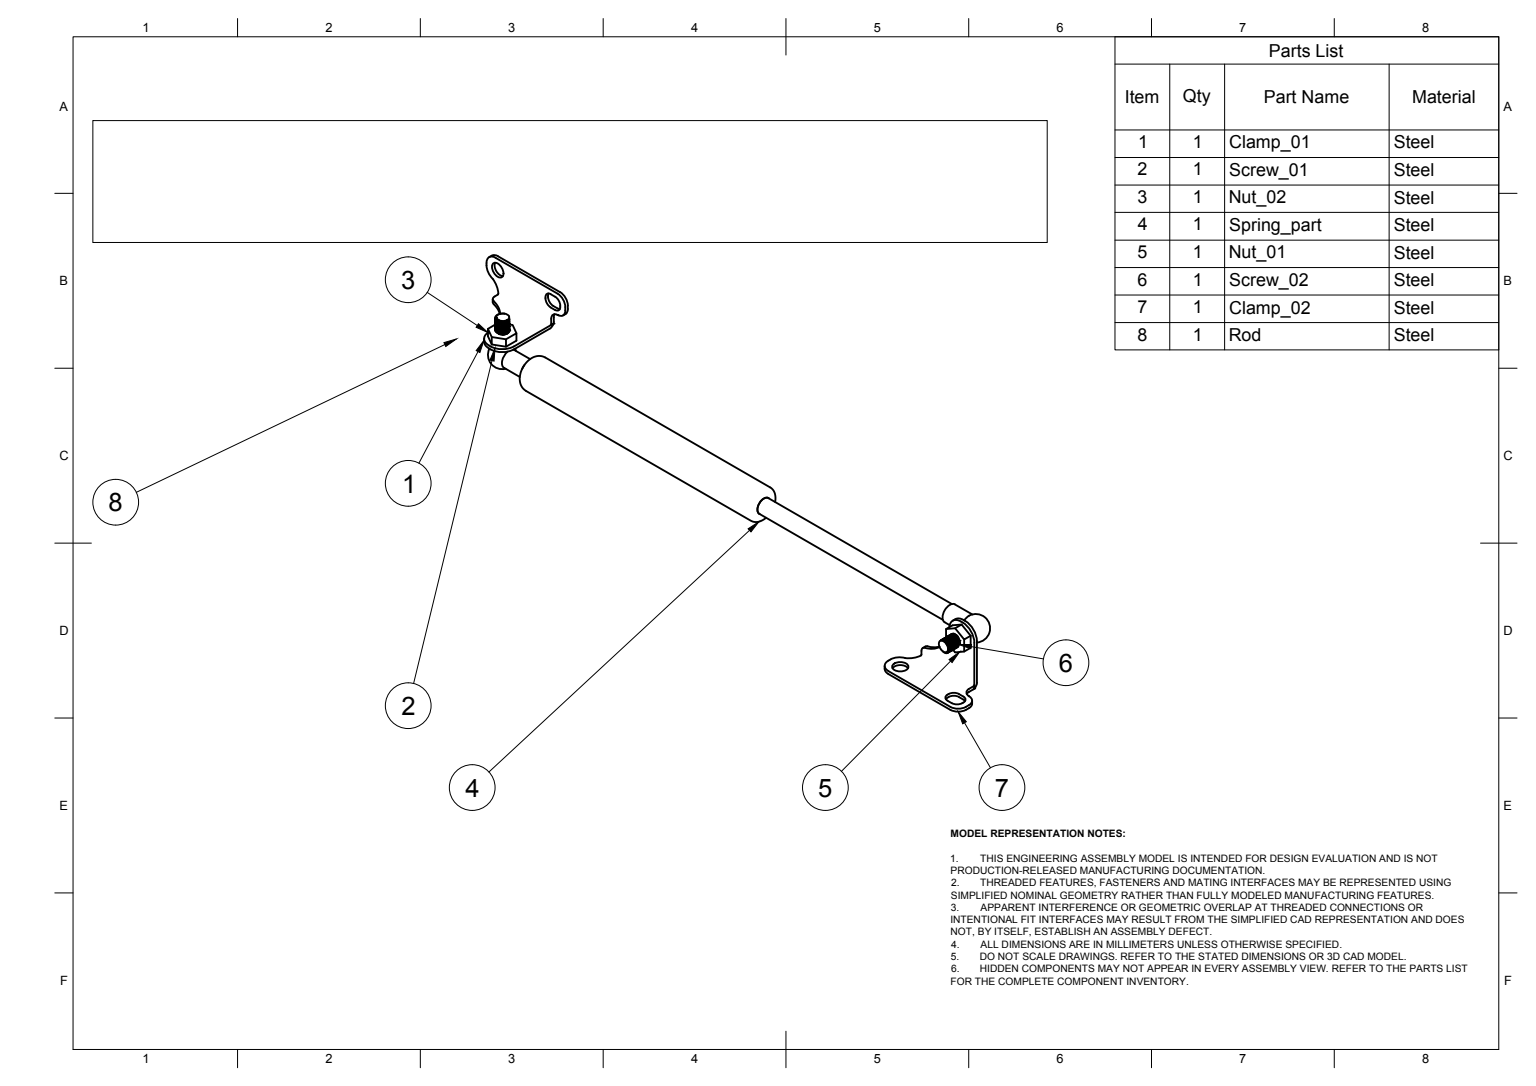
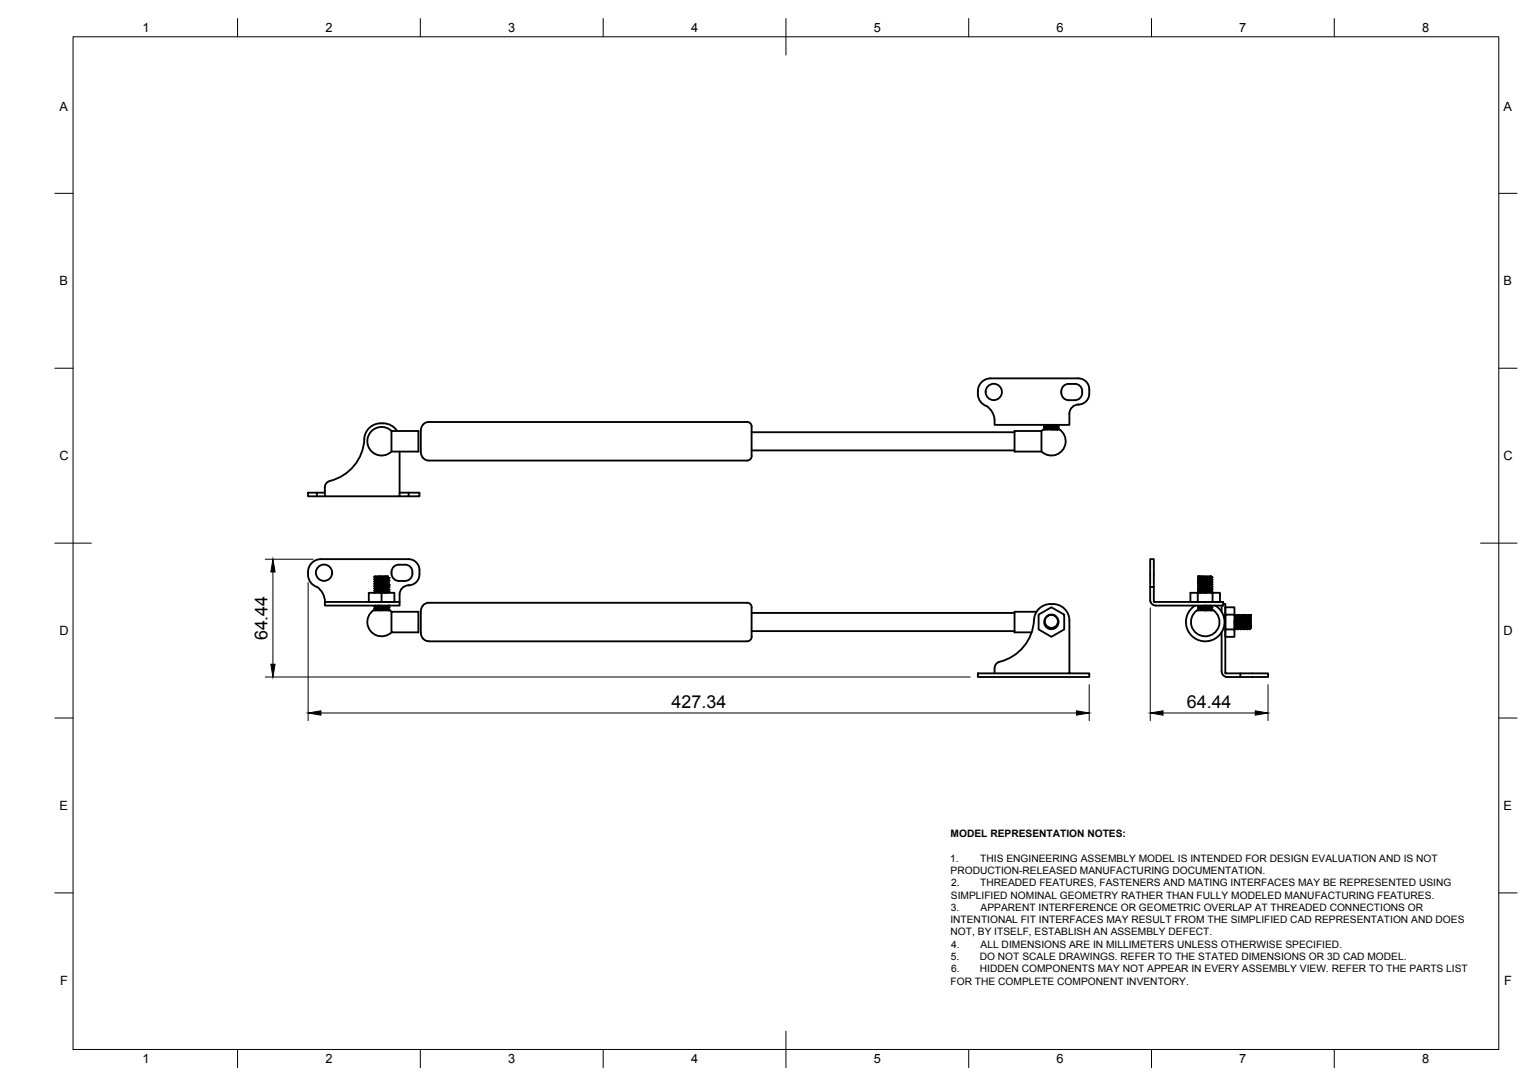
ISO-10303-21;
HEADER;
/* Generated by software containing ST-Developer
 * from STEP Tools, Inc. (www.steptools.com) 
 */

FILE_DESCRIPTION(
/* description */ (''),
/* implementation_level */ '2;1');

FILE_NAME(
/* name */ 'BR-107',
/* time_stamp */ '2026-10-04T16:49:01-07:00',
/* author */ (''),
/* organization */ (''),
/* preprocessor_version */ 'ST-DEVELOPER v20.2',
/* originating_system */ 'Autodesk Translation Framework v15.15.0.0',
/* authorisation */ '');

FILE_SCHEMA (('AUTOMOTIVE_DESIGN { 1 0 10303 214 3 1 1 }'));
ENDSEC;

DATA;
#10=MECHANICAL_DESIGN_GEOMETRIC_PRESENTATION_REPRESENTATION('',(#80,#81,
#82,#83,#84,#85,#86,#87,#88),#51553);
#11=ITEM_DEFINED_TRANSFORMATION($,$,#4358,#4663);
#12=ITEM_DEFINED_TRANSFORMATION($,$,#4430,#4664);
#13=ITEM_DEFINED_TRANSFORMATION($,$,#4466,#4665);
#14=ITEM_DEFINED_TRANSFORMATION($,$,#4489,#4666);
#15=ITEM_DEFINED_TRANSFORMATION($,$,#4507,#4667);
#16=ITEM_DEFINED_TRANSFORMATION($,$,#4530,#4668);
#17=ITEM_DEFINED_TRANSFORMATION($,$,#4559,#4669);
#18=ITEM_DEFINED_TRANSFORMATION($,$,#4631,#4670);
#19=(
REPRESENTATION_RELATIONSHIP($,$,#51585,#51584)
REPRESENTATION_RELATIONSHIP_WITH_TRANSFORMATION(#11)
SHAPE_REPRESENTATION_RELATIONSHIP()
);
#20=(
REPRESENTATION_RELATIONSHIP($,$,#51586,#51584)
REPRESENTATION_RELATIONSHIP_WITH_TRANSFORMATION(#12)
SHAPE_REPRESENTATION_RELATIONSHIP()
);
#21=(
REPRESENTATION_RELATIONSHIP($,$,#51587,#51584)
REPRESENTATION_RELATIONSHIP_WITH_TRANSFORMATION(#13)
SHAPE_REPRESENTATION_RELATIONSHIP()
);
#22=(
REPRESENTATION_RELATIONSHIP($,$,#51588,#51584)
REPRESENTATION_RELATIONSHIP_WITH_TRANSFORMATION(#14)
SHAPE_REPRESENTATION_RELATIONSHIP()
);
#23=(
REPRESENTATION_RELATIONSHIP($,$,#51589,#51584)
REPRESENTATION_RELATIONSHIP_WITH_TRANSFORMATION(#15)
SHAPE_REPRESENTATION_RELATIONSHIP()
);
#24=(
REPRESENTATION_RELATIONSHIP($,$,#51590,#51584)
REPRESENTATION_RELATIONSHIP_WITH_TRANSFORMATION(#16)
SHAPE_REPRESENTATION_RELATIONSHIP()
);
#25=(
REPRESENTATION_RELATIONSHIP($,$,#51591,#51584)
REPRESENTATION_RELATIONSHIP_WITH_TRANSFORMATION(#17)
SHAPE_REPRESENTATION_RELATIONSHIP()
);
#26=(
REPRESENTATION_RELATIONSHIP($,$,#51592,#51584)
REPRESENTATION_RELATIONSHIP_WITH_TRANSFORMATION(#18)
SHAPE_REPRESENTATION_RELATIONSHIP()
);
#27=CONTEXT_DEPENDENT_SHAPE_REPRESENTATION(#19,#51576);
#28=CONTEXT_DEPENDENT_SHAPE_REPRESENTATION(#20,#51577);
#29=CONTEXT_DEPENDENT_SHAPE_REPRESENTATION(#21,#51578);
#30=CONTEXT_DEPENDENT_SHAPE_REPRESENTATION(#22,#51579);
#31=CONTEXT_DEPENDENT_SHAPE_REPRESENTATION(#23,#51580);
#32=CONTEXT_DEPENDENT_SHAPE_REPRESENTATION(#24,#51581);
#33=CONTEXT_DEPENDENT_SHAPE_REPRESENTATION(#25,#51582);
#34=CONTEXT_DEPENDENT_SHAPE_REPRESENTATION(#26,#51583);
#35=NEXT_ASSEMBLY_USAGE_OCCURRENCE('Clamp_01:1','Clamp_01:1',
'Clamp_01:1',#51594,#51595,'Clamp_01:1');
#36=NEXT_ASSEMBLY_USAGE_OCCURRENCE('Screw_01:1','Screw_01:1',
'Screw_01:1',#51594,#51596,'Screw_01:1');
#37=NEXT_ASSEMBLY_USAGE_OCCURRENCE('Nut_02:1','Nut_02:1','Nut_02:1',#51594,
#51597,'Nut_02:1');
#38=NEXT_ASSEMBLY_USAGE_OCCURRENCE('Spring_part:1','Spring_part:1',
'Spring_part:1',#51594,#51598,'Spring_part:1');
#39=NEXT_ASSEMBLY_USAGE_OCCURRENCE('Nut_01:1','Nut_01:1','Nut_01:1',#51594,
#51599,'Nut_01:1');
#40=NEXT_ASSEMBLY_USAGE_OCCURRENCE('Screw_02:1','Screw_02:1',
'Screw_02:1',#51594,#51600,'Screw_02:1');
#41=NEXT_ASSEMBLY_USAGE_OCCURRENCE('Clamp_02:1','Clamp_02:1',
'Clamp_02:1',#51594,#51601,'Clamp_02:1');
#42=NEXT_ASSEMBLY_USAGE_OCCURRENCE('Rod:1','Rod:1','Rod:1',#51594,#51602,
'Rod:1');
#43=SPHERICAL_SURFACE('',#4646,7.81234603703673);
#44=SPHERICAL_SURFACE('',#4651,7.81234603703673);
#45=TOROIDAL_SURFACE('',#4496,8.03882147643231,2.49999999999996);
#46=TOROIDAL_SURFACE('',#4502,5.78096926885271,5.05765846207533);
#47=TOROIDAL_SURFACE('',#4505,6.2888214764323,4.24999999999998);
#48=B_SPLINE_SURFACE_WITH_KNOTS('',3,3,((#17982,#17983,#17984,#17985,#17986,
#17987,#17988,#17989,#17990,#17991,#17992,#17993,#17994,#17995,#17996,#17997,
#17998,#17999,#18000,#18001,#18002,#18003,#18004,#18005,#18006,#18007,#18008,
#18009,#18010,#18011,#18012,#18013,#18014,#18015,#18016,#18017,#18018,#18019,
#18020,#18021,#18022,#18023,#18024,#18025,#18026,#18027,#18028,#18029,#18030,
#18031,#18032,#18033,#18034,#18035,#18036,#18037,#18038,#18039,#18040,#18041,
#18042,#18043,#18044,#18045,#18046,#18047,#18048,#18049,#18050,#18051,#18052,
#18053,#18054,#18055,#18056,#18057,#18058,#18059,#18060,#18061,#18062,#18063,
#18064,#18065,#18066,#18067,#18068,#18069,#18070,#18071,#18072,#18073,#18074,
#18075,#18076,#18077,#18078,#18079,#18080,#18081,#18082,#18083,#18084,#18085,
#18086,#18087,#18088,#18089,#18090,#18091,#18092,#18093,#18094,#18095,#18096,
#18097,#18098,#18099,#18100,#18101,#18102,#18103,#18104,#18105,#18106,#18107,
#18108,#18109,#18110,#18111,#18112),(#18113,#18114,#18115,#18116,#18117,
#18118,#18119,#18120,#18121,#18122,#18123,#18124,#18125,#18126,#18127,#18128,
#18129,#18130,#18131,#18132,#18133,#18134,#18135,#18136,#18137,#18138,#18139,
#18140,#18141,#18142,#18143,#18144,#18145,#18146,#18147,#18148,#18149,#18150,
#18151,#18152,#18153,#18154,#18155,#18156,#18157,#18158,#18159,#18160,#18161,
#18162,#18163,#18164,#18165,#18166,#18167,#18168,#18169,#18170,#18171,#18172,
#18173,#18174,#18175,#18176,#18177,#18178,#18179,#18180,#18181,#18182,#18183,
#18184,#18185,#18186,#18187,#18188,#18189,#18190,#18191,#18192,#18193,#18194,
#18195,#18196,#18197,#18198,#18199,#18200,#18201,#18202,#18203,#18204,#18205,
#18206,#18207,#18208,#18209,#18210,#18211,#18212,#18213,#18214,#18215,#18216,
#18217,#18218,#18219,#18220,#18221,#18222,#18223,#18224,#18225,#18226,#18227,
#18228,#18229,#18230,#18231,#18232,#18233,#18234,#18235,#18236,#18237,#18238,
#18239,#18240,#18241,#18242,#18243),(#18244,#18245,#18246,#18247,#18248,
#18249,#18250,#18251,#18252,#18253,#18254,#18255,#18256,#18257,#18258,#18259,
#18260,#18261,#18262,#18263,#18264,#18265,#18266,#18267,#18268,#18269,#18270,
#18271,#18272,#18273,#18274,#18275,#18276,#18277,#18278,#18279,#18280,#18281,
#18282,#18283,#18284,#18285,#18286,#18287,#18288,#18289,#18290,#18291,#18292,
#18293,#18294,#18295,#18296,#18297,#18298,#18299,#18300,#18301,#18302,#18303,
#18304,#18305,#18306,#18307,#18308,#18309,#18310,#18311,#18312,#18313,#18314,
#18315,#18316,#18317,#18318,#18319,#18320,#18321,#18322,#18323,#18324,#18325,
#18326,#18327,#18328,#18329,#18330,#18331,#18332,#18333,#18334,#18335,#18336,
#18337,#18338,#18339,#18340,#18341,#18342,#18343,#18344,#18345,#18346,#18347,
#18348,#18349,#18350,#18351,#18352,#18353,#18354,#18355,#18356,#18357,#18358,
#18359,#18360,#18361,#18362,#18363,#18364,#18365,#18366,#18367,#18368,#18369,
#18370,#18371,#18372,#18373,#18374),(#18375,#18376,#18377,#18378,#18379,
#18380,#18381,#18382,#18383,#18384,#18385,#18386,#18387,#18388,#18389,#18390,
#18391,#18392,#18393,#18394,#18395,#18396,#18397,#18398,#18399,#18400,#18401,
#18402,#18403,#18404,#18405,#18406,#18407,#18408,#18409,#18410,#18411,#18412,
#18413,#18414,#18415,#18416,#18417,#18418,#18419,#18420,#18421,#18422,#18423,
#18424,#18425,#18426,#18427,#18428,#18429,#18430,#18431,#18432,#18433,#18434,
#18435,#18436,#18437,#18438,#18439,#18440,#18441,#18442,#18443,#18444,#18445,
#18446,#18447,#18448,#18449,#18450,#18451,#18452,#18453,#18454,#18455,#18456,
#18457,#18458,#18459,#18460,#18461,#18462,#18463,#18464,#18465,#18466,#18467,
#18468,#18469,#18470,#18471,#18472,#18473,#18474,#18475,#18476,#18477,#18478,
#18479,#18480,#18481,#18482,#18483,#18484,#18485,#18486,#18487,#18488,#18489,
#18490,#18491,#18492,#18493,#18494,#18495,#18496,#18497,#18498,#18499,#18500,
#18501,#18502,#18503,#18504,#18505)),.UNSPECIFIED.,.F.,.F.,.F.,(4,4),(4,
1,1,1,1,1,1,1,1,1,1,1,1,1,1,1,1,1,1,1,1,1,1,1,1,1,1,1,1,1,1,1,1,1,1,1,1,
1,1,1,1,1,1,1,1,1,1,1,1,1,1,1,1,1,1,1,1,1,1,1,1,1,1,1,1,1,1,1,1,1,1,1,1,
1,1,1,1,1,1,1,1,1,1,1,1,1,1,1,1,1,1,1,1,1,1,1,1,1,1,1,1,1,1,1,1,1,1,1,1,
1,1,1,1,1,1,1,1,1,1,1,1,1,1,1,1,1,1,1,4),(-0.000314077148181808,0.0826777824702824),
(11.6145490510227,12.613065069482,13.6109159112094,14.6087667529368,15.6066175946642,
16.6044684363917,17.6023192781191,18.6001701198465,19.5980209615739,20.5958718033013,
21.5937226450287,22.5915734867561,23.5894243284835,24.5872751702109,25.5851260119383,
26.5829768536657,27.5808276953931,28.5786785371205,29.5765293788479,30.5743802205753,
31.5722310623027,32.5700819040301,33.5679327457575,34.5657835874849,35.5636344292123,
36.5614852709397,37.5593361126671,38.5571869543945,39.5550377961219,40.5528886378493,
41.5507394795767,42.5485903213041,43.5464411630315,44.5442920047589,45.5421428464863,
46.5399936882137,47.5378445299411,48.5356953716685,49.5335462133959,50.5313970551233,
51.5292478968507,52.5270987385781,53.5249495803055,54.522800422033,55.5206512637604,
56.5185021054878,57.5163529472152,58.5142037889426,59.51205463067,60.5099054723974,
61.5077563141248,62.5056071558522,63.5034579975796,64.501308839307,65.4991596810344,
66.4970105227618,67.4948613644892,68.4927122062166,69.490563047944,70.4884138896714,
71.4862647313988,72.4841155731262,73.4819664148536,74.479817256581,75.4776680983084,
76.4755189400358,77.4733697817632,78.4712206234906,79.469071465218,80.4669223069454,
81.4647731486728,82.4626239904002,83.4604748321276,84.458325673855,85.4561765155824,
86.4540273573098,87.4518781990372,88.4497290407646,89.4475798824921,90.4454307242194,
91.4432815659468,92.4411324076742,93.4389832494017,94.4368340911291,95.4346849328565,
96.4325357745839,97.4303866163113,98.4282374580387,99.4260882997661,100.423939141493,
101.421789983221,102.419640824948,103.417491666676,104.415342508403,105.41319335013,
106.411044191858,107.408895033585,108.406745875313,109.40459671704,110.402447558768,
111.400298400495,112.398149242222,113.39600008395,114.393850925677,115.391701767405,
116.389552609132,117.387403450859,118.385254292587,119.383105134314,120.380955976042,
121.378806817769,122.376657659496,123.374508501224,124.372359342951,125.370210184679,
126.368061026406,127.365911868133,128.363762709861,129.361613551588,130.359464393316,
131.357315235043,132.35516607677,133.353016918498,134.350867760225,135.348718601953,
136.34656944368,137.344420285407,138.342271127135,139.340121968862),
 .UNSPECIFIED.);
#49=B_SPLINE_SURFACE_WITH_KNOTS('',3,3,((#18820,#18821,#18822,#18823,#18824,
#18825,#18826,#18827,#18828,#18829,#18830,#18831,#18832,#18833,#18834,#18835,
#18836,#18837,#18838,#18839,#18840,#18841,#18842,#18843,#18844,#18845,#18846,
#18847,#18848,#18849,#18850,#18851,#18852,#18853,#18854,#18855,#18856,#18857,
#18858,#18859,#18860,#18861,#18862,#18863,#18864,#18865,#18866,#18867,#18868,
#18869,#18870,#18871,#18872,#18873,#18874,#18875,#18876,#18877,#18878,#18879,
#18880,#18881,#18882,#18883,#18884,#18885,#18886,#18887,#18888,#18889,#18890,
#18891,#18892,#18893,#18894,#18895,#18896,#18897,#18898,#18899,#18900,#18901,
#18902,#18903,#18904,#18905,#18906,#18907,#18908,#18909,#18910,#18911,#18912,
#18913,#18914,#18915,#18916,#18917,#18918,#18919,#18920,#18921,#18922,#18923,
#18924,#18925,#18926,#18927,#18928,#18929,#18930,#18931,#18932,#18933,#18934,
#18935,#18936,#18937,#18938,#18939,#18940,#18941,#18942,#18943,#18944,#18945,
#18946,#18947,#18948,#18949,#18950),(#18951,#18952,#18953,#18954,#18955,
#18956,#18957,#18958,#18959,#18960,#18961,#18962,#18963,#18964,#18965,#18966,
#18967,#18968,#18969,#18970,#18971,#18972,#18973,#18974,#18975,#18976,#18977,
#18978,#18979,#18980,#18981,#18982,#18983,#18984,#18985,#18986,#18987,#18988,
#18989,#18990,#18991,#18992,#18993,#18994,#18995,#18996,#18997,#18998,#18999,
#19000,#19001,#19002,#19003,#19004,#19005,#19006,#19007,#19008,#19009,#19010,
#19011,#19012,#19013,#19014,#19015,#19016,#19017,#19018,#19019,#19020,#19021,
#19022,#19023,#19024,#19025,#19026,#19027,#19028,#19029,#19030,#19031,#19032,
#19033,#19034,#19035,#19036,#19037,#19038,#19039,#19040,#19041,#19042,#19043,
#19044,#19045,#19046,#19047,#19048,#19049,#19050,#19051,#19052,#19053,#19054,
#19055,#19056,#19057,#19058,#19059,#19060,#19061,#19062,#19063,#19064,#19065,
#19066,#19067,#19068,#19069,#19070,#19071,#19072,#19073,#19074,#19075,#19076,
#19077,#19078,#19079,#19080,#19081),(#19082,#19083,#19084,#19085,#19086,
#19087,#19088,#19089,#19090,#19091,#19092,#19093,#19094,#19095,#19096,#19097,
#19098,#19099,#19100,#19101,#19102,#19103,#19104,#19105,#19106,#19107,#19108,
#19109,#19110,#19111,#19112,#19113,#19114,#19115,#19116,#19117,#19118,#19119,
#19120,#19121,#19122,#19123,#19124,#19125,#19126,#19127,#19128,#19129,#19130,
#19131,#19132,#19133,#19134,#19135,#19136,#19137,#19138,#19139,#19140,#19141,
#19142,#19143,#19144,#19145,#19146,#19147,#19148,#19149,#19150,#19151,#19152,
#19153,#19154,#19155,#19156,#19157,#19158,#19159,#19160,#19161,#19162,#19163,
#19164,#19165,#19166,#19167,#19168,#19169,#19170,#19171,#19172,#19173,#19174,
#19175,#19176,#19177,#19178,#19179,#19180,#19181,#19182,#19183,#19184,#19185,
#19186,#19187,#19188,#19189,#19190,#19191,#19192,#19193,#19194,#19195,#19196,
#19197,#19198,#19199,#19200,#19201,#19202,#19203,#19204,#19205,#19206,#19207,
#19208,#19209,#19210,#19211,#19212),(#19213,#19214,#19215,#19216,#19217,
#19218,#19219,#19220,#19221,#19222,#19223,#19224,#19225,#19226,#19227,#19228,
#19229,#19230,#19231,#19232,#19233,#19234,#19235,#19236,#19237,#19238,#19239,
#19240,#19241,#19242,#19243,#19244,#19245,#19246,#19247,#19248,#19249,#19250,
#19251,#19252,#19253,#19254,#19255,#19256,#19257,#19258,#19259,#19260,#19261,
#19262,#19263,#19264,#19265,#19266,#19267,#19268,#19269,#19270,#19271,#19272,
#19273,#19274,#19275,#19276,#19277,#19278,#19279,#19280,#19281,#19282,#19283,
#19284,#19285,#19286,#19287,#19288,#19289,#19290,#19291,#19292,#19293,#19294,
#19295,#19296,#19297,#19298,#19299,#19300,#19301,#19302,#19303,#19304,#19305,
#19306,#19307,#19308,#19309,#19310,#19311,#19312,#19313,#19314,#19315,#19316,
#19317,#19318,#19319,#19320,#19321,#19322,#19323,#19324,#19325,#19326,#19327,
#19328,#19329,#19330,#19331,#19332,#19333,#19334,#19335,#19336,#19337,#19338,
#19339,#19340,#19341,#19342,#19343)),.UNSPECIFIED.,.F.,.F.,.F.,(4,4),(4,
1,1,1,1,1,1,1,1,1,1,1,1,1,1,1,1,1,1,1,1,1,1,1,1,1,1,1,1,1,1,1,1,1,1,1,1,
1,1,1,1,1,1,1,1,1,1,1,1,1,1,1,1,1,1,1,1,1,1,1,1,1,1,1,1,1,1,1,1,1,1,1,1,
1,1,1,1,1,1,1,1,1,1,1,1,1,1,1,1,1,1,1,1,1,1,1,1,1,1,1,1,1,1,1,1,1,1,1,1,
1,1,1,1,1,1,1,1,1,1,1,1,1,1,1,1,1,1,1,4),(-0.000314077148181808,0.0826777824702824),
(11.6145490510227,12.613065069482,13.6109159112094,14.6087667529368,15.6066175946642,
16.6044684363917,17.6023192781191,18.6001701198465,19.5980209615739,20.5958718033013,
21.5937226450287,22.5915734867561,23.5894243284835,24.5872751702109,25.5851260119383,
26.5829768536657,27.5808276953931,28.5786785371205,29.5765293788479,30.5743802205753,
31.5722310623027,32.5700819040301,33.5679327457575,34.5657835874849,35.5636344292123,
36.5614852709397,37.5593361126671,38.5571869543945,39.5550377961219,40.5528886378493,
41.5507394795767,42.5485903213041,43.5464411630315,44.5442920047589,45.5421428464863,
46.5399936882137,47.5378445299411,48.5356953716685,49.5335462133959,50.5313970551233,
51.5292478968507,52.5270987385781,53.5249495803055,54.522800422033,55.5206512637604,
56.5185021054878,57.5163529472152,58.5142037889426,59.51205463067,60.5099054723974,
61.5077563141248,62.5056071558522,63.5034579975796,64.501308839307,65.4991596810344,
66.4970105227618,67.4948613644892,68.4927122062166,69.490563047944,70.4884138896714,
71.4862647313988,72.4841155731262,73.4819664148536,74.479817256581,75.4776680983084,
76.4755189400358,77.4733697817632,78.4712206234906,79.469071465218,80.4669223069454,
81.4647731486728,82.4626239904002,83.4604748321276,84.458325673855,85.4561765155824,
86.4540273573098,87.4518781990372,88.4497290407646,89.4475798824921,90.4454307242194,
91.4432815659468,92.4411324076742,93.4389832494017,94.4368340911291,95.4346849328565,
96.4325357745839,97.4303866163113,98.4282374580387,99.4260882997661,100.423939141493,
101.421789983221,102.419640824948,103.417491666676,104.415342508403,105.41319335013,
106.411044191858,107.408895033585,108.406745875313,109.40459671704,110.402447558768,
111.400298400495,112.398149242222,113.39600008395,114.393850925677,115.391701767405,
116.389552609132,117.387403450859,118.385254292587,119.383105134314,120.380955976042,
121.378806817769,122.376657659496,123.374508501224,124.372359342951,125.370210184679,
126.368061026406,127.365911868133,128.363762709861,129.361613551588,130.359464393316,
131.357315235043,132.35516607677,133.353016918498,134.350867760225,135.348718601953,
136.34656944368,137.344420285407,138.342271127135,139.340121968862),
 .UNSPECIFIED.);
#50=B_SPLINE_SURFACE_WITH_KNOTS('',3,3,((#19498,#19499,#19500,#19501,#19502,
#19503,#19504,#19505,#19506,#19507,#19508,#19509,#19510,#19511,#19512,#19513,
#19514,#19515,#19516,#19517,#19518,#19519,#19520,#19521,#19522,#19523,#19524,
#19525,#19526,#19527,#19528,#19529,#19530,#19531,#19532,#19533,#19534,#19535,
#19536,#19537,#19538,#19539,#19540,#19541,#19542,#19543,#19544,#19545,#19546,
#19547,#19548,#19549,#19550,#19551,#19552,#19553,#19554,#19555,#19556,#19557,
#19558,#19559,#19560,#19561,#19562,#19563,#19564,#19565,#19566,#19567,#19568,
#19569,#19570,#19571,#19572,#19573,#19574,#19575,#19576,#19577,#19578,#19579,
#19580,#19581,#19582,#19583,#19584,#19585,#19586,#19587,#19588,#19589,#19590,
#19591,#19592,#19593,#19594,#19595,#19596,#19597,#19598,#19599,#19600,#19601,
#19602,#19603,#19604,#19605,#19606,#19607,#19608,#19609,#19610,#19611,#19612,
#19613,#19614,#19615,#19616,#19617,#19618,#19619,#19620,#19621,#19622,#19623,
#19624,#19625,#19626,#19627,#19628),(#19629,#19630,#19631,#19632,#19633,
#19634,#19635,#19636,#19637,#19638,#19639,#19640,#19641,#19642,#19643,#19644,
#19645,#19646,#19647,#19648,#19649,#19650,#19651,#19652,#19653,#19654,#19655,
#19656,#19657,#19658,#19659,#19660,#19661,#19662,#19663,#19664,#19665,#19666,
#19667,#19668,#19669,#19670,#19671,#19672,#19673,#19674,#19675,#19676,#19677,
#19678,#19679,#19680,#19681,#19682,#19683,#19684,#19685,#19686,#19687,#19688,
#19689,#19690,#19691,#19692,#19693,#19694,#19695,#19696,#19697,#19698,#19699,
#19700,#19701,#19702,#19703,#19704,#19705,#19706,#19707,#19708,#19709,#19710,
#19711,#19712,#19713,#19714,#19715,#19716,#19717,#19718,#19719,#19720,#19721,
#19722,#19723,#19724,#19725,#19726,#19727,#19728,#19729,#19730,#19731,#19732,
#19733,#19734,#19735,#19736,#19737,#19738,#19739,#19740,#19741,#19742,#19743,
#19744,#19745,#19746,#19747,#19748,#19749,#19750,#19751,#19752,#19753,#19754,
#19755,#19756,#19757,#19758,#19759),(#19760,#19761,#19762,#19763,#19764,
#19765,#19766,#19767,#19768,#19769,#19770,#19771,#19772,#19773,#19774,#19775,
#19776,#19777,#19778,#19779,#19780,#19781,#19782,#19783,#19784,#19785,#19786,
#19787,#19788,#19789,#19790,#19791,#19792,#19793,#19794,#19795,#19796,#19797,
#19798,#19799,#19800,#19801,#19802,#19803,#19804,#19805,#19806,#19807,#19808,
#19809,#19810,#19811,#19812,#19813,#19814,#19815,#19816,#19817,#19818,#19819,
#19820,#19821,#19822,#19823,#19824,#19825,#19826,#19827,#19828,#19829,#19830,
#19831,#19832,#19833,#19834,#19835,#19836,#19837,#19838,#19839,#19840,#19841,
#19842,#19843,#19844,#19845,#19846,#19847,#19848,#19849,#19850,#19851,#19852,
#19853,#19854,#19855,#19856,#19857,#19858,#19859,#19860,#19861,#19862,#19863,
#19864,#19865,#19866,#19867,#19868,#19869,#19870,#19871,#19872,#19873,#19874,
#19875,#19876,#19877,#19878,#19879,#19880,#19881,#19882,#19883,#19884,#19885,
#19886,#19887,#19888,#19889,#19890),(#19891,#19892,#19893,#19894,#19895,
#19896,#19897,#19898,#19899,#19900,#19901,#19902,#19903,#19904,#19905,#19906,
#19907,#19908,#19909,#19910,#19911,#19912,#19913,#19914,#19915,#19916,#19917,
#19918,#19919,#19920,#19921,#19922,#19923,#19924,#19925,#19926,#19927,#19928,
#19929,#19930,#19931,#19932,#19933,#19934,#19935,#19936,#19937,#19938,#19939,
#19940,#19941,#19942,#19943,#19944,#19945,#19946,#19947,#19948,#19949,#19950,
#19951,#19952,#19953,#19954,#19955,#19956,#19957,#19958,#19959,#19960,#19961,
#19962,#19963,#19964,#19965,#19966,#19967,#19968,#19969,#19970,#19971,#19972,
#19973,#19974,#19975,#19976,#19977,#19978,#19979,#19980,#19981,#19982,#19983,
#19984,#19985,#19986,#19987,#19988,#19989,#19990,#19991,#19992,#19993,#19994,
#19995,#19996,#19997,#19998,#19999,#20000,#20001,#20002,#20003,#20004,#20005,
#20006,#20007,#20008,#20009,#20010,#20011,#20012,#20013,#20014,#20015,#20016,
#20017,#20018,#20019,#20020,#20021)),.UNSPECIFIED.,.F.,.F.,.F.,(4,4),(4,
1,1,1,1,1,1,1,1,1,1,1,1,1,1,1,1,1,1,1,1,1,1,1,1,1,1,1,1,1,1,1,1,1,1,1,1,
1,1,1,1,1,1,1,1,1,1,1,1,1,1,1,1,1,1,1,1,1,1,1,1,1,1,1,1,1,1,1,1,1,1,1,1,
1,1,1,1,1,1,1,1,1,1,1,1,1,1,1,1,1,1,1,1,1,1,1,1,1,1,1,1,1,1,1,1,1,1,1,1,
1,1,1,1,1,1,1,1,1,1,1,1,1,1,1,1,1,1,1,4),(-0.000314077148181808,0.0826777824702824),
(11.6145490510227,12.613065069482,13.6109159112094,14.6087667529368,15.6066175946642,
16.6044684363917,17.6023192781191,18.6001701198465,19.5980209615739,20.5958718033013,
21.5937226450287,22.5915734867561,23.5894243284835,24.5872751702109,25.5851260119383,
26.5829768536657,27.5808276953931,28.5786785371205,29.5765293788479,30.5743802205753,
31.5722310623027,32.5700819040301,33.5679327457575,34.5657835874849,35.5636344292123,
36.5614852709397,37.5593361126671,38.5571869543945,39.5550377961219,40.5528886378493,
41.5507394795767,42.5485903213041,43.5464411630315,44.5442920047589,45.5421428464863,
46.5399936882137,47.5378445299411,48.5356953716685,49.5335462133959,50.5313970551233,
51.5292478968507,52.5270987385781,53.5249495803055,54.522800422033,55.5206512637604,
56.5185021054878,57.5163529472152,58.5142037889426,59.51205463067,60.5099054723974,
61.5077563141248,62.5056071558522,63.5034579975796,64.501308839307,65.4991596810344,
66.4970105227618,67.4948613644892,68.4927122062166,69.490563047944,70.4884138896714,
71.4862647313988,72.4841155731262,73.4819664148536,74.479817256581,75.4776680983084,
76.4755189400358,77.4733697817632,78.4712206234906,79.469071465218,80.4669223069454,
81.4647731486728,82.4626239904002,83.4604748321276,84.458325673855,85.4561765155824,
86.4540273573098,87.4518781990372,88.4497290407646,89.4475798824921,90.4454307242194,
91.4432815659468,92.4411324076742,93.4389832494017,94.4368340911291,95.4346849328565,
96.4325357745839,97.4303866163113,98.4282374580387,99.4260882997661,100.423939141493,
101.421789983221,102.419640824948,103.417491666676,104.415342508403,105.41319335013,
106.411044191858,107.408895033585,108.406745875313,109.40459671704,110.402447558768,
111.400298400495,112.398149242222,113.39600008395,114.393850925677,115.391701767405,
116.389552609132,117.387403450859,118.385254292587,119.383105134314,120.380955976042,
121.378806817769,122.376657659496,123.374508501224,124.372359342951,125.370210184679,
126.368061026406,127.365911868133,128.363762709861,129.361613551588,130.359464393316,
131.357315235043,132.35516607677,133.353016918498,134.350867760225,135.348718601953,
136.34656944368,137.344420285407,138.342271127135,139.340121968862),
 .UNSPECIFIED.);
#51=B_SPLINE_SURFACE_WITH_KNOTS('',3,3,((#20214,#20215,#20216,#20217,#20218,
#20219,#20220,#20221,#20222,#20223,#20224,#20225,#20226,#20227,#20228,#20229,
#20230,#20231,#20232,#20233,#20234,#20235,#20236,#20237,#20238,#20239,#20240,
#20241,#20242,#20243,#20244,#20245,#20246,#20247,#20248,#20249,#20250,#20251,
#20252,#20253,#20254,#20255,#20256,#20257,#20258,#20259,#20260,#20261,#20262,
#20263,#20264,#20265,#20266,#20267,#20268,#20269,#20270,#20271,#20272,#20273,
#20274,#20275,#20276,#20277,#20278,#20279,#20280,#20281,#20282,#20283,#20284,
#20285,#20286,#20287,#20288,#20289,#20290,#20291,#20292,#20293,#20294,#20295,
#20296,#20297,#20298,#20299,#20300,#20301,#20302,#20303,#20304,#20305,#20306,
#20307,#20308,#20309,#20310,#20311,#20312,#20313,#20314,#20315,#20316,#20317,
#20318,#20319,#20320,#20321,#20322,#20323,#20324,#20325,#20326,#20327,#20328,
#20329,#20330,#20331,#20332,#20333,#20334,#20335,#20336,#20337,#20338,#20339,
#20340,#20341,#20342,#20343,#20344),(#20345,#20346,#20347,#20348,#20349,
#20350,#20351,#20352,#20353,#20354,#20355,#20356,#20357,#20358,#20359,#20360,
#20361,#20362,#20363,#20364,#20365,#20366,#20367,#20368,#20369,#20370,#20371,
#20372,#20373,#20374,#20375,#20376,#20377,#20378,#20379,#20380,#20381,#20382,
#20383,#20384,#20385,#20386,#20387,#20388,#20389,#20390,#20391,#20392,#20393,
#20394,#20395,#20396,#20397,#20398,#20399,#20400,#20401,#20402,#20403,#20404,
#20405,#20406,#20407,#20408,#20409,#20410,#20411,#20412,#20413,#20414,#20415,
#20416,#20417,#20418,#20419,#20420,#20421,#20422,#20423,#20424,#20425,#20426,
#20427,#20428,#20429,#20430,#20431,#20432,#20433,#20434,#20435,#20436,#20437,
#20438,#20439,#20440,#20441,#20442,#20443,#20444,#20445,#20446,#20447,#20448,
#20449,#20450,#20451,#20452,#20453,#20454,#20455,#20456,#20457,#20458,#20459,
#20460,#20461,#20462,#20463,#20464,#20465,#20466,#20467,#20468,#20469,#20470,
#20471,#20472,#20473,#20474,#20475),(#20476,#20477,#20478,#20479,#20480,
#20481,#20482,#20483,#20484,#20485,#20486,#20487,#20488,#20489,#20490,#20491,
#20492,#20493,#20494,#20495,#20496,#20497,#20498,#20499,#20500,#20501,#20502,
#20503,#20504,#20505,#20506,#20507,#20508,#20509,#20510,#20511,#20512,#20513,
#20514,#20515,#20516,#20517,#20518,#20519,#20520,#20521,#20522,#20523,#20524,
#20525,#20526,#20527,#20528,#20529,#20530,#20531,#20532,#20533,#20534,#20535,
#20536,#20537,#20538,#20539,#20540,#20541,#20542,#20543,#20544,#20545,#20546,
#20547,#20548,#20549,#20550,#20551,#20552,#20553,#20554,#20555,#20556,#20557,
#20558,#20559,#20560,#20561,#20562,#20563,#20564,#20565,#20566,#20567,#20568,
#20569,#20570,#20571,#20572,#20573,#20574,#20575,#20576,#20577,#20578,#20579,
#20580,#20581,#20582,#20583,#20584,#20585,#20586,#20587,#20588,#20589,#20590,
#20591,#20592,#20593,#20594,#20595,#20596,#20597,#20598,#20599,#20600,#20601,
#20602,#20603,#20604,#20605,#20606),(#20607,#20608,#20609,#20610,#20611,
#20612,#20613,#20614,#20615,#20616,#20617,#20618,#20619,#20620,#20621,#20622,
#20623,#20624,#20625,#20626,#20627,#20628,#20629,#20630,#20631,#20632,#20633,
#20634,#20635,#20636,#20637,#20638,#20639,#20640,#20641,#20642,#20643,#20644,
#20645,#20646,#20647,#20648,#20649,#20650,#20651,#20652,#20653,#20654,#20655,
#20656,#20657,#20658,#20659,#20660,#20661,#20662,#20663,#20664,#20665,#20666,
#20667,#20668,#20669,#20670,#20671,#20672,#20673,#20674,#20675,#20676,#20677,
#20678,#20679,#20680,#20681,#20682,#20683,#20684,#20685,#20686,#20687,#20688,
#20689,#20690,#20691,#20692,#20693,#20694,#20695,#20696,#20697,#20698,#20699,
#20700,#20701,#20702,#20703,#20704,#20705,#20706,#20707,#20708,#20709,#20710,
#20711,#20712,#20713,#20714,#20715,#20716,#20717,#20718,#20719,#20720,#20721,
#20722,#20723,#20724,#20725,#20726,#20727,#20728,#20729,#20730,#20731,#20732,
#20733,#20734,#20735,#20736,#20737)),.UNSPECIFIED.,.F.,.F.,.F.,(4,4),(4,
1,1,1,1,1,1,1,1,1,1,1,1,1,1,1,1,1,1,1,1,1,1,1,1,1,1,1,1,1,1,1,1,1,1,1,1,
1,1,1,1,1,1,1,1,1,1,1,1,1,1,1,1,1,1,1,1,1,1,1,1,1,1,1,1,1,1,1,1,1,1,1,1,
1,1,1,1,1,1,1,1,1,1,1,1,1,1,1,1,1,1,1,1,1,1,1,1,1,1,1,1,1,1,1,1,1,1,1,1,
1,1,1,1,1,1,1,1,1,1,1,1,1,1,1,1,1,1,1,4),(-0.000314077148181808,0.0826777824702824),
(11.6145490510227,12.613065069482,13.6109159112094,14.6087667529368,15.6066175946642,
16.6044684363917,17.6023192781191,18.6001701198465,19.5980209615739,20.5958718033013,
21.5937226450287,22.5915734867561,23.5894243284835,24.5872751702109,25.5851260119383,
26.5829768536657,27.5808276953931,28.5786785371205,29.5765293788479,30.5743802205753,
31.5722310623027,32.5700819040301,33.5679327457575,34.5657835874849,35.5636344292123,
36.5614852709397,37.5593361126671,38.5571869543945,39.5550377961219,40.5528886378493,
41.5507394795767,42.5485903213041,43.5464411630315,44.5442920047589,45.5421428464863,
46.5399936882137,47.5378445299411,48.5356953716685,49.5335462133959,50.5313970551233,
51.5292478968507,52.5270987385781,53.5249495803055,54.522800422033,55.5206512637604,
56.5185021054878,57.5163529472152,58.5142037889426,59.51205463067,60.5099054723974,
61.5077563141248,62.5056071558522,63.5034579975796,64.501308839307,65.4991596810344,
66.4970105227618,67.4948613644892,68.4927122062166,69.490563047944,70.4884138896714,
71.4862647313988,72.4841155731262,73.4819664148536,74.479817256581,75.4776680983084,
76.4755189400358,77.4733697817632,78.4712206234906,79.469071465218,80.4669223069454,
81.4647731486728,82.4626239904002,83.4604748321276,84.458325673855,85.4561765155824,
86.4540273573098,87.4518781990372,88.4497290407646,89.4475798824921,90.4454307242194,
91.4432815659468,92.4411324076742,93.4389832494017,94.4368340911291,95.4346849328565,
96.4325357745839,97.4303866163113,98.4282374580387,99.4260882997661,100.423939141493,
101.421789983221,102.419640824948,103.417491666676,104.415342508403,105.41319335013,
106.411044191858,107.408895033585,108.406745875313,109.40459671704,110.402447558768,
111.400298400495,112.398149242222,113.39600008395,114.393850925677,115.391701767405,
116.389552609132,117.387403450859,118.385254292587,119.383105134314,120.380955976042,
121.378806817769,122.376657659496,123.374508501224,124.372359342951,125.370210184679,
126.368061026406,127.365911868133,128.363762709861,129.361613551588,130.359464393316,
131.357315235043,132.35516607677,133.353016918498,134.350867760225,135.348718601953,
136.34656944368,137.344420285407,138.342271127135,139.340121968862),
 .UNSPECIFIED.);
#52=B_SPLINE_SURFACE_WITH_KNOTS('',3,3,((#21566,#21567,#21568,#21569,#21570,
#21571,#21572,#21573,#21574,#21575,#21576,#21577,#21578,#21579,#21580,#21581,
#21582,#21583,#21584,#21585,#21586,#21587,#21588,#21589,#21590,#21591,#21592,
#21593,#21594,#21595,#21596,#21597,#21598,#21599,#21600,#21601,#21602,#21603,
#21604,#21605,#21606,#21607,#21608,#21609,#21610,#21611,#21612,#21613,#21614,
#21615,#21616,#21617,#21618,#21619,#21620,#21621,#21622,#21623,#21624,#21625,
#21626,#21627,#21628,#21629,#21630,#21631,#21632,#21633,#21634,#21635,#21636,
#21637,#21638,#21639,#21640,#21641,#21642,#21643,#21644,#21645,#21646,#21647,
#21648,#21649,#21650,#21651,#21652,#21653,#21654,#21655,#21656,#21657,#21658,
#21659,#21660,#21661,#21662,#21663,#21664,#21665,#21666,#21667,#21668,#21669,
#21670,#21671,#21672,#21673,#21674,#21675,#21676,#21677,#21678,#21679,#21680,
#21681,#21682,#21683,#21684,#21685,#21686,#21687,#21688,#21689,#21690,#21691,
#21692,#21693,#21694,#21695,#21696),(#21697,#21698,#21699,#21700,#21701,
#21702,#21703,#21704,#21705,#21706,#21707,#21708,#21709,#21710,#21711,#21712,
#21713,#21714,#21715,#21716,#21717,#21718,#21719,#21720,#21721,#21722,#21723,
#21724,#21725,#21726,#21727,#21728,#21729,#21730,#21731,#21732,#21733,#21734,
#21735,#21736,#21737,#21738,#21739,#21740,#21741,#21742,#21743,#21744,#21745,
#21746,#21747,#21748,#21749,#21750,#21751,#21752,#21753,#21754,#21755,#21756,
#21757,#21758,#21759,#21760,#21761,#21762,#21763,#21764,#21765,#21766,#21767,
#21768,#21769,#21770,#21771,#21772,#21773,#21774,#21775,#21776,#21777,#21778,
#21779,#21780,#21781,#21782,#21783,#21784,#21785,#21786,#21787,#21788,#21789,
#21790,#21791,#21792,#21793,#21794,#21795,#21796,#21797,#21798,#21799,#21800,
#21801,#21802,#21803,#21804,#21805,#21806,#21807,#21808,#21809,#21810,#21811,
#21812,#21813,#21814,#21815,#21816,#21817,#21818,#21819,#21820,#21821,#21822,
#21823,#21824,#21825,#21826,#21827),(#21828,#21829,#21830,#21831,#21832,
#21833,#21834,#21835,#21836,#21837,#21838,#21839,#21840,#21841,#21842,#21843,
#21844,#21845,#21846,#21847,#21848,#21849,#21850,#21851,#21852,#21853,#21854,
#21855,#21856,#21857,#21858,#21859,#21860,#21861,#21862,#21863,#21864,#21865,
#21866,#21867,#21868,#21869,#21870,#21871,#21872,#21873,#21874,#21875,#21876,
#21877,#21878,#21879,#21880,#21881,#21882,#21883,#21884,#21885,#21886,#21887,
#21888,#21889,#21890,#21891,#21892,#21893,#21894,#21895,#21896,#21897,#21898,
#21899,#21900,#21901,#21902,#21903,#21904,#21905,#21906,#21907,#21908,#21909,
#21910,#21911,#21912,#21913,#21914,#21915,#21916,#21917,#21918,#21919,#21920,
#21921,#21922,#21923,#21924,#21925,#21926,#21927,#21928,#21929,#21930,#21931,
#21932,#21933,#21934,#21935,#21936,#21937,#21938,#21939,#21940,#21941,#21942,
#21943,#21944,#21945,#21946,#21947,#21948,#21949,#21950,#21951,#21952,#21953,
#21954,#21955,#21956,#21957,#21958),(#21959,#21960,#21961,#21962,#21963,
#21964,#21965,#21966,#21967,#21968,#21969,#21970,#21971,#21972,#21973,#21974,
#21975,#21976,#21977,#21978,#21979,#21980,#21981,#21982,#21983,#21984,#21985,
#21986,#21987,#21988,#21989,#21990,#21991,#21992,#21993,#21994,#21995,#21996,
#21997,#21998,#21999,#22000,#22001,#22002,#22003,#22004,#22005,#22006,#22007,
#22008,#22009,#22010,#22011,#22012,#22013,#22014,#22015,#22016,#22017,#22018,
#22019,#22020,#22021,#22022,#22023,#22024,#22025,#22026,#22027,#22028,#22029,
#22030,#22031,#22032,#22033,#22034,#22035,#22036,#22037,#22038,#22039,#22040,
#22041,#22042,#22043,#22044,#22045,#22046,#22047,#22048,#22049,#22050,#22051,
#22052,#22053,#22054,#22055,#22056,#22057,#22058,#22059,#22060,#22061,#22062,
#22063,#22064,#22065,#22066,#22067,#22068,#22069,#22070,#22071,#22072,#22073,
#22074,#22075,#22076,#22077,#22078,#22079,#22080,#22081,#22082,#22083,#22084,
#22085,#22086,#22087,#22088,#22089)),.UNSPECIFIED.,.F.,.F.,.F.,(4,4),(4,
1,1,1,1,1,1,1,1,1,1,1,1,1,1,1,1,1,1,1,1,1,1,1,1,1,1,1,1,1,1,1,1,1,1,1,1,
1,1,1,1,1,1,1,1,1,1,1,1,1,1,1,1,1,1,1,1,1,1,1,1,1,1,1,1,1,1,1,1,1,1,1,1,
1,1,1,1,1,1,1,1,1,1,1,1,1,1,1,1,1,1,1,1,1,1,1,1,1,1,1,1,1,1,1,1,1,1,1,1,
1,1,1,1,1,1,1,1,1,1,1,1,1,1,1,1,1,1,1,4),(-0.000646252380093648,0.082354798859151),
(8.31473274985794,9.31258359158534,10.3104344333127,11.3082852750401,12.3061361167675,
13.3039869584949,14.3018378002224,15.2996886419498,16.2975394836772,17.2953903254046,
18.293241167132,19.2910920088594,20.2889428505868,21.2867936923142,22.2846445340416,
23.282495375769,24.2803462174964,25.2781970592238,26.2760479009512,27.2738987426786,
28.271749584406,29.2696004261334,30.2674512678608,31.2653021095882,32.2631529513156,
33.261003793043,34.2588546347704,35.2567054764978,36.2545563182252,37.2524071599526,
38.25025800168,39.2481088434074,40.2459596851348,41.2438105268622,42.2416613685896,
43.239512210317,44.2373630520444,45.2352138937718,46.2330647354992,47.2309155772266,
48.228766418954,49.2266172606814,50.2244681024088,51.2223189441362,52.2201697858636,
53.218020627591,54.2158714693185,55.2137223110459,56.2115731527733,57.2094239945007,
58.2072748362281,59.2051256779555,60.2029765196829,61.2008273614103,62.1986782031377,
63.1965290448651,64.1943798865925,65.1922307283199,66.1900815700473,67.1879324117747,
68.1857832535021,69.1836340952295,70.1814849369569,71.1793357786843,72.1771866204117,
73.1750374621391,74.1728883038665,75.1707391455939,76.1685899873213,77.1664408290487,
78.1642916707761,79.1621425125035,80.1599933542309,81.1578441959583,82.1556950376857,
83.1535458794131,84.1513967211405,85.1492475628679,86.1470984045953,87.1449492463227,
88.1428000880501,89.1406509297776,90.1385017715049,91.1363526132323,92.1342034549598,
93.1320542966872,94.1299051384146,95.127755980142,96.1256068218694,97.1234576635968,
98.1213085053242,99.1191593470516,100.117010188779,101.114861030506,102.112711872234,
103.110562713961,104.108413555689,105.106264397416,106.104115239143,107.101966080871,
108.099816922598,109.097667764326,110.095518606053,111.09336944778,112.091220289508,
113.089071131235,114.086921972963,115.08477281469,116.082623656417,117.080474498145,
118.078325339872,119.0761761816,120.074027023327,121.071877865054,122.069728706782,
123.067579548509,124.065430390237,125.063281231964,126.061132073691,127.058982915419,
128.056833757146,129.054684598874,130.052535440601,131.050386282328,132.048237124056,
133.046087965783,134.043938807511,135.041789649238,136.040286743345),
 .UNSPECIFIED.);
#53=B_SPLINE_SURFACE_WITH_KNOTS('',3,3,((#22184,#22185,#22186,#22187,#22188,
#22189,#22190,#22191,#22192,#22193,#22194,#22195,#22196,#22197,#22198,#22199,
#22200,#22201,#22202,#22203,#22204,#22205,#22206,#22207,#22208,#22209,#22210,
#22211,#22212,#22213,#22214,#22215,#22216,#22217,#22218,#22219,#22220,#22221,
#22222,#22223,#22224,#22225,#22226,#22227,#22228,#22229,#22230,#22231,#22232,
#22233,#22234,#22235,#22236,#22237,#22238,#22239,#22240,#22241,#22242,#22243,
#22244,#22245,#22246,#22247,#22248,#22249,#22250,#22251,#22252,#22253,#22254,
#22255,#22256,#22257,#22258,#22259,#22260,#22261,#22262,#22263,#22264,#22265,
#22266,#22267,#22268,#22269,#22270,#22271,#22272,#22273,#22274,#22275,#22276,
#22277,#22278,#22279,#22280,#22281,#22282,#22283,#22284,#22285,#22286,#22287,
#22288,#22289,#22290,#22291,#22292,#22293,#22294,#22295,#22296,#22297,#22298,
#22299,#22300,#22301,#22302,#22303,#22304,#22305,#22306,#22307,#22308,#22309,
#22310,#22311,#22312,#22313,#22314),(#22315,#22316,#22317,#22318,#22319,
#22320,#22321,#22322,#22323,#22324,#22325,#22326,#22327,#22328,#22329,#22330,
#22331,#22332,#22333,#22334,#22335,#22336,#22337,#22338,#22339,#22340,#22341,
#22342,#22343,#22344,#22345,#22346,#22347,#22348,#22349,#22350,#22351,#22352,
#22353,#22354,#22355,#22356,#22357,#22358,#22359,#22360,#22361,#22362,#22363,
#22364,#22365,#22366,#22367,#22368,#22369,#22370,#22371,#22372,#22373,#22374,
#22375,#22376,#22377,#22378,#22379,#22380,#22381,#22382,#22383,#22384,#22385,
#22386,#22387,#22388,#22389,#22390,#22391,#22392,#22393,#22394,#22395,#22396,
#22397,#22398,#22399,#22400,#22401,#22402,#22403,#22404,#22405,#22406,#22407,
#22408,#22409,#22410,#22411,#22412,#22413,#22414,#22415,#22416,#22417,#22418,
#22419,#22420,#22421,#22422,#22423,#22424,#22425,#22426,#22427,#22428,#22429,
#22430,#22431,#22432,#22433,#22434,#22435,#22436,#22437,#22438,#22439,#22440,
#22441,#22442,#22443,#22444,#22445),(#22446,#22447,#22448,#22449,#22450,
#22451,#22452,#22453,#22454,#22455,#22456,#22457,#22458,#22459,#22460,#22461,
#22462,#22463,#22464,#22465,#22466,#22467,#22468,#22469,#22470,#22471,#22472,
#22473,#22474,#22475,#22476,#22477,#22478,#22479,#22480,#22481,#22482,#22483,
#22484,#22485,#22486,#22487,#22488,#22489,#22490,#22491,#22492,#22493,#22494,
#22495,#22496,#22497,#22498,#22499,#22500,#22501,#22502,#22503,#22504,#22505,
#22506,#22507,#22508,#22509,#22510,#22511,#22512,#22513,#22514,#22515,#22516,
#22517,#22518,#22519,#22520,#22521,#22522,#22523,#22524,#22525,#22526,#22527,
#22528,#22529,#22530,#22531,#22532,#22533,#22534,#22535,#22536,#22537,#22538,
#22539,#22540,#22541,#22542,#22543,#22544,#22545,#22546,#22547,#22548,#22549,
#22550,#22551,#22552,#22553,#22554,#22555,#22556,#22557,#22558,#22559,#22560,
#22561,#22562,#22563,#22564,#22565,#22566,#22567,#22568,#22569,#22570,#22571,
#22572,#22573,#22574,#22575,#22576),(#22577,#22578,#22579,#22580,#22581,
#22582,#22583,#22584,#22585,#22586,#22587,#22588,#22589,#22590,#22591,#22592,
#22593,#22594,#22595,#22596,#22597,#22598,#22599,#22600,#22601,#22602,#22603,
#22604,#22605,#22606,#22607,#22608,#22609,#22610,#22611,#22612,#22613,#22614,
#22615,#22616,#22617,#22618,#22619,#22620,#22621,#22622,#22623,#22624,#22625,
#22626,#22627,#22628,#22629,#22630,#22631,#22632,#22633,#22634,#22635,#22636,
#22637,#22638,#22639,#22640,#22641,#22642,#22643,#22644,#22645,#22646,#22647,
#22648,#22649,#22650,#22651,#22652,#22653,#22654,#22655,#22656,#22657,#22658,
#22659,#22660,#22661,#22662,#22663,#22664,#22665,#22666,#22667,#22668,#22669,
#22670,#22671,#22672,#22673,#22674,#22675,#22676,#22677,#22678,#22679,#22680,
#22681,#22682,#22683,#22684,#22685,#22686,#22687,#22688,#22689,#22690,#22691,
#22692,#22693,#22694,#22695,#22696,#22697,#22698,#22699,#22700,#22701,#22702,
#22703,#22704,#22705,#22706,#22707)),.UNSPECIFIED.,.F.,.F.,.F.,(4,4),(4,
1,1,1,1,1,1,1,1,1,1,1,1,1,1,1,1,1,1,1,1,1,1,1,1,1,1,1,1,1,1,1,1,1,1,1,1,
1,1,1,1,1,1,1,1,1,1,1,1,1,1,1,1,1,1,1,1,1,1,1,1,1,1,1,1,1,1,1,1,1,1,1,1,
1,1,1,1,1,1,1,1,1,1,1,1,1,1,1,1,1,1,1,1,1,1,1,1,1,1,1,1,1,1,1,1,1,1,1,1,
1,1,1,1,1,1,1,1,1,1,1,1,1,1,1,1,1,1,1,4),(-0.000646252380093648,0.082354798859151),
(8.31473274985794,9.31258359158534,10.3104344333127,11.3082852750401,12.3061361167675,
13.3039869584949,14.3018378002224,15.2996886419498,16.2975394836772,17.2953903254046,
18.293241167132,19.2910920088594,20.2889428505868,21.2867936923142,22.2846445340416,
23.282495375769,24.2803462174964,25.2781970592238,26.2760479009512,27.2738987426786,
28.271749584406,29.2696004261334,30.2674512678608,31.2653021095882,32.2631529513156,
33.261003793043,34.2588546347704,35.2567054764978,36.2545563182252,37.2524071599526,
38.25025800168,39.2481088434074,40.2459596851348,41.2438105268622,42.2416613685896,
43.239512210317,44.2373630520444,45.2352138937718,46.2330647354992,47.2309155772266,
48.228766418954,49.2266172606814,50.2244681024088,51.2223189441362,52.2201697858636,
53.218020627591,54.2158714693185,55.2137223110459,56.2115731527733,57.2094239945007,
58.2072748362281,59.2051256779555,60.2029765196829,61.2008273614103,62.1986782031377,
63.1965290448651,64.1943798865925,65.1922307283199,66.1900815700473,67.1879324117747,
68.1857832535021,69.1836340952295,70.1814849369569,71.1793357786843,72.1771866204117,
73.1750374621391,74.1728883038665,75.1707391455939,76.1685899873213,77.1664408290487,
78.1642916707761,79.1621425125035,80.1599933542309,81.1578441959583,82.1556950376857,
83.1535458794131,84.1513967211405,85.1492475628679,86.1470984045953,87.1449492463227,
88.1428000880501,89.1406509297776,90.1385017715049,91.1363526132323,92.1342034549598,
93.1320542966872,94.1299051384146,95.127755980142,96.1256068218694,97.1234576635968,
98.1213085053242,99.1191593470516,100.117010188779,101.114861030506,102.112711872234,
103.110562713961,104.108413555689,105.106264397416,106.104115239143,107.101966080871,
108.099816922598,109.097667764326,110.095518606053,111.09336944778,112.091220289508,
113.089071131235,114.086921972963,115.08477281469,116.082623656417,117.080474498145,
118.078325339872,119.0761761816,120.074027023327,121.071877865054,122.069728706782,
123.067579548509,124.065430390237,125.063281231964,126.061132073691,127.058982915419,
128.056833757146,129.054684598874,130.052535440601,131.050386282328,132.048237124056,
133.046087965783,134.043938807511,135.041789649238,136.040286743345),
 .UNSPECIFIED.);
#54=B_SPLINE_SURFACE_WITH_KNOTS('',3,3,((#22708,#22709,#22710,#22711,#22712,
#22713,#22714,#22715,#22716,#22717,#22718,#22719,#22720,#22721,#22722,#22723,
#22724,#22725,#22726,#22727,#22728,#22729,#22730,#22731,#22732,#22733,#22734,
#22735,#22736,#22737,#22738,#22739,#22740,#22741,#22742,#22743,#22744,#22745,
#22746,#22747,#22748,#22749,#22750,#22751,#22752,#22753,#22754,#22755,#22756,
#22757,#22758,#22759,#22760,#22761,#22762,#22763,#22764,#22765,#22766,#22767,
#22768,#22769,#22770,#22771,#22772,#22773,#22774,#22775,#22776,#22777,#22778,
#22779,#22780,#22781,#22782,#22783,#22784,#22785,#22786,#22787,#22788,#22789,
#22790,#22791,#22792,#22793,#22794,#22795,#22796,#22797,#22798,#22799,#22800,
#22801,#22802,#22803,#22804,#22805,#22806,#22807,#22808,#22809,#22810,#22811,
#22812,#22813,#22814,#22815,#22816,#22817,#22818,#22819,#22820,#22821,#22822,
#22823,#22824,#22825,#22826,#22827,#22828,#22829,#22830,#22831,#22832,#22833,
#22834,#22835,#22836,#22837,#22838),(#22839,#22840,#22841,#22842,#22843,
#22844,#22845,#22846,#22847,#22848,#22849,#22850,#22851,#22852,#22853,#22854,
#22855,#22856,#22857,#22858,#22859,#22860,#22861,#22862,#22863,#22864,#22865,
#22866,#22867,#22868,#22869,#22870,#22871,#22872,#22873,#22874,#22875,#22876,
#22877,#22878,#22879,#22880,#22881,#22882,#22883,#22884,#22885,#22886,#22887,
#22888,#22889,#22890,#22891,#22892,#22893,#22894,#22895,#22896,#22897,#22898,
#22899,#22900,#22901,#22902,#22903,#22904,#22905,#22906,#22907,#22908,#22909,
#22910,#22911,#22912,#22913,#22914,#22915,#22916,#22917,#22918,#22919,#22920,
#22921,#22922,#22923,#22924,#22925,#22926,#22927,#22928,#22929,#22930,#22931,
#22932,#22933,#22934,#22935,#22936,#22937,#22938,#22939,#22940,#22941,#22942,
#22943,#22944,#22945,#22946,#22947,#22948,#22949,#22950,#22951,#22952,#22953,
#22954,#22955,#22956,#22957,#22958,#22959,#22960,#22961,#22962,#22963,#22964,
#22965,#22966,#22967,#22968,#22969),(#22970,#22971,#22972,#22973,#22974,
#22975,#22976,#22977,#22978,#22979,#22980,#22981,#22982,#22983,#22984,#22985,
#22986,#22987,#22988,#22989,#22990,#22991,#22992,#22993,#22994,#22995,#22996,
#22997,#22998,#22999,#23000,#23001,#23002,#23003,#23004,#23005,#23006,#23007,
#23008,#23009,#23010,#23011,#23012,#23013,#23014,#23015,#23016,#23017,#23018,
#23019,#23020,#23021,#23022,#23023,#23024,#23025,#23026,#23027,#23028,#23029,
#23030,#23031,#23032,#23033,#23034,#23035,#23036,#23037,#23038,#23039,#23040,
#23041,#23042,#23043,#23044,#23045,#23046,#23047,#23048,#23049,#23050,#23051,
#23052,#23053,#23054,#23055,#23056,#23057,#23058,#23059,#23060,#23061,#23062,
#23063,#23064,#23065,#23066,#23067,#23068,#23069,#23070,#23071,#23072,#23073,
#23074,#23075,#23076,#23077,#23078,#23079,#23080,#23081,#23082,#23083,#23084,
#23085,#23086,#23087,#23088,#23089,#23090,#23091,#23092,#23093,#23094,#23095,
#23096,#23097,#23098,#23099,#23100),(#23101,#23102,#23103,#23104,#23105,
#23106,#23107,#23108,#23109,#23110,#23111,#23112,#23113,#23114,#23115,#23116,
#23117,#23118,#23119,#23120,#23121,#23122,#23123,#23124,#23125,#23126,#23127,
#23128,#23129,#23130,#23131,#23132,#23133,#23134,#23135,#23136,#23137,#23138,
#23139,#23140,#23141,#23142,#23143,#23144,#23145,#23146,#23147,#23148,#23149,
#23150,#23151,#23152,#23153,#23154,#23155,#23156,#23157,#23158,#23159,#23160,
#23161,#23162,#23163,#23164,#23165,#23166,#23167,#23168,#23169,#23170,#23171,
#23172,#23173,#23174,#23175,#23176,#23177,#23178,#23179,#23180,#23181,#23182,
#23183,#23184,#23185,#23186,#23187,#23188,#23189,#23190,#23191,#23192,#23193,
#23194,#23195,#23196,#23197,#23198,#23199,#23200,#23201,#23202,#23203,#23204,
#23205,#23206,#23207,#23208,#23209,#23210,#23211,#23212,#23213,#23214,#23215,
#23216,#23217,#23218,#23219,#23220,#23221,#23222,#23223,#23224,#23225,#23226,
#23227,#23228,#23229,#23230,#23231)),.UNSPECIFIED.,.F.,.F.,.F.,(4,4),(4,
1,1,1,1,1,1,1,1,1,1,1,1,1,1,1,1,1,1,1,1,1,1,1,1,1,1,1,1,1,1,1,1,1,1,1,1,
1,1,1,1,1,1,1,1,1,1,1,1,1,1,1,1,1,1,1,1,1,1,1,1,1,1,1,1,1,1,1,1,1,1,1,1,
1,1,1,1,1,1,1,1,1,1,1,1,1,1,1,1,1,1,1,1,1,1,1,1,1,1,1,1,1,1,1,1,1,1,1,1,
1,1,1,1,1,1,1,1,1,1,1,1,1,1,1,1,1,1,1,4),(-0.000646252380093648,0.082354798859151),
(8.31473274985794,9.31258359158534,10.3104344333127,11.3082852750401,12.3061361167675,
13.3039869584949,14.3018378002224,15.2996886419498,16.2975394836772,17.2953903254046,
18.293241167132,19.2910920088594,20.2889428505868,21.2867936923142,22.2846445340416,
23.282495375769,24.2803462174964,25.2781970592238,26.2760479009512,27.2738987426786,
28.271749584406,29.2696004261334,30.2674512678608,31.2653021095882,32.2631529513156,
33.261003793043,34.2588546347704,35.2567054764978,36.2545563182252,37.2524071599526,
38.25025800168,39.2481088434074,40.2459596851348,41.2438105268622,42.2416613685896,
43.239512210317,44.2373630520444,45.2352138937718,46.2330647354992,47.2309155772266,
48.228766418954,49.2266172606814,50.2244681024088,51.2223189441362,52.2201697858636,
53.218020627591,54.2158714693185,55.2137223110459,56.2115731527733,57.2094239945007,
58.2072748362281,59.2051256779555,60.2029765196829,61.2008273614103,62.1986782031377,
63.1965290448651,64.1943798865925,65.1922307283199,66.1900815700473,67.1879324117747,
68.1857832535021,69.1836340952295,70.1814849369569,71.1793357786843,72.1771866204117,
73.1750374621391,74.1728883038665,75.1707391455939,76.1685899873213,77.1664408290487,
78.1642916707761,79.1621425125035,80.1599933542309,81.1578441959583,82.1556950376857,
83.1535458794131,84.1513967211405,85.1492475628679,86.1470984045953,87.1449492463227,
88.1428000880501,89.1406509297776,90.1385017715049,91.1363526132323,92.1342034549598,
93.1320542966872,94.1299051384146,95.127755980142,96.1256068218694,97.1234576635968,
98.1213085053242,99.1191593470516,100.117010188779,101.114861030506,102.112711872234,
103.110562713961,104.108413555689,105.106264397416,106.104115239143,107.101966080871,
108.099816922598,109.097667764326,110.095518606053,111.09336944778,112.091220289508,
113.089071131235,114.086921972963,115.08477281469,116.082623656417,117.080474498145,
118.078325339872,119.0761761816,120.074027023327,121.071877865054,122.069728706782,
123.067579548509,124.065430390237,125.063281231964,126.061132073691,127.058982915419,
128.056833757146,129.054684598874,130.052535440601,131.050386282328,132.048237124056,
133.046087965783,134.043938807511,135.041789649238,136.040286743345),
 .UNSPECIFIED.);
#55=B_SPLINE_SURFACE_WITH_KNOTS('',3,3,((#23232,#23233,#23234,#23235,#23236,
#23237,#23238,#23239,#23240,#23241,#23242,#23243,#23244,#23245,#23246,#23247,
#23248,#23249,#23250,#23251,#23252,#23253,#23254,#23255,#23256,#23257,#23258,
#23259,#23260,#23261,#23262,#23263,#23264,#23265,#23266,#23267,#23268,#23269,
#23270,#23271,#23272,#23273,#23274,#23275,#23276,#23277,#23278,#23279,#23280,
#23281,#23282,#23283,#23284,#23285,#23286,#23287,#23288,#23289,#23290,#23291,
#23292,#23293,#23294,#23295,#23296,#23297,#23298,#23299,#23300,#23301,#23302,
#23303,#23304,#23305,#23306,#23307,#23308,#23309,#23310,#23311,#23312,#23313,
#23314,#23315,#23316,#23317,#23318,#23319,#23320,#23321,#23322,#23323,#23324,
#23325,#23326,#23327,#23328,#23329,#23330,#23331,#23332,#23333,#23334,#23335,
#23336,#23337,#23338,#23339,#23340,#23341,#23342,#23343,#23344,#23345,#23346,
#23347,#23348,#23349,#23350,#23351,#23352,#23353,#23354,#23355,#23356,#23357,
#23358,#23359,#23360,#23361,#23362),(#23363,#23364,#23365,#23366,#23367,
#23368,#23369,#23370,#23371,#23372,#23373,#23374,#23375,#23376,#23377,#23378,
#23379,#23380,#23381,#23382,#23383,#23384,#23385,#23386,#23387,#23388,#23389,
#23390,#23391,#23392,#23393,#23394,#23395,#23396,#23397,#23398,#23399,#23400,
#23401,#23402,#23403,#23404,#23405,#23406,#23407,#23408,#23409,#23410,#23411,
#23412,#23413,#23414,#23415,#23416,#23417,#23418,#23419,#23420,#23421,#23422,
#23423,#23424,#23425,#23426,#23427,#23428,#23429,#23430,#23431,#23432,#23433,
#23434,#23435,#23436,#23437,#23438,#23439,#23440,#23441,#23442,#23443,#23444,
#23445,#23446,#23447,#23448,#23449,#23450,#23451,#23452,#23453,#23454,#23455,
#23456,#23457,#23458,#23459,#23460,#23461,#23462,#23463,#23464,#23465,#23466,
#23467,#23468,#23469,#23470,#23471,#23472,#23473,#23474,#23475,#23476,#23477,
#23478,#23479,#23480,#23481,#23482,#23483,#23484,#23485,#23486,#23487,#23488,
#23489,#23490,#23491,#23492,#23493),(#23494,#23495,#23496,#23497,#23498,
#23499,#23500,#23501,#23502,#23503,#23504,#23505,#23506,#23507,#23508,#23509,
#23510,#23511,#23512,#23513,#23514,#23515,#23516,#23517,#23518,#23519,#23520,
#23521,#23522,#23523,#23524,#23525,#23526,#23527,#23528,#23529,#23530,#23531,
#23532,#23533,#23534,#23535,#23536,#23537,#23538,#23539,#23540,#23541,#23542,
#23543,#23544,#23545,#23546,#23547,#23548,#23549,#23550,#23551,#23552,#23553,
#23554,#23555,#23556,#23557,#23558,#23559,#23560,#23561,#23562,#23563,#23564,
#23565,#23566,#23567,#23568,#23569,#23570,#23571,#23572,#23573,#23574,#23575,
#23576,#23577,#23578,#23579,#23580,#23581,#23582,#23583,#23584,#23585,#23586,
#23587,#23588,#23589,#23590,#23591,#23592,#23593,#23594,#23595,#23596,#23597,
#23598,#23599,#23600,#23601,#23602,#23603,#23604,#23605,#23606,#23607,#23608,
#23609,#23610,#23611,#23612,#23613,#23614,#23615,#23616,#23617,#23618,#23619,
#23620,#23621,#23622,#23623,#23624),(#23625,#23626,#23627,#23628,#23629,
#23630,#23631,#23632,#23633,#23634,#23635,#23636,#23637,#23638,#23639,#23640,
#23641,#23642,#23643,#23644,#23645,#23646,#23647,#23648,#23649,#23650,#23651,
#23652,#23653,#23654,#23655,#23656,#23657,#23658,#23659,#23660,#23661,#23662,
#23663,#23664,#23665,#23666,#23667,#23668,#23669,#23670,#23671,#23672,#23673,
#23674,#23675,#23676,#23677,#23678,#23679,#23680,#23681,#23682,#23683,#23684,
#23685,#23686,#23687,#23688,#23689,#23690,#23691,#23692,#23693,#23694,#23695,
#23696,#23697,#23698,#23699,#23700,#23701,#23702,#23703,#23704,#23705,#23706,
#23707,#23708,#23709,#23710,#23711,#23712,#23713,#23714,#23715,#23716,#23717,
#23718,#23719,#23720,#23721,#23722,#23723,#23724,#23725,#23726,#23727,#23728,
#23729,#23730,#23731,#23732,#23733,#23734,#23735,#23736,#23737,#23738,#23739,
#23740,#23741,#23742,#23743,#23744,#23745,#23746,#23747,#23748,#23749,#23750,
#23751,#23752,#23753,#23754,#23755)),.UNSPECIFIED.,.F.,.F.,.F.,(4,4),(4,
1,1,1,1,1,1,1,1,1,1,1,1,1,1,1,1,1,1,1,1,1,1,1,1,1,1,1,1,1,1,1,1,1,1,1,1,
1,1,1,1,1,1,1,1,1,1,1,1,1,1,1,1,1,1,1,1,1,1,1,1,1,1,1,1,1,1,1,1,1,1,1,1,
1,1,1,1,1,1,1,1,1,1,1,1,1,1,1,1,1,1,1,1,1,1,1,1,1,1,1,1,1,1,1,1,1,1,1,1,
1,1,1,1,1,1,1,1,1,1,1,1,1,1,1,1,1,1,1,4),(-0.000646252380093648,0.082354798859151),
(8.31473274985794,9.31258359158534,10.3104344333127,11.3082852750401,12.3061361167675,
13.3039869584949,14.3018378002224,15.2996886419498,16.2975394836772,17.2953903254046,
18.293241167132,19.2910920088594,20.2889428505868,21.2867936923142,22.2846445340416,
23.282495375769,24.2803462174964,25.2781970592238,26.2760479009512,27.2738987426786,
28.271749584406,29.2696004261334,30.2674512678608,31.2653021095882,32.2631529513156,
33.261003793043,34.2588546347704,35.2567054764978,36.2545563182252,37.2524071599526,
38.25025800168,39.2481088434074,40.2459596851348,41.2438105268622,42.2416613685896,
43.239512210317,44.2373630520444,45.2352138937718,46.2330647354992,47.2309155772266,
48.228766418954,49.2266172606814,50.2244681024088,51.2223189441362,52.2201697858636,
53.218020627591,54.2158714693185,55.2137223110459,56.2115731527733,57.2094239945007,
58.2072748362281,59.2051256779555,60.2029765196829,61.2008273614103,62.1986782031377,
63.1965290448651,64.1943798865925,65.1922307283199,66.1900815700473,67.1879324117747,
68.1857832535021,69.1836340952295,70.1814849369569,71.1793357786843,72.1771866204117,
73.1750374621391,74.1728883038665,75.1707391455939,76.1685899873213,77.1664408290487,
78.1642916707761,79.1621425125035,80.1599933542309,81.1578441959583,82.1556950376857,
83.1535458794131,84.1513967211405,85.1492475628679,86.1470984045953,87.1449492463227,
88.1428000880501,89.1406509297776,90.1385017715049,91.1363526132323,92.1342034549598,
93.1320542966872,94.1299051384146,95.127755980142,96.1256068218694,97.1234576635968,
98.1213085053242,99.1191593470516,100.117010188779,101.114861030506,102.112711872234,
103.110562713961,104.108413555689,105.106264397416,106.104115239143,107.101966080871,
108.099816922598,109.097667764326,110.095518606053,111.09336944778,112.091220289508,
113.089071131235,114.086921972963,115.08477281469,116.082623656417,117.080474498145,
118.078325339872,119.0761761816,120.074027023327,121.071877865054,122.069728706782,
123.067579548509,124.065430390237,125.063281231964,126.061132073691,127.058982915419,
128.056833757146,129.054684598874,130.052535440601,131.050386282328,132.048237124056,
133.046087965783,134.043938807511,135.041789649238,136.040286743345),
 .UNSPECIFIED.);
#56=B_SPLINE_SURFACE_WITH_KNOTS('',3,3,((#24051,#24052,#24053,#24054,#24055,
#24056,#24057,#24058,#24059,#24060,#24061,#24062,#24063,#24064,#24065,#24066,
#24067,#24068,#24069,#24070,#24071,#24072,#24073,#24074,#24075,#24076,#24077,
#24078,#24079,#24080,#24081,#24082,#24083,#24084,#24085,#24086,#24087,#24088,
#24089,#24090,#24091,#24092,#24093,#24094,#24095,#24096,#24097,#24098,#24099,
#24100,#24101,#24102,#24103,#24104,#24105,#24106,#24107,#24108,#24109,#24110,
#24111,#24112,#24113,#24114,#24115,#24116,#24117,#24118,#24119,#24120,#24121,
#24122,#24123,#24124,#24125,#24126,#24127,#24128,#24129,#24130,#24131,#24132,
#24133,#24134,#24135,#24136,#24137,#24138,#24139,#24140,#24141,#24142,#24143,
#24144,#24145,#24146,#24147,#24148,#24149,#24150,#24151,#24152,#24153,#24154,
#24155,#24156,#24157,#24158,#24159,#24160,#24161,#24162,#24163,#24164,#24165,
#24166,#24167,#24168,#24169,#24170,#24171,#24172,#24173,#24174,#24175,#24176,
#24177,#24178,#24179,#24180,#24181),(#24182,#24183,#24184,#24185,#24186,
#24187,#24188,#24189,#24190,#24191,#24192,#24193,#24194,#24195,#24196,#24197,
#24198,#24199,#24200,#24201,#24202,#24203,#24204,#24205,#24206,#24207,#24208,
#24209,#24210,#24211,#24212,#24213,#24214,#24215,#24216,#24217,#24218,#24219,
#24220,#24221,#24222,#24223,#24224,#24225,#24226,#24227,#24228,#24229,#24230,
#24231,#24232,#24233,#24234,#24235,#24236,#24237,#24238,#24239,#24240,#24241,
#24242,#24243,#24244,#24245,#24246,#24247,#24248,#24249,#24250,#24251,#24252,
#24253,#24254,#24255,#24256,#24257,#24258,#24259,#24260,#24261,#24262,#24263,
#24264,#24265,#24266,#24267,#24268,#24269,#24270,#24271,#24272,#24273,#24274,
#24275,#24276,#24277,#24278,#24279,#24280,#24281,#24282,#24283,#24284,#24285,
#24286,#24287,#24288,#24289,#24290,#24291,#24292,#24293,#24294,#24295,#24296,
#24297,#24298,#24299,#24300,#24301,#24302,#24303,#24304,#24305,#24306,#24307,
#24308,#24309,#24310,#24311,#24312),(#24313,#24314,#24315,#24316,#24317,
#24318,#24319,#24320,#24321,#24322,#24323,#24324,#24325,#24326,#24327,#24328,
#24329,#24330,#24331,#24332,#24333,#24334,#24335,#24336,#24337,#24338,#24339,
#24340,#24341,#24342,#24343,#24344,#24345,#24346,#24347,#24348,#24349,#24350,
#24351,#24352,#24353,#24354,#24355,#24356,#24357,#24358,#24359,#24360,#24361,
#24362,#24363,#24364,#24365,#24366,#24367,#24368,#24369,#24370,#24371,#24372,
#24373,#24374,#24375,#24376,#24377,#24378,#24379,#24380,#24381,#24382,#24383,
#24384,#24385,#24386,#24387,#24388,#24389,#24390,#24391,#24392,#24393,#24394,
#24395,#24396,#24397,#24398,#24399,#24400,#24401,#24402,#24403,#24404,#24405,
#24406,#24407,#24408,#24409,#24410,#24411,#24412,#24413,#24414,#24415,#24416,
#24417,#24418,#24419,#24420,#24421,#24422,#24423,#24424,#24425,#24426,#24427,
#24428,#24429,#24430,#24431,#24432,#24433,#24434,#24435,#24436,#24437,#24438,
#24439,#24440,#24441,#24442,#24443),(#24444,#24445,#24446,#24447,#24448,
#24449,#24450,#24451,#24452,#24453,#24454,#24455,#24456,#24457,#24458,#24459,
#24460,#24461,#24462,#24463,#24464,#24465,#24466,#24467,#24468,#24469,#24470,
#24471,#24472,#24473,#24474,#24475,#24476,#24477,#24478,#24479,#24480,#24481,
#24482,#24483,#24484,#24485,#24486,#24487,#24488,#24489,#24490,#24491,#24492,
#24493,#24494,#24495,#24496,#24497,#24498,#24499,#24500,#24501,#24502,#24503,
#24504,#24505,#24506,#24507,#24508,#24509,#24510,#24511,#24512,#24513,#24514,
#24515,#24516,#24517,#24518,#24519,#24520,#24521,#24522,#24523,#24524,#24525,
#24526,#24527,#24528,#24529,#24530,#24531,#24532,#24533,#24534,#24535,#24536,
#24537,#24538,#24539,#24540,#24541,#24542,#24543,#24544,#24545,#24546,#24547,
#24548,#24549,#24550,#24551,#24552,#24553,#24554,#24555,#24556,#24557,#24558,
#24559,#24560,#24561,#24562,#24563,#24564,#24565,#24566,#24567,#24568,#24569,
#24570,#24571,#24572,#24573,#24574)),.UNSPECIFIED.,.F.,.F.,.F.,(4,4),(4,
1,1,1,1,1,1,1,1,1,1,1,1,1,1,1,1,1,1,1,1,1,1,1,1,1,1,1,1,1,1,1,1,1,1,1,1,
1,1,1,1,1,1,1,1,1,1,1,1,1,1,1,1,1,1,1,1,1,1,1,1,1,1,1,1,1,1,1,1,1,1,1,1,
1,1,1,1,1,1,1,1,1,1,1,1,1,1,1,1,1,1,1,1,1,1,1,1,1,1,1,1,1,1,1,1,1,1,1,1,
1,1,1,1,1,1,1,1,1,1,1,1,1,1,1,1,1,1,1,4),(-0.000646252380093648,0.082354798859151),
(8.31473274985794,9.31258359158534,10.3104344333127,11.3082852750401,12.3061361167675,
13.3039869584949,14.3018378002224,15.2996886419498,16.2975394836772,17.2953903254046,
18.293241167132,19.2910920088594,20.2889428505868,21.2867936923142,22.2846445340416,
23.282495375769,24.2803462174964,25.2781970592238,26.2760479009512,27.2738987426786,
28.271749584406,29.2696004261334,30.2674512678608,31.2653021095882,32.2631529513156,
33.261003793043,34.2588546347704,35.2567054764978,36.2545563182252,37.2524071599526,
38.25025800168,39.2481088434074,40.2459596851348,41.2438105268622,42.2416613685896,
43.239512210317,44.2373630520444,45.2352138937718,46.2330647354992,47.2309155772266,
48.228766418954,49.2266172606814,50.2244681024088,51.2223189441362,52.2201697858636,
53.218020627591,54.2158714693185,55.2137223110459,56.2115731527733,57.2094239945007,
58.2072748362281,59.2051256779555,60.2029765196829,61.2008273614103,62.1986782031377,
63.1965290448651,64.1943798865925,65.1922307283199,66.1900815700473,67.1879324117747,
68.1857832535021,69.1836340952295,70.1814849369569,71.1793357786843,72.1771866204117,
73.1750374621391,74.1728883038665,75.1707391455939,76.1685899873213,77.1664408290487,
78.1642916707761,79.1621425125035,80.1599933542309,81.1578441959583,82.1556950376857,
83.1535458794131,84.1513967211405,85.1492475628679,86.1470984045953,87.1449492463227,
88.1428000880501,89.1406509297776,90.1385017715049,91.1363526132323,92.1342034549598,
93.1320542966872,94.1299051384146,95.127755980142,96.1256068218694,97.1234576635968,
98.1213085053242,99.1191593470516,100.117010188779,101.114861030506,102.112711872234,
103.110562713961,104.108413555689,105.106264397416,106.104115239143,107.101966080871,
108.099816922598,109.097667764326,110.095518606053,111.09336944778,112.091220289508,
113.089071131235,114.086921972963,115.08477281469,116.082623656417,117.080474498145,
118.078325339872,119.0761761816,120.074027023327,121.071877865054,122.069728706782,
123.067579548509,124.065430390237,125.063281231964,126.061132073691,127.058982915419,
128.056833757146,129.054684598874,130.052535440601,131.050386282328,132.048237124056,
133.046087965783,134.043938807511,135.041789649238,136.040286743345),
 .UNSPECIFIED.);
#57=B_SPLINE_SURFACE_WITH_KNOTS('',3,3,((#24575,#24576,#24577,#24578,#24579,
#24580,#24581,#24582,#24583,#24584,#24585,#24586,#24587,#24588,#24589,#24590,
#24591,#24592,#24593,#24594,#24595,#24596,#24597,#24598,#24599,#24600,#24601,
#24602,#24603,#24604,#24605,#24606,#24607,#24608,#24609,#24610,#24611,#24612,
#24613,#24614,#24615,#24616,#24617,#24618,#24619,#24620,#24621,#24622,#24623,
#24624,#24625,#24626,#24627,#24628,#24629,#24630,#24631,#24632,#24633,#24634,
#24635,#24636,#24637,#24638,#24639,#24640,#24641,#24642,#24643,#24644,#24645,
#24646,#24647,#24648,#24649,#24650,#24651,#24652,#24653,#24654,#24655,#24656,
#24657,#24658,#24659,#24660,#24661,#24662,#24663,#24664,#24665,#24666,#24667,
#24668,#24669,#24670,#24671,#24672,#24673,#24674,#24675,#24676,#24677,#24678,
#24679,#24680,#24681,#24682,#24683,#24684,#24685,#24686,#24687,#24688,#24689,
#24690,#24691,#24692,#24693,#24694,#24695,#24696,#24697,#24698,#24699,#24700,
#24701,#24702,#24703,#24704,#24705),(#24706,#24707,#24708,#24709,#24710,
#24711,#24712,#24713,#24714,#24715,#24716,#24717,#24718,#24719,#24720,#24721,
#24722,#24723,#24724,#24725,#24726,#24727,#24728,#24729,#24730,#24731,#24732,
#24733,#24734,#24735,#24736,#24737,#24738,#24739,#24740,#24741,#24742,#24743,
#24744,#24745,#24746,#24747,#24748,#24749,#24750,#24751,#24752,#24753,#24754,
#24755,#24756,#24757,#24758,#24759,#24760,#24761,#24762,#24763,#24764,#24765,
#24766,#24767,#24768,#24769,#24770,#24771,#24772,#24773,#24774,#24775,#24776,
#24777,#24778,#24779,#24780,#24781,#24782,#24783,#24784,#24785,#24786,#24787,
#24788,#24789,#24790,#24791,#24792,#24793,#24794,#24795,#24796,#24797,#24798,
#24799,#24800,#24801,#24802,#24803,#24804,#24805,#24806,#24807,#24808,#24809,
#24810,#24811,#24812,#24813,#24814,#24815,#24816,#24817,#24818,#24819,#24820,
#24821,#24822,#24823,#24824,#24825,#24826,#24827,#24828,#24829,#24830,#24831,
#24832,#24833,#24834,#24835,#24836),(#24837,#24838,#24839,#24840,#24841,
#24842,#24843,#24844,#24845,#24846,#24847,#24848,#24849,#24850,#24851,#24852,
#24853,#24854,#24855,#24856,#24857,#24858,#24859,#24860,#24861,#24862,#24863,
#24864,#24865,#24866,#24867,#24868,#24869,#24870,#24871,#24872,#24873,#24874,
#24875,#24876,#24877,#24878,#24879,#24880,#24881,#24882,#24883,#24884,#24885,
#24886,#24887,#24888,#24889,#24890,#24891,#24892,#24893,#24894,#24895,#24896,
#24897,#24898,#24899,#24900,#24901,#24902,#24903,#24904,#24905,#24906,#24907,
#24908,#24909,#24910,#24911,#24912,#24913,#24914,#24915,#24916,#24917,#24918,
#24919,#24920,#24921,#24922,#24923,#24924,#24925,#24926,#24927,#24928,#24929,
#24930,#24931,#24932,#24933,#24934,#24935,#24936,#24937,#24938,#24939,#24940,
#24941,#24942,#24943,#24944,#24945,#24946,#24947,#24948,#24949,#24950,#24951,
#24952,#24953,#24954,#24955,#24956,#24957,#24958,#24959,#24960,#24961,#24962,
#24963,#24964,#24965,#24966,#24967),(#24968,#24969,#24970,#24971,#24972,
#24973,#24974,#24975,#24976,#24977,#24978,#24979,#24980,#24981,#24982,#24983,
#24984,#24985,#24986,#24987,#24988,#24989,#24990,#24991,#24992,#24993,#24994,
#24995,#24996,#24997,#24998,#24999,#25000,#25001,#25002,#25003,#25004,#25005,
#25006,#25007,#25008,#25009,#25010,#25011,#25012,#25013,#25014,#25015,#25016,
#25017,#25018,#25019,#25020,#25021,#25022,#25023,#25024,#25025,#25026,#25027,
#25028,#25029,#25030,#25031,#25032,#25033,#25034,#25035,#25036,#25037,#25038,
#25039,#25040,#25041,#25042,#25043,#25044,#25045,#25046,#25047,#25048,#25049,
#25050,#25051,#25052,#25053,#25054,#25055,#25056,#25057,#25058,#25059,#25060,
#25061,#25062,#25063,#25064,#25065,#25066,#25067,#25068,#25069,#25070,#25071,
#25072,#25073,#25074,#25075,#25076,#25077,#25078,#25079,#25080,#25081,#25082,
#25083,#25084,#25085,#25086,#25087,#25088,#25089,#25090,#25091,#25092,#25093,
#25094,#25095,#25096,#25097,#25098)),.UNSPECIFIED.,.F.,.F.,.F.,(4,4),(4,
1,1,1,1,1,1,1,1,1,1,1,1,1,1,1,1,1,1,1,1,1,1,1,1,1,1,1,1,1,1,1,1,1,1,1,1,
1,1,1,1,1,1,1,1,1,1,1,1,1,1,1,1,1,1,1,1,1,1,1,1,1,1,1,1,1,1,1,1,1,1,1,1,
1,1,1,1,1,1,1,1,1,1,1,1,1,1,1,1,1,1,1,1,1,1,1,1,1,1,1,1,1,1,1,1,1,1,1,1,
1,1,1,1,1,1,1,1,1,1,1,1,1,1,1,1,1,1,1,4),(-0.000314077148181808,0.0826777824702824),
(11.6145490510227,12.613065069482,13.6109159112094,14.6087667529368,15.6066175946642,
16.6044684363917,17.6023192781191,18.6001701198465,19.5980209615739,20.5958718033013,
21.5937226450287,22.5915734867561,23.5894243284835,24.5872751702109,25.5851260119383,
26.5829768536657,27.5808276953931,28.5786785371205,29.5765293788479,30.5743802205753,
31.5722310623027,32.5700819040301,33.5679327457575,34.5657835874849,35.5636344292123,
36.5614852709397,37.5593361126671,38.5571869543945,39.5550377961219,40.5528886378493,
41.5507394795767,42.5485903213041,43.5464411630315,44.5442920047589,45.5421428464863,
46.5399936882137,47.5378445299411,48.5356953716685,49.5335462133959,50.5313970551233,
51.5292478968507,52.5270987385781,53.5249495803055,54.522800422033,55.5206512637604,
56.5185021054878,57.5163529472152,58.5142037889426,59.51205463067,60.5099054723974,
61.5077563141248,62.5056071558522,63.5034579975796,64.501308839307,65.4991596810344,
66.4970105227618,67.4948613644892,68.4927122062166,69.490563047944,70.4884138896714,
71.4862647313988,72.4841155731262,73.4819664148536,74.479817256581,75.4776680983084,
76.4755189400358,77.4733697817632,78.4712206234906,79.469071465218,80.4669223069454,
81.4647731486728,82.4626239904002,83.4604748321276,84.458325673855,85.4561765155824,
86.4540273573098,87.4518781990372,88.4497290407646,89.4475798824921,90.4454307242194,
91.4432815659468,92.4411324076742,93.4389832494017,94.4368340911291,95.4346849328565,
96.4325357745839,97.4303866163113,98.4282374580387,99.4260882997661,100.423939141493,
101.421789983221,102.419640824948,103.417491666676,104.415342508403,105.41319335013,
106.411044191858,107.408895033585,108.406745875313,109.40459671704,110.402447558768,
111.400298400495,112.398149242222,113.39600008395,114.393850925677,115.391701767405,
116.389552609132,117.387403450859,118.385254292587,119.383105134314,120.380955976042,
121.378806817769,122.376657659496,123.374508501224,124.372359342951,125.370210184679,
126.368061026406,127.365911868133,128.363762709861,129.361613551588,130.359464393316,
131.357315235043,132.35516607677,133.353016918498,134.350867760225,135.348718601953,
136.34656944368,137.344420285407,138.342271127135,139.340121968862),
 .UNSPECIFIED.);
#58=B_SPLINE_SURFACE_WITH_KNOTS('',3,3,((#27435,#27436,#27437,#27438,#27439,
#27440,#27441,#27442,#27443,#27444,#27445,#27446,#27447,#27448,#27449,#27450,
#27451,#27452,#27453,#27454,#27455,#27456,#27457,#27458,#27459,#27460,#27461,
#27462,#27463,#27464,#27465),(#27466,#27467,#27468,#27469,#27470,#27471,
#27472,#27473,#27474,#27475,#27476,#27477,#27478,#27479,#27480,#27481,#27482,
#27483,#27484,#27485,#27486,#27487,#27488,#27489,#27490,#27491,#27492,#27493,
#27494,#27495,#27496),(#27497,#27498,#27499,#27500,#27501,#27502,#27503,
#27504,#27505,#27506,#27507,#27508,#27509,#27510,#27511,#27512,#27513,#27514,
#27515,#27516,#27517,#27518,#27519,#27520,#27521,#27522,#27523,#27524,#27525,
#27526,#27527),(#27528,#27529,#27530,#27531,#27532,#27533,#27534,#27535,
#27536,#27537,#27538,#27539,#27540,#27541,#27542,#27543,#27544,#27545,#27546,
#27547,#27548,#27549,#27550,#27551,#27552,#27553,#27554,#27555,#27556,#27557,
#27558)),.UNSPECIFIED.,.F.,.F.,.F.,(4,4),(4,1,1,1,1,1,1,1,1,1,1,1,1,1,1,
1,1,1,1,1,1,1,1,1,1,1,1,1,4),(-0.000628230388590609,0.0805634975574235),
(11.8569095924278,12.8271953814412,13.7968529400659,14.7665104986906,15.7361680573154,
16.7058256159401,17.6754831745648,18.6451407331896,19.6147982918143,20.584455850439,
21.5541134090638,22.5237709676885,23.4934285263132,24.4630860849379,25.4327436435627,
26.4024012021874,27.3720587608121,28.3417163194369,29.3113738780616,30.2810314366863,
31.2506889953111,32.2203465539358,33.1900041125605,34.1596616711853,35.12931922981,
36.0989767884347,37.0686343470595,38.0382919056842,39.0079494643089),
 .UNSPECIFIED.);
#59=B_SPLINE_SURFACE_WITH_KNOTS('',3,3,((#27743,#27744,#27745,#27746,#27747,
#27748,#27749,#27750,#27751,#27752,#27753,#27754,#27755,#27756,#27757,#27758,
#27759,#27760,#27761,#27762,#27763,#27764,#27765,#27766,#27767,#27768,#27769,
#27770,#27771,#27772,#27773),(#27774,#27775,#27776,#27777,#27778,#27779,
#27780,#27781,#27782,#27783,#27784,#27785,#27786,#27787,#27788,#27789,#27790,
#27791,#27792,#27793,#27794,#27795,#27796,#27797,#27798,#27799,#27800,#27801,
#27802,#27803,#27804),(#27805,#27806,#27807,#27808,#27809,#27810,#27811,
#27812,#27813,#27814,#27815,#27816,#27817,#27818,#27819,#27820,#27821,#27822,
#27823,#27824,#27825,#27826,#27827,#27828,#27829,#27830,#27831,#27832,#27833,
#27834,#27835),(#27836,#27837,#27838,#27839,#27840,#27841,#27842,#27843,
#27844,#27845,#27846,#27847,#27848,#27849,#27850,#27851,#27852,#27853,#27854,
#27855,#27856,#27857,#27858,#27859,#27860,#27861,#27862,#27863,#27864,#27865,
#27866)),.UNSPECIFIED.,.F.,.F.,.F.,(4,4),(4,1,1,1,1,1,1,1,1,1,1,1,1,1,1,
1,1,1,1,1,1,1,1,1,1,1,1,1,4),(-0.000286423065855878,0.0807675649255769),
(14.3991256467175,15.3687832053423,16.338440763967,17.3080983225917,18.2777558812165,
19.2474134398412,20.2170709984659,21.1867285570907,22.1563861157154,23.1260436743401,
24.0957012329649,25.0653587915896,26.0350163502143,27.0046739088391,27.9743314674638,
28.9439890260885,29.9136465847132,30.883304143338,31.8529617019627,32.8226192605874,
33.7922768192122,34.7619343778369,35.7315919364616,36.7012494950864,37.6709070537111,
38.6405646123358,39.6102221709606,40.5798797295853,41.54953728821),
 .UNSPECIFIED.);
#60=B_SPLINE_SURFACE_WITH_KNOTS('',3,3,((#31226,#31227,#31228,#31229,#31230,
#31231,#31232,#31233,#31234,#31235,#31236,#31237,#31238,#31239,#31240,#31241,
#31242,#31243,#31244,#31245,#31246,#31247,#31248,#31249,#31250,#31251,#31252,
#31253,#31254,#31255,#31256),(#31257,#31258,#31259,#31260,#31261,#31262,
#31263,#31264,#31265,#31266,#31267,#31268,#31269,#31270,#31271,#31272,#31273,
#31274,#31275,#31276,#31277,#31278,#31279,#31280,#31281,#31282,#31283,#31284,
#31285,#31286,#31287),(#31288,#31289,#31290,#31291,#31292,#31293,#31294,
#31295,#31296,#31297,#31298,#31299,#31300,#31301,#31302,#31303,#31304,#31305,
#31306,#31307,#31308,#31309,#31310,#31311,#31312,#31313,#31314,#31315,#31316,
#31317,#31318),(#31319,#31320,#31321,#31322,#31323,#31324,#31325,#31326,
#31327,#31328,#31329,#31330,#31331,#31332,#31333,#31334,#31335,#31336,#31337,
#31338,#31339,#31340,#31341,#31342,#31343,#31344,#31345,#31346,#31347,#31348,
#31349)),.UNSPECIFIED.,.F.,.F.,.F.,(4,4),(4,1,1,1,1,1,1,1,1,1,1,1,1,1,1,
1,1,1,1,1,1,1,1,1,1,1,1,1,4),(-0.000675443843025915,0.0807213590385511),
(11.8568623789734,12.8271953814412,13.7968529400659,14.7665104986906,15.7361680573154,
16.7058256159401,17.6754831745648,18.6451407331896,19.6147982918143,20.584455850439,
21.5541134090638,22.5237709676885,23.4934285263132,24.4630860849379,25.4327436435627,
26.4024012021874,27.3720587608121,28.3417163194369,29.3113738780616,30.2810314366863,
31.2506889953111,32.2203465539358,33.1900041125605,34.1596616711853,35.12931922981,
36.0989767884347,37.0686343470595,38.0382919056842,39.0079494643089),
 .UNSPECIFIED.);
#61=B_SPLINE_SURFACE_WITH_KNOTS('',3,3,((#31546,#31547,#31548,#31549,#31550,
#31551,#31552,#31553,#31554,#31555,#31556,#31557,#31558,#31559,#31560,#31561,
#31562,#31563,#31564,#31565,#31566,#31567,#31568,#31569,#31570,#31571,#31572,
#31573,#31574,#31575,#31576),(#31577,#31578,#31579,#31580,#31581,#31582,
#31583,#31584,#31585,#31586,#31587,#31588,#31589,#31590,#31591,#31592,#31593,
#31594,#31595,#31596,#31597,#31598,#31599,#31600,#31601,#31602,#31603,#31604,
#31605,#31606,#31607),(#31608,#31609,#31610,#31611,#31612,#31613,#31614,
#31615,#31616,#31617,#31618,#31619,#31620,#31621,#31622,#31623,#31624,#31625,
#31626,#31627,#31628,#31629,#31630,#31631,#31632,#31633,#31634,#31635,#31636,
#31637,#31638),(#31639,#31640,#31641,#31642,#31643,#31644,#31645,#31646,
#31647,#31648,#31649,#31650,#31651,#31652,#31653,#31654,#31655,#31656,#31657,
#31658,#31659,#31660,#31661,#31662,#31663,#31664,#31665,#31666,#31667,#31668,
#31669)),.UNSPECIFIED.,.F.,.F.,.F.,(4,4),(4,1,1,1,1,1,1,1,1,1,1,1,1,1,1,
1,1,1,1,1,1,1,1,1,1,1,1,1,4),(-0.000338746594202325,0.0807654267453605),
(14.3988578448057,15.3687832053423,16.338440763967,17.3080983225917,18.2777558812165,
19.2474134398412,20.2170709984659,21.1867285570907,22.1563861157154,23.1260436743401,
24.0957012329649,25.0653587915896,26.0350163502143,27.0046739088391,27.9743314674638,
28.9439890260885,29.9136465847132,30.883304143338,31.8529617019627,32.8226192605874,
33.7922768192122,34.7619343778369,35.7315919364616,36.7012494950864,37.6709070537111,
38.6405646123358,39.6102221709606,40.5798797295853,41.54953728821),
 .UNSPECIFIED.);
#62=B_SPLINE_SURFACE_WITH_KNOTS('',3,3,((#49814,#49815,#49816,#49817,#49818,
#49819,#49820,#49821,#49822,#49823,#49824,#49825,#49826,#49827,#49828,#49829,
#49830,#49831,#49832,#49833,#49834,#49835,#49836,#49837,#49838,#49839,#49840,
#49841,#49842,#49843,#49844,#49845,#49846,#49847,#49848,#49849,#49850,#49851,
#49852,#49853,#49854,#49855,#49856,#49857,#49858,#49859,#49860,#49861,#49862,
#49863,#49864,#49865,#49866,#49867,#49868,#49869,#49870,#49871,#49872,#49873,
#49874,#49875,#49876,#49877,#49878,#49879,#49880,#49881,#49882,#49883,#49884,
#49885,#49886,#49887,#49888,#49889,#49890,#49891,#49892,#49893,#49894,#49895,
#49896,#49897,#49898,#49899,#49900,#49901,#49902,#49903,#49904,#49905,#49906,
#49907,#49908,#49909,#49910,#49911,#49912,#49913,#49914,#49915,#49916,#49917,
#49918,#49919,#49920,#49921,#49922,#49923,#49924,#49925,#49926,#49927,#49928,
#49929,#49930,#49931,#49932,#49933,#49934,#49935,#49936,#49937,#49938,#49939,
#49940,#49941,#49942,#49943,#49944),(#49945,#49946,#49947,#49948,#49949,
#49950,#49951,#49952,#49953,#49954,#49955,#49956,#49957,#49958,#49959,#49960,
#49961,#49962,#49963,#49964,#49965,#49966,#49967,#49968,#49969,#49970,#49971,
#49972,#49973,#49974,#49975,#49976,#49977,#49978,#49979,#49980,#49981,#49982,
#49983,#49984,#49985,#49986,#49987,#49988,#49989,#49990,#49991,#49992,#49993,
#49994,#49995,#49996,#49997,#49998,#49999,#50000,#50001,#50002,#50003,#50004,
#50005,#50006,#50007,#50008,#50009,#50010,#50011,#50012,#50013,#50014,#50015,
#50016,#50017,#50018,#50019,#50020,#50021,#50022,#50023,#50024,#50025,#50026,
#50027,#50028,#50029,#50030,#50031,#50032,#50033,#50034,#50035,#50036,#50037,
#50038,#50039,#50040,#50041,#50042,#50043,#50044,#50045,#50046,#50047,#50048,
#50049,#50050,#50051,#50052,#50053,#50054,#50055,#50056,#50057,#50058,#50059,
#50060,#50061,#50062,#50063,#50064,#50065,#50066,#50067,#50068,#50069,#50070,
#50071,#50072,#50073,#50074,#50075),(#50076,#50077,#50078,#50079,#50080,
#50081,#50082,#50083,#50084,#50085,#50086,#50087,#50088,#50089,#50090,#50091,
#50092,#50093,#50094,#50095,#50096,#50097,#50098,#50099,#50100,#50101,#50102,
#50103,#50104,#50105,#50106,#50107,#50108,#50109,#50110,#50111,#50112,#50113,
#50114,#50115,#50116,#50117,#50118,#50119,#50120,#50121,#50122,#50123,#50124,
#50125,#50126,#50127,#50128,#50129,#50130,#50131,#50132,#50133,#50134,#50135,
#50136,#50137,#50138,#50139,#50140,#50141,#50142,#50143,#50144,#50145,#50146,
#50147,#50148,#50149,#50150,#50151,#50152,#50153,#50154,#50155,#50156,#50157,
#50158,#50159,#50160,#50161,#50162,#50163,#50164,#50165,#50166,#50167,#50168,
#50169,#50170,#50171,#50172,#50173,#50174,#50175,#50176,#50177,#50178,#50179,
#50180,#50181,#50182,#50183,#50184,#50185,#50186,#50187,#50188,#50189,#50190,
#50191,#50192,#50193,#50194,#50195,#50196,#50197,#50198,#50199,#50200,#50201,
#50202,#50203,#50204,#50205,#50206),(#50207,#50208,#50209,#50210,#50211,
#50212,#50213,#50214,#50215,#50216,#50217,#50218,#50219,#50220,#50221,#50222,
#50223,#50224,#50225,#50226,#50227,#50228,#50229,#50230,#50231,#50232,#50233,
#50234,#50235,#50236,#50237,#50238,#50239,#50240,#50241,#50242,#50243,#50244,
#50245,#50246,#50247,#50248,#50249,#50250,#50251,#50252,#50253,#50254,#50255,
#50256,#50257,#50258,#50259,#50260,#50261,#50262,#50263,#50264,#50265,#50266,
#50267,#50268,#50269,#50270,#50271,#50272,#50273,#50274,#50275,#50276,#50277,
#50278,#50279,#50280,#50281,#50282,#50283,#50284,#50285,#50286,#50287,#50288,
#50289,#50290,#50291,#50292,#50293,#50294,#50295,#50296,#50297,#50298,#50299,
#50300,#50301,#50302,#50303,#50304,#50305,#50306,#50307,#50308,#50309,#50310,
#50311,#50312,#50313,#50314,#50315,#50316,#50317,#50318,#50319,#50320,#50321,
#50322,#50323,#50324,#50325,#50326,#50327,#50328,#50329,#50330,#50331,#50332,
#50333,#50334,#50335,#50336,#50337)),.UNSPECIFIED.,.F.,.F.,.F.,(4,4),(4,
1,1,1,1,1,1,1,1,1,1,1,1,1,1,1,1,1,1,1,1,1,1,1,1,1,1,1,1,1,1,1,1,1,1,1,1,
1,1,1,1,1,1,1,1,1,1,1,1,1,1,1,1,1,1,1,1,1,1,1,1,1,1,1,1,1,1,1,1,1,1,1,1,
1,1,1,1,1,1,1,1,1,1,1,1,1,1,1,1,1,1,1,1,1,1,1,1,1,1,1,1,1,1,1,1,1,1,1,1,
1,1,1,1,1,1,1,1,1,1,1,1,1,1,1,1,1,1,1,4),(-0.000669933452207598,0.082357279631371),
(8.31473274985794,9.31258359158534,10.3104344333127,11.3082852750401,12.3061361167675,
13.3039869584949,14.3018378002224,15.2996886419498,16.2975394836772,17.2953903254046,
18.293241167132,19.2910920088594,20.2889428505868,21.2867936923142,22.2846445340416,
23.282495375769,24.2803462174964,25.2781970592238,26.2760479009512,27.2738987426786,
28.271749584406,29.2696004261334,30.2674512678608,31.2653021095882,32.2631529513156,
33.261003793043,34.2588546347704,35.2567054764978,36.2545563182252,37.2524071599526,
38.25025800168,39.2481088434074,40.2459596851348,41.2438105268622,42.2416613685896,
43.239512210317,44.2373630520444,45.2352138937718,46.2330647354992,47.2309155772266,
48.228766418954,49.2266172606814,50.2244681024088,51.2223189441362,52.2201697858636,
53.218020627591,54.2158714693185,55.2137223110459,56.2115731527733,57.2094239945007,
58.2072748362281,59.2051256779555,60.2029765196829,61.2008273614103,62.1986782031377,
63.1965290448651,64.1943798865925,65.1922307283199,66.1900815700473,67.1879324117747,
68.1857832535021,69.1836340952295,70.1814849369569,71.1793357786843,72.1771866204117,
73.1750374621391,74.1728883038665,75.1707391455939,76.1685899873213,77.1664408290487,
78.1642916707761,79.1621425125035,80.1599933542309,81.1578441959583,82.1556950376857,
83.1535458794131,84.1513967211405,85.1492475628679,86.1470984045953,87.1449492463227,
88.1428000880501,89.1406509297776,90.1385017715049,91.1363526132323,92.1342034549598,
93.1320542966872,94.1299051384146,95.127755980142,96.1256068218694,97.1234576635968,
98.1213085053242,99.1191593470516,100.117010188779,101.114861030506,102.112711872234,
103.110562713961,104.108413555689,105.106264397416,106.104115239143,107.101966080871,
108.099816922598,109.097667764326,110.095518606053,111.09336944778,112.091220289508,
113.089071131235,114.086921972963,115.08477281469,116.082623656417,117.080474498145,
118.078325339872,119.0761761816,120.074027023327,121.071877865054,122.069728706782,
123.067579548509,124.065430390237,125.063281231964,126.061132073691,127.058982915419,
128.056833757146,129.054684598874,130.052535440601,131.050386282328,132.048237124056,
133.046087965783,134.043938807511,135.041789649238,136.040310424417),
 .UNSPECIFIED.);
#63=B_SPLINE_SURFACE_WITH_KNOTS('',3,3,((#50529,#50530,#50531,#50532,#50533,
#50534,#50535,#50536,#50537,#50538,#50539,#50540,#50541,#50542,#50543,#50544,
#50545,#50546,#50547,#50548,#50549,#50550,#50551,#50552,#50553,#50554,#50555,
#50556,#50557,#50558,#50559,#50560,#50561,#50562,#50563,#50564,#50565,#50566,
#50567,#50568,#50569,#50570,#50571,#50572,#50573,#50574,#50575,#50576,#50577,
#50578,#50579,#50580,#50581,#50582,#50583,#50584,#50585,#50586,#50587,#50588,
#50589,#50590,#50591,#50592,#50593,#50594,#50595,#50596,#50597,#50598,#50599,
#50600,#50601,#50602,#50603,#50604,#50605,#50606,#50607,#50608,#50609,#50610,
#50611,#50612,#50613,#50614,#50615,#50616,#50617,#50618,#50619,#50620,#50621,
#50622,#50623,#50624,#50625,#50626,#50627,#50628,#50629,#50630,#50631,#50632,
#50633,#50634,#50635,#50636,#50637,#50638,#50639,#50640,#50641,#50642,#50643,
#50644,#50645,#50646,#50647,#50648,#50649,#50650,#50651,#50652,#50653,#50654,
#50655,#50656,#50657,#50658,#50659),(#50660,#50661,#50662,#50663,#50664,
#50665,#50666,#50667,#50668,#50669,#50670,#50671,#50672,#50673,#50674,#50675,
#50676,#50677,#50678,#50679,#50680,#50681,#50682,#50683,#50684,#50685,#50686,
#50687,#50688,#50689,#50690,#50691,#50692,#50693,#50694,#50695,#50696,#50697,
#50698,#50699,#50700,#50701,#50702,#50703,#50704,#50705,#50706,#50707,#50708,
#50709,#50710,#50711,#50712,#50713,#50714,#50715,#50716,#50717,#50718,#50719,
#50720,#50721,#50722,#50723,#50724,#50725,#50726,#50727,#50728,#50729,#50730,
#50731,#50732,#50733,#50734,#50735,#50736,#50737,#50738,#50739,#50740,#50741,
#50742,#50743,#50744,#50745,#50746,#50747,#50748,#50749,#50750,#50751,#50752,
#50753,#50754,#50755,#50756,#50757,#50758,#50759,#50760,#50761,#50762,#50763,
#50764,#50765,#50766,#50767,#50768,#50769,#50770,#50771,#50772,#50773,#50774,
#50775,#50776,#50777,#50778,#50779,#50780,#50781,#50782,#50783,#50784,#50785,
#50786,#50787,#50788,#50789,#50790),(#50791,#50792,#50793,#50794,#50795,
#50796,#50797,#50798,#50799,#50800,#50801,#50802,#50803,#50804,#50805,#50806,
#50807,#50808,#50809,#50810,#50811,#50812,#50813,#50814,#50815,#50816,#50817,
#50818,#50819,#50820,#50821,#50822,#50823,#50824,#50825,#50826,#50827,#50828,
#50829,#50830,#50831,#50832,#50833,#50834,#50835,#50836,#50837,#50838,#50839,
#50840,#50841,#50842,#50843,#50844,#50845,#50846,#50847,#50848,#50849,#50850,
#50851,#50852,#50853,#50854,#50855,#50856,#50857,#50858,#50859,#50860,#50861,
#50862,#50863,#50864,#50865,#50866,#50867,#50868,#50869,#50870,#50871,#50872,
#50873,#50874,#50875,#50876,#50877,#50878,#50879,#50880,#50881,#50882,#50883,
#50884,#50885,#50886,#50887,#50888,#50889,#50890,#50891,#50892,#50893,#50894,
#50895,#50896,#50897,#50898,#50899,#50900,#50901,#50902,#50903,#50904,#50905,
#50906,#50907,#50908,#50909,#50910,#50911,#50912,#50913,#50914,#50915,#50916,
#50917,#50918,#50919,#50920,#50921),(#50922,#50923,#50924,#50925,#50926,
#50927,#50928,#50929,#50930,#50931,#50932,#50933,#50934,#50935,#50936,#50937,
#50938,#50939,#50940,#50941,#50942,#50943,#50944,#50945,#50946,#50947,#50948,
#50949,#50950,#50951,#50952,#50953,#50954,#50955,#50956,#50957,#50958,#50959,
#50960,#50961,#50962,#50963,#50964,#50965,#50966,#50967,#50968,#50969,#50970,
#50971,#50972,#50973,#50974,#50975,#50976,#50977,#50978,#50979,#50980,#50981,
#50982,#50983,#50984,#50985,#50986,#50987,#50988,#50989,#50990,#50991,#50992,
#50993,#50994,#50995,#50996,#50997,#50998,#50999,#51000,#51001,#51002,#51003,
#51004,#51005,#51006,#51007,#51008,#51009,#51010,#51011,#51012,#51013,#51014,
#51015,#51016,#51017,#51018,#51019,#51020,#51021,#51022,#51023,#51024,#51025,
#51026,#51027,#51028,#51029,#51030,#51031,#51032,#51033,#51034,#51035,#51036,
#51037,#51038,#51039,#51040,#51041,#51042,#51043,#51044,#51045,#51046,#51047,
#51048,#51049,#51050,#51051,#51052)),.UNSPECIFIED.,.F.,.F.,.F.,(4,4),(4,
1,1,1,1,1,1,1,1,1,1,1,1,1,1,1,1,1,1,1,1,1,1,1,1,1,1,1,1,1,1,1,1,1,1,1,1,
1,1,1,1,1,1,1,1,1,1,1,1,1,1,1,1,1,1,1,1,1,1,1,1,1,1,1,1,1,1,1,1,1,1,1,1,
1,1,1,1,1,1,1,1,1,1,1,1,1,1,1,1,1,1,1,1,1,1,1,1,1,1,1,1,1,1,1,1,1,1,1,1,
1,1,1,1,1,1,1,1,1,1,1,1,1,1,1,1,1,1,1,4),(-0.000386098416431568,0.0827034127833099),
(11.6145234207097,12.613065069482,13.6109159112094,14.6087667529368,15.6066175946642,
16.6044684363917,17.6023192781191,18.6001701198465,19.5980209615739,20.5958718033013,
21.5937226450287,22.5915734867561,23.5894243284835,24.5872751702109,25.5851260119383,
26.5829768536657,27.5808276953931,28.5786785371205,29.5765293788479,30.5743802205753,
31.5722310623027,32.5700819040301,33.5679327457575,34.5657835874849,35.5636344292123,
36.5614852709397,37.5593361126671,38.5571869543945,39.5550377961219,40.5528886378493,
41.5507394795767,42.5485903213041,43.5464411630315,44.5442920047589,45.5421428464863,
46.5399936882137,47.5378445299411,48.5356953716685,49.5335462133959,50.5313970551233,
51.5292478968507,52.5270987385781,53.5249495803055,54.522800422033,55.5206512637604,
56.5185021054878,57.5163529472152,58.5142037889426,59.51205463067,60.5099054723974,
61.5077563141248,62.5056071558522,63.5034579975796,64.501308839307,65.4991596810344,
66.4970105227618,67.4948613644892,68.4927122062166,69.490563047944,70.4884138896714,
71.4862647313988,72.4841155731262,73.4819664148536,74.479817256581,75.4776680983084,
76.4755189400358,77.4733697817632,78.4712206234906,79.469071465218,80.4669223069454,
81.4647731486728,82.4626239904002,83.4604748321276,84.458325673855,85.4561765155824,
86.4540273573098,87.4518781990372,88.4497290407646,89.4475798824921,90.4454307242194,
91.4432815659468,92.4411324076742,93.4389832494017,94.4368340911291,95.4346849328565,
96.4325357745839,97.4303866163113,98.4282374580387,99.4260882997661,100.423939141493,
101.421789983221,102.419640824948,103.417491666676,104.415342508403,105.41319335013,
106.411044191858,107.408895033585,108.406745875313,109.40459671704,110.402447558768,
111.400298400495,112.398149242222,113.39600008395,114.393850925677,115.391701767405,
116.389552609132,117.387403450859,118.385254292587,119.383105134314,120.380955976042,
121.378806817769,122.376657659496,123.374508501224,124.372359342951,125.370210184679,
126.368061026406,127.365911868133,128.363762709861,129.361613551588,130.359464393316,
131.357315235043,132.35516607677,133.353016918498,134.350867760225,135.348718601953,
136.34656944368,137.344420285407,138.342271127135,139.340121968862),
 .UNSPECIFIED.);
#64=SHAPE_REPRESENTATION_RELATIONSHIP('SRR','None',#51585,#72);
#65=SHAPE_REPRESENTATION_RELATIONSHIP('SRR','None',#51586,#73);
#66=SHAPE_REPRESENTATION_RELATIONSHIP('SRR','None',#51587,#74);
#67=SHAPE_REPRESENTATION_RELATIONSHIP('SRR','None',#51588,#75);
#68=SHAPE_REPRESENTATION_RELATIONSHIP('SRR','None',#51589,#76);
#69=SHAPE_REPRESENTATION_RELATIONSHIP('SRR','None',#51590,#77);
#70=SHAPE_REPRESENTATION_RELATIONSHIP('SRR','None',#51591,#78);
#71=SHAPE_REPRESENTATION_RELATIONSHIP('SRR','None',#51592,#79);
#72=ADVANCED_BREP_SHAPE_REPRESENTATION('',(#89),#51545);
#73=ADVANCED_BREP_SHAPE_REPRESENTATION('',(#90),#51546);
#74=ADVANCED_BREP_SHAPE_REPRESENTATION('',(#91),#51547);
#75=ADVANCED_BREP_SHAPE_REPRESENTATION('',(#92),#51548);
#76=ADVANCED_BREP_SHAPE_REPRESENTATION('',(#93),#51549);
#77=ADVANCED_BREP_SHAPE_REPRESENTATION('',(#94),#51550);
#78=ADVANCED_BREP_SHAPE_REPRESENTATION('',(#95),#51551);
#79=ADVANCED_BREP_SHAPE_REPRESENTATION('',(#96,#97),#51552);
#80=STYLED_ITEM('',(#51634),#89);
#81=STYLED_ITEM('',(#51634),#90);
#82=STYLED_ITEM('',(#51634),#91);
#83=STYLED_ITEM('',(#51635),#92);
#84=STYLED_ITEM('',(#51634),#93);
#85=STYLED_ITEM('',(#51634),#94);
#86=STYLED_ITEM('',(#51634),#95);
#87=STYLED_ITEM('',(#51634),#96);
#88=STYLED_ITEM('',(#51634),#97);
#89=MANIFOLD_SOLID_BREP('Body1',#4259);
#90=MANIFOLD_SOLID_BREP('Body1',#4260);
#91=MANIFOLD_SOLID_BREP('Body1',#4261);
#92=MANIFOLD_SOLID_BREP('Body1',#4262);
#93=MANIFOLD_SOLID_BREP('Body1',#4263);
#94=MANIFOLD_SOLID_BREP('Body1',#4264);
#95=MANIFOLD_SOLID_BREP('Body1',#4265);
#96=MANIFOLD_SOLID_BREP('Body1',#4266);
#97=MANIFOLD_SOLID_BREP('Body2',#4267);
#98=FACE_BOUND('',#379,.T.);
#99=FACE_BOUND('',#382,.T.);
#100=FACE_BOUND('',#411,.T.);
#101=FACE_BOUND('',#412,.T.);
#102=FACE_BOUND('',#414,.T.);
#103=FACE_BOUND('',#415,.T.);
#104=FACE_BOUND('',#469,.T.);
#105=FACE_BOUND('',#477,.T.);
#106=FACE_BOUND('',#482,.T.);
#107=FACE_BOUND('',#484,.T.);
#108=FACE_BOUND('',#500,.T.);
#109=FACE_BOUND('',#508,.T.);
#110=FACE_BOUND('',#538,.T.);
#111=FACE_BOUND('',#541,.T.);
#112=FACE_BOUND('',#570,.T.);
#113=FACE_BOUND('',#571,.T.);
#114=FACE_BOUND('',#573,.T.);
#115=FACE_BOUND('',#574,.T.);
#116=FACE_BOUND('',#579,.T.);
#117=FACE_BOUND('',#583,.T.);
#118=FACE_BOUND('',#586,.T.);
#119=FACE_BOUND('',#591,.T.);
#120=PLANE('',#4363);
#121=PLANE('',#4365);
#122=PLANE('',#4371);
#123=PLANE('',#4372);
#124=PLANE('',#4383);
#125=PLANE('',#4386);
#126=PLANE('',#4390);
#127=PLANE('',#4394);
#128=PLANE('',#4398);
#129=PLANE('',#4402);
#130=PLANE('',#4415);
#131=PLANE('',#4419);
#132=PLANE('',#4423);
#133=PLANE('',#4427);
#134=PLANE('',#4428);
#135=PLANE('',#4429);
#136=PLANE('',#4448);
#137=PLANE('',#4451);
#138=PLANE('',#4465);
#139=PLANE('',#4481);
#140=PLANE('',#4482);
#141=PLANE('',#4483);
#142=PLANE('',#4484);
#143=PLANE('',#4485);
#144=PLANE('',#4486);
#145=PLANE('',#4487);
#146=PLANE('',#4488);
#147=PLANE('',#4499);
#148=PLANE('',#4500);
#149=PLANE('',#4522);
#150=PLANE('',#4523);
#151=PLANE('',#4524);
#152=PLANE('',#4525);
#153=PLANE('',#4526);
#154=PLANE('',#4527);
#155=PLANE('',#4528);
#156=PLANE('',#4529);
#157=PLANE('',#4557);
#158=PLANE('',#4558);
#159=PLANE('',#4564);
#160=PLANE('',#4566);
#161=PLANE('',#4572);
#162=PLANE('',#4573);
#163=PLANE('',#4584);
#164=PLANE('',#4587);
#165=PLANE('',#4591);
#166=PLANE('',#4595);
#167=PLANE('',#4599);
#168=PLANE('',#4603);
#169=PLANE('',#4616);
#170=PLANE('',#4620);
#171=PLANE('',#4624);
#172=PLANE('',#4628);
#173=PLANE('',#4629);
#174=PLANE('',#4630);
#175=PLANE('',#4632);
#176=PLANE('',#4637);
#177=PLANE('',#4639);
#178=PLANE('',#4658);
#179=PLANE('',#4661);
#180=PLANE('',#4662);
#181=FACE_OUTER_BOUND('',#376,.T.);
#182=FACE_OUTER_BOUND('',#377,.T.);
#183=FACE_OUTER_BOUND('',#378,.T.);
#184=FACE_OUTER_BOUND('',#380,.T.);
#185=FACE_OUTER_BOUND('',#381,.T.);
#186=FACE_OUTER_BOUND('',#383,.T.);
#187=FACE_OUTER_BOUND('',#384,.T.);
#188=FACE_OUTER_BOUND('',#385,.T.);
#189=FACE_OUTER_BOUND('',#386,.T.);
#190=FACE_OUTER_BOUND('',#387,.T.);
#191=FACE_OUTER_BOUND('',#388,.T.);
#192=FACE_OUTER_BOUND('',#389,.T.);
#193=FACE_OUTER_BOUND('',#390,.T.);
#194=FACE_OUTER_BOUND('',#391,.T.);
#195=FACE_OUTER_BOUND('',#392,.T.);
#196=FACE_OUTER_BOUND('',#393,.T.);
#197=FACE_OUTER_BOUND('',#394,.T.);
#198=FACE_OUTER_BOUND('',#395,.T.);
#199=FACE_OUTER_BOUND('',#396,.T.);
#200=FACE_OUTER_BOUND('',#397,.T.);
#201=FACE_OUTER_BOUND('',#398,.T.);
#202=FACE_OUTER_BOUND('',#399,.T.);
#203=FACE_OUTER_BOUND('',#400,.T.);
#204=FACE_OUTER_BOUND('',#401,.T.);
#205=FACE_OUTER_BOUND('',#402,.T.);
#206=FACE_OUTER_BOUND('',#403,.T.);
#207=FACE_OUTER_BOUND('',#404,.T.);
#208=FACE_OUTER_BOUND('',#405,.T.);
#209=FACE_OUTER_BOUND('',#406,.T.);
#210=FACE_OUTER_BOUND('',#407,.T.);
#211=FACE_OUTER_BOUND('',#408,.T.);
#212=FACE_OUTER_BOUND('',#409,.T.);
#213=FACE_OUTER_BOUND('',#410,.T.);
#214=FACE_OUTER_BOUND('',#413,.T.);
#215=FACE_OUTER_BOUND('',#416,.T.);
#216=FACE_OUTER_BOUND('',#417,.T.);
#217=FACE_OUTER_BOUND('',#418,.T.);
#218=FACE_OUTER_BOUND('',#419,.T.);
#219=FACE_OUTER_BOUND('',#420,.T.);
#220=FACE_OUTER_BOUND('',#421,.T.);
#221=FACE_OUTER_BOUND('',#422,.T.);
#222=FACE_OUTER_BOUND('',#423,.T.);
#223=FACE_OUTER_BOUND('',#424,.T.);
#224=FACE_OUTER_BOUND('',#425,.T.);
#225=FACE_OUTER_BOUND('',#426,.T.);
#226=FACE_OUTER_BOUND('',#427,.T.);
#227=FACE_OUTER_BOUND('',#428,.T.);
#228=FACE_OUTER_BOUND('',#429,.T.);
#229=FACE_OUTER_BOUND('',#430,.T.);
#230=FACE_OUTER_BOUND('',#431,.T.);
#231=FACE_OUTER_BOUND('',#432,.T.);
#232=FACE_OUTER_BOUND('',#433,.T.);
#233=FACE_OUTER_BOUND('',#434,.T.);
#234=FACE_OUTER_BOUND('',#435,.T.);
#235=FACE_OUTER_BOUND('',#436,.T.);
#236=FACE_OUTER_BOUND('',#437,.T.);
#237=FACE_OUTER_BOUND('',#438,.T.);
#238=FACE_OUTER_BOUND('',#439,.T.);
#239=FACE_OUTER_BOUND('',#440,.T.);
#240=FACE_OUTER_BOUND('',#441,.T.);
#241=FACE_OUTER_BOUND('',#442,.T.);
#242=FACE_OUTER_BOUND('',#443,.T.);
#243=FACE_OUTER_BOUND('',#444,.T.);
#244=FACE_OUTER_BOUND('',#445,.T.);
#245=FACE_OUTER_BOUND('',#446,.T.);
#246=FACE_OUTER_BOUND('',#447,.T.);
#247=FACE_OUTER_BOUND('',#448,.T.);
#248=FACE_OUTER_BOUND('',#449,.T.);
#249=FACE_OUTER_BOUND('',#450,.T.);
#250=FACE_OUTER_BOUND('',#451,.T.);
#251=FACE_OUTER_BOUND('',#452,.T.);
#252=FACE_OUTER_BOUND('',#453,.T.);
#253=FACE_OUTER_BOUND('',#454,.T.);
#254=FACE_OUTER_BOUND('',#455,.T.);
#255=FACE_OUTER_BOUND('',#456,.T.);
#256=FACE_OUTER_BOUND('',#457,.T.);
#257=FACE_OUTER_BOUND('',#458,.T.);
#258=FACE_OUTER_BOUND('',#459,.T.);
#259=FACE_OUTER_BOUND('',#460,.T.);
#260=FACE_OUTER_BOUND('',#461,.T.);
#261=FACE_OUTER_BOUND('',#462,.T.);
#262=FACE_OUTER_BOUND('',#463,.T.);
#263=FACE_OUTER_BOUND('',#464,.T.);
#264=FACE_OUTER_BOUND('',#465,.T.);
#265=FACE_OUTER_BOUND('',#466,.T.);
#266=FACE_OUTER_BOUND('',#467,.T.);
#267=FACE_OUTER_BOUND('',#468,.T.);
#268=FACE_OUTER_BOUND('',#470,.T.);
#269=FACE_OUTER_BOUND('',#471,.T.);
#270=FACE_OUTER_BOUND('',#472,.T.);
#271=FACE_OUTER_BOUND('',#473,.T.);
#272=FACE_OUTER_BOUND('',#474,.T.);
#273=FACE_OUTER_BOUND('',#475,.T.);
#274=FACE_OUTER_BOUND('',#476,.T.);
#275=FACE_OUTER_BOUND('',#478,.T.);
#276=FACE_OUTER_BOUND('',#479,.T.);
#277=FACE_OUTER_BOUND('',#480,.T.);
#278=FACE_OUTER_BOUND('',#481,.T.);
#279=FACE_OUTER_BOUND('',#483,.T.);
#280=FACE_OUTER_BOUND('',#485,.T.);
#281=FACE_OUTER_BOUND('',#486,.T.);
#282=FACE_OUTER_BOUND('',#487,.T.);
#283=FACE_OUTER_BOUND('',#488,.T.);
#284=FACE_OUTER_BOUND('',#489,.T.);
#285=FACE_OUTER_BOUND('',#490,.T.);
#286=FACE_OUTER_BOUND('',#491,.T.);
#287=FACE_OUTER_BOUND('',#492,.T.);
#288=FACE_OUTER_BOUND('',#493,.T.);
#289=FACE_OUTER_BOUND('',#494,.T.);
#290=FACE_OUTER_BOUND('',#495,.T.);
#291=FACE_OUTER_BOUND('',#496,.T.);
#292=FACE_OUTER_BOUND('',#497,.T.);
#293=FACE_OUTER_BOUND('',#498,.T.);
#294=FACE_OUTER_BOUND('',#499,.T.);
#295=FACE_OUTER_BOUND('',#501,.T.);
#296=FACE_OUTER_BOUND('',#502,.T.);
#297=FACE_OUTER_BOUND('',#503,.T.);
#298=FACE_OUTER_BOUND('',#504,.T.);
#299=FACE_OUTER_BOUND('',#505,.T.);
#300=FACE_OUTER_BOUND('',#506,.T.);
#301=FACE_OUTER_BOUND('',#507,.T.);
#302=FACE_OUTER_BOUND('',#509,.T.);
#303=FACE_OUTER_BOUND('',#510,.T.);
#304=FACE_OUTER_BOUND('',#511,.T.);
#305=FACE_OUTER_BOUND('',#512,.T.);
#306=FACE_OUTER_BOUND('',#513,.T.);
#307=FACE_OUTER_BOUND('',#514,.T.);
#308=FACE_OUTER_BOUND('',#515,.T.);
#309=FACE_OUTER_BOUND('',#516,.T.);
#310=FACE_OUTER_BOUND('',#517,.T.);
#311=FACE_OUTER_BOUND('',#518,.T.);
#312=FACE_OUTER_BOUND('',#519,.T.);
#313=FACE_OUTER_BOUND('',#520,.T.);
#314=FACE_OUTER_BOUND('',#521,.T.);
#315=FACE_OUTER_BOUND('',#522,.T.);
#316=FACE_OUTER_BOUND('',#523,.T.);
#317=FACE_OUTER_BOUND('',#524,.T.);
#318=FACE_OUTER_BOUND('',#525,.T.);
#319=FACE_OUTER_BOUND('',#526,.T.);
#320=FACE_OUTER_BOUND('',#527,.T.);
#321=FACE_OUTER_BOUND('',#528,.T.);
#322=FACE_OUTER_BOUND('',#529,.T.);
#323=FACE_OUTER_BOUND('',#530,.T.);
#324=FACE_OUTER_BOUND('',#531,.T.);
#325=FACE_OUTER_BOUND('',#532,.T.);
#326=FACE_OUTER_BOUND('',#533,.T.);
#327=FACE_OUTER_BOUND('',#534,.T.);
#328=FACE_OUTER_BOUND('',#535,.T.);
#329=FACE_OUTER_BOUND('',#536,.T.);
#330=FACE_OUTER_BOUND('',#537,.T.);
#331=FACE_OUTER_BOUND('',#539,.T.);
#332=FACE_OUTER_BOUND('',#540,.T.);
#333=FACE_OUTER_BOUND('',#542,.T.);
#334=FACE_OUTER_BOUND('',#543,.T.);
#335=FACE_OUTER_BOUND('',#544,.T.);
#336=FACE_OUTER_BOUND('',#545,.T.);
#337=FACE_OUTER_BOUND('',#546,.T.);
#338=FACE_OUTER_BOUND('',#547,.T.);
#339=FACE_OUTER_BOUND('',#548,.T.);
#340=FACE_OUTER_BOUND('',#549,.T.);
#341=FACE_OUTER_BOUND('',#550,.T.);
#342=FACE_OUTER_BOUND('',#551,.T.);
#343=FACE_OUTER_BOUND('',#552,.T.);
#344=FACE_OUTER_BOUND('',#553,.T.);
#345=FACE_OUTER_BOUND('',#554,.T.);
#346=FACE_OUTER_BOUND('',#555,.T.);
#347=FACE_OUTER_BOUND('',#556,.T.);
#348=FACE_OUTER_BOUND('',#557,.T.);
#349=FACE_OUTER_BOUND('',#558,.T.);
#350=FACE_OUTER_BOUND('',#559,.T.);
#351=FACE_OUTER_BOUND('',#560,.T.);
#352=FACE_OUTER_BOUND('',#561,.T.);
#353=FACE_OUTER_BOUND('',#562,.T.);
#354=FACE_OUTER_BOUND('',#563,.T.);
#355=FACE_OUTER_BOUND('',#564,.T.);
#356=FACE_OUTER_BOUND('',#565,.T.);
#357=FACE_OUTER_BOUND('',#566,.T.);
#358=FACE_OUTER_BOUND('',#567,.T.);
#359=FACE_OUTER_BOUND('',#568,.T.);
#360=FACE_OUTER_BOUND('',#569,.T.);
#361=FACE_OUTER_BOUND('',#572,.T.);
#362=FACE_OUTER_BOUND('',#575,.T.);
#363=FACE_OUTER_BOUND('',#576,.T.);
#364=FACE_OUTER_BOUND('',#577,.T.);
#365=FACE_OUTER_BOUND('',#578,.T.);
#366=FACE_OUTER_BOUND('',#580,.T.);
#367=FACE_OUTER_BOUND('',#581,.T.);
#368=FACE_OUTER_BOUND('',#582,.T.);
#369=FACE_OUTER_BOUND('',#584,.T.);
#370=FACE_OUTER_BOUND('',#585,.T.);
#371=FACE_OUTER_BOUND('',#587,.T.);
#372=FACE_OUTER_BOUND('',#588,.T.);
#373=FACE_OUTER_BOUND('',#589,.T.);
#374=FACE_OUTER_BOUND('',#590,.T.);
#375=FACE_OUTER_BOUND('',#592,.T.);
#376=EDGE_LOOP('',(#2629,#2630,#2631,#2632,#2633,#2634,#2635));
#377=EDGE_LOOP('',(#2636,#2637,#2638,#2639,#2640,#2641));
#378=EDGE_LOOP('',(#2642,#2643,#2644,#2645,#2646,#2647,#2648,#2649,#2650,
#2651));
#379=EDGE_LOOP('',(#2652));
#380=EDGE_LOOP('',(#2653,#2654,#2655,#2656));
#381=EDGE_LOOP('',(#2657,#2658,#2659,#2660,#2661,#2662,#2663,#2664));
#382=EDGE_LOOP('',(#2665));
#383=EDGE_LOOP('',(#2666,#2667,#2668,#2669));
#384=EDGE_LOOP('',(#2670,#2671,#2672,#2673));
#385=EDGE_LOOP('',(#2674,#2675,#2676,#2677));
#386=EDGE_LOOP('',(#2678,#2679,#2680,#2681));
#387=EDGE_LOOP('',(#2682,#2683,#2684,#2685));
#388=EDGE_LOOP('',(#2686,#2687,#2688,#2689));
#389=EDGE_LOOP('',(#2690,#2691,#2692,#2693));
#390=EDGE_LOOP('',(#2694,#2695,#2696,#2697,#2698,#2699,#2700));
#391=EDGE_LOOP('',(#2701,#2702,#2703,#2704));
#392=EDGE_LOOP('',(#2705,#2706,#2707,#2708));
#393=EDGE_LOOP('',(#2709,#2710,#2711,#2712));
#394=EDGE_LOOP('',(#2713,#2714,#2715,#2716));
#395=EDGE_LOOP('',(#2717,#2718,#2719,#2720));
#396=EDGE_LOOP('',(#2721,#2722,#2723,#2724));
#397=EDGE_LOOP('',(#2725,#2726,#2727,#2728));
#398=EDGE_LOOP('',(#2729,#2730,#2731,#2732));
#399=EDGE_LOOP('',(#2733,#2734,#2735,#2736));
#400=EDGE_LOOP('',(#2737,#2738,#2739,#2740));
#401=EDGE_LOOP('',(#2741,#2742,#2743,#2744,#2745));
#402=EDGE_LOOP('',(#2746,#2747,#2748,#2749));
#403=EDGE_LOOP('',(#2750,#2751,#2752,#2753));
#404=EDGE_LOOP('',(#2754,#2755,#2756,#2757));
#405=EDGE_LOOP('',(#2758,#2759,#2760,#2761));
#406=EDGE_LOOP('',(#2762,#2763,#2764,#2765));
#407=EDGE_LOOP('',(#2766,#2767,#2768,#2769));
#408=EDGE_LOOP('',(#2770,#2771,#2772,#2773));
#409=EDGE_LOOP('',(#2774,#2775,#2776,#2777));
#410=EDGE_LOOP('',(#2778,#2779,#2780,#2781,#2782,#2783,#2784,#2785,#2786,
#2787,#2788,#2789,#2790));
#411=EDGE_LOOP('',(#2791,#2792,#2793,#2794,#2795,#2796,#2797,#2798));
#412=EDGE_LOOP('',(#2799));
#413=EDGE_LOOP('',(#2800,#2801,#2802,#2803,#2804,#2805,#2806,#2807,#2808,
#2809,#2810,#2811));
#414=EDGE_LOOP('',(#2812,#2813,#2814,#2815,#2816,#2817,#2818,#2819));
#415=EDGE_LOOP('',(#2820));
#416=EDGE_LOOP('',(#2821,#2822,#2823,#2824));
#417=EDGE_LOOP('',(#2825,#2826,#2827,#2828));
#418=EDGE_LOOP('',(#2829,#2830,#2831,#2832));
#419=EDGE_LOOP('',(#2833,#2834,#2835,#2836,#2837));
#420=EDGE_LOOP('',(#2838,#2839,#2840,#2841,#2842));
#421=EDGE_LOOP('',(#2843,#2844,#2845,#2846));
#422=EDGE_LOOP('',(#2847,#2848,#2849,#2850,#2851));
#423=EDGE_LOOP('',(#2852,#2853,#2854,#2855,#2856,#2857));
#424=EDGE_LOOP('',(#2858,#2859,#2860,#2861,#2862));
#425=EDGE_LOOP('',(#2863,#2864,#2865,#2866));
#426=EDGE_LOOP('',(#2867,#2868,#2869,#2870,#2871));
#427=EDGE_LOOP('',(#2872,#2873,#2874,#2875,#2876));
#428=EDGE_LOOP('',(#2877,#2878,#2879,#2880));
#429=EDGE_LOOP('',(#2881,#2882,#2883,#2884,#2885));
#430=EDGE_LOOP('',(#2886,#2887,#2888,#2889,#2890));
#431=EDGE_LOOP('',(#2891,#2892,#2893,#2894,#2895));
#432=EDGE_LOOP('',(#2896,#2897,#2898,#2899,#2900,#2901,#2902,#2903,#2904,
#2905,#2906,#2907,#2908,#2909,#2910,#2911,#2912,#2913,#2914,#2915,#2916,
#2917,#2918,#2919,#2920,#2921,#2922,#2923));
#433=EDGE_LOOP('',(#2924,#2925,#2926,#2927,#2928,#2929,#2930,#2931,#2932,
#2933));
#434=EDGE_LOOP('',(#2934,#2935,#2936,#2937,#2938,#2939,#2940));
#435=EDGE_LOOP('',(#2941,#2942,#2943,#2944,#2945,#2946,#2947,#2948,#2949,
#2950,#2951,#2952,#2953,#2954,#2955,#2956,#2957,#2958,#2959,#2960,#2961,
#2962,#2963,#2964,#2965,#2966,#2967,#2968,#2969,#2970,#2971,#2972,#2973,
#2974,#2975,#2976));
#436=EDGE_LOOP('',(#2977,#2978,#2979,#2980));
#437=EDGE_LOOP('',(#2981,#2982,#2983,#2984));
#438=EDGE_LOOP('',(#2985,#2986,#2987,#2988));
#439=EDGE_LOOP('',(#2989,#2990,#2991,#2992,#2993,#2994,#2995,#2996,#2997,
#2998,#2999,#3000,#3001,#3002,#3003,#3004,#3005,#3006,#3007,#3008,#3009,
#3010,#3011,#3012,#3013,#3014,#3015,#3016,#3017,#3018,#3019,#3020,#3021,
#3022,#3023,#3024,#3025,#3026,#3027,#3028,#3029,#3030,#3031));
#440=EDGE_LOOP('',(#3032,#3033,#3034,#3035));
#441=EDGE_LOOP('',(#3036,#3037,#3038,#3039));
#442=EDGE_LOOP('',(#3040,#3041,#3042,#3043));
#443=EDGE_LOOP('',(#3044,#3045,#3046,#3047));
#444=EDGE_LOOP('',(#3048,#3049,#3050,#3051));
#445=EDGE_LOOP('',(#3052,#3053,#3054,#3055));
#446=EDGE_LOOP('',(#3056,#3057,#3058,#3059));
#447=EDGE_LOOP('',(#3060,#3061,#3062,#3063,#3064,#3065,#3066,#3067,#3068,
#3069,#3070,#3071,#3072,#3073,#3074,#3075,#3076,#3077,#3078,#3079,#3080,
#3081,#3082,#3083,#3084,#3085,#3086,#3087,#3088,#3089,#3090,#3091,#3092,
#3093,#3094,#3095,#3096,#3097,#3098,#3099,#3100,#3101,#3102,#3103));
#448=EDGE_LOOP('',(#3104,#3105,#3106,#3107,#3108));
#449=EDGE_LOOP('',(#3109,#3110,#3111,#3112));
#450=EDGE_LOOP('',(#3113,#3114,#3115,#3116,#3117,#3118));
#451=EDGE_LOOP('',(#3119,#3120,#3121,#3122));
#452=EDGE_LOOP('',(#3123,#3124,#3125,#3126));
#453=EDGE_LOOP('',(#3127,#3128,#3129));
#454=EDGE_LOOP('',(#3130,#3131,#3132,#3133));
#455=EDGE_LOOP('',(#3134,#3135,#3136,#3137,#3138));
#456=EDGE_LOOP('',(#3139,#3140,#3141,#3142));
#457=EDGE_LOOP('',(#3143,#3144,#3145,#3146,#3147,#3148));
#458=EDGE_LOOP('',(#3149,#3150,#3151,#3152,#3153,#3154));
#459=EDGE_LOOP('',(#3155,#3156,#3157,#3158,#3159,#3160));
#460=EDGE_LOOP('',(#3161,#3162,#3163,#3164,#3165));
#461=EDGE_LOOP('',(#3166,#3167,#3168,#3169,#3170));
#462=EDGE_LOOP('',(#3171,#3172,#3173,#3174,#3175));
#463=EDGE_LOOP('',(#3176,#3177,#3178,#3179,#3180));
#464=EDGE_LOOP('',(#3181,#3182,#3183,#3184));
#465=EDGE_LOOP('',(#3185,#3186,#3187,#3188,#3189,#3190));
#466=EDGE_LOOP('',(#3191,#3192,#3193,#3194,#3195,#3196,#3197,#3198,#3199,
#3200,#3201,#3202,#3203,#3204,#3205,#3206,#3207));
#467=EDGE_LOOP('',(#3208,#3209,#3210,#3211,#3212,#3213,#3214,#3215,#3216,
#3217,#3218,#3219,#3220,#3221,#3222,#3223,#3224,#3225,#3226,#3227));
#468=EDGE_LOOP('',(#3228,#3229,#3230,#3231,#3232,#3233));
#469=EDGE_LOOP('',(#3234,#3235,#3236,#3237));
#470=EDGE_LOOP('',(#3238,#3239,#3240,#3241));
#471=EDGE_LOOP('',(#3242,#3243,#3244,#3245));
#472=EDGE_LOOP('',(#3246,#3247,#3248,#3249));
#473=EDGE_LOOP('',(#3250,#3251,#3252,#3253));
#474=EDGE_LOOP('',(#3254,#3255,#3256,#3257));
#475=EDGE_LOOP('',(#3258,#3259,#3260,#3261));
#476=EDGE_LOOP('',(#3262,#3263,#3264,#3265,#3266,#3267));
#477=EDGE_LOOP('',(#3268,#3269,#3270,#3271,#3272));
#478=EDGE_LOOP('',(#3273,#3274,#3275,#3276));
#479=EDGE_LOOP('',(#3277,#3278,#3279,#3280));
#480=EDGE_LOOP('',(#3281,#3282,#3283,#3284));
#481=EDGE_LOOP('',(#3285));
#482=EDGE_LOOP('',(#3286));
#483=EDGE_LOOP('',(#3287));
#484=EDGE_LOOP('',(#3288));
#485=EDGE_LOOP('',(#3289,#3290,#3291,#3292));
#486=EDGE_LOOP('',(#3293,#3294,#3295,#3296));
#487=EDGE_LOOP('',(#3297,#3298,#3299,#3300));
#488=EDGE_LOOP('',(#3301,#3302,#3303,#3304,#3305,#3306));
#489=EDGE_LOOP('',(#3307,#3308,#3309,#3310,#3311,#3312));
#490=EDGE_LOOP('',(#3313,#3314,#3315,#3316,#3317,#3318));
#491=EDGE_LOOP('',(#3319,#3320,#3321,#3322,#3323));
#492=EDGE_LOOP('',(#3324,#3325,#3326,#3327,#3328,#3329));
#493=EDGE_LOOP('',(#3330,#3331,#3332,#3333,#3334));
#494=EDGE_LOOP('',(#3335,#3336,#3337,#3338));
#495=EDGE_LOOP('',(#3339,#3340,#3341,#3342,#3343,#3344));
#496=EDGE_LOOP('',(#3345,#3346,#3347,#3348,#3349,#3350));
#497=EDGE_LOOP('',(#3351,#3352,#3353,#3354,#3355,#3356,#3357,#3358,#3359,
#3360,#3361,#3362,#3363,#3364,#3365,#3366,#3367,#3368,#3369));
#498=EDGE_LOOP('',(#3370,#3371,#3372,#3373,#3374,#3375,#3376,#3377,#3378,
#3379,#3380,#3381,#3382,#3383,#3384,#3385,#3386,#3387,#3388,#3389));
#499=EDGE_LOOP('',(#3390,#3391,#3392,#3393,#3394,#3395));
#500=EDGE_LOOP('',(#3396,#3397,#3398,#3399));
#501=EDGE_LOOP('',(#3400,#3401,#3402,#3403));
#502=EDGE_LOOP('',(#3404,#3405,#3406,#3407));
#503=EDGE_LOOP('',(#3408,#3409,#3410,#3411));
#504=EDGE_LOOP('',(#3412,#3413,#3414,#3415));
#505=EDGE_LOOP('',(#3416,#3417,#3418,#3419));
#506=EDGE_LOOP('',(#3420,#3421,#3422,#3423));
#507=EDGE_LOOP('',(#3424,#3425,#3426,#3427,#3428,#3429));
#508=EDGE_LOOP('',(#3430,#3431,#3432,#3433,#3434));
#509=EDGE_LOOP('',(#3435,#3436,#3437,#3438));
#510=EDGE_LOOP('',(#3439,#3440,#3441,#3442,#3443));
#511=EDGE_LOOP('',(#3444,#3445,#3446,#3447,#3448));
#512=EDGE_LOOP('',(#3449,#3450,#3451,#3452,#3453));
#513=EDGE_LOOP('',(#3454,#3455,#3456,#3457,#3458));
#514=EDGE_LOOP('',(#3459,#3460,#3461,#3462,#3463));
#515=EDGE_LOOP('',(#3464,#3465,#3466,#3467,#3468));
#516=EDGE_LOOP('',(#3469,#3470,#3471,#3472,#3473));
#517=EDGE_LOOP('',(#3474,#3475,#3476,#3477,#3478));
#518=EDGE_LOOP('',(#3479,#3480,#3481,#3482,#3483));
#519=EDGE_LOOP('',(#3484,#3485,#3486,#3487,#3488));
#520=EDGE_LOOP('',(#3489,#3490,#3491,#3492,#3493));
#521=EDGE_LOOP('',(#3494,#3495,#3496,#3497,#3498));
#522=EDGE_LOOP('',(#3499,#3500,#3501,#3502,#3503));
#523=EDGE_LOOP('',(#3504,#3505,#3506,#3507,#3508));
#524=EDGE_LOOP('',(#3509,#3510,#3511,#3512,#3513));
#525=EDGE_LOOP('',(#3514,#3515,#3516,#3517,#3518));
#526=EDGE_LOOP('',(#3519,#3520,#3521,#3522,#3523));
#527=EDGE_LOOP('',(#3524,#3525,#3526,#3527,#3528));
#528=EDGE_LOOP('',(#3529,#3530,#3531,#3532,#3533,#3534));
#529=EDGE_LOOP('',(#3535,#3536,#3537,#3538,#3539,#3540,#3541,#3542,#3543,
#3544,#3545,#3546,#3547,#3548,#3549,#3550,#3551,#3552,#3553,#3554,#3555,
#3556,#3557,#3558,#3559,#3560,#3561,#3562,#3563,#3564,#3565,#3566,#3567,
#3568,#3569,#3570,#3571,#3572,#3573,#3574,#3575,#3576,#3577,#3578));
#530=EDGE_LOOP('',(#3579,#3580,#3581,#3582,#3583));
#531=EDGE_LOOP('',(#3584,#3585,#3586,#3587,#3588,#3589,#3590,#3591,#3592,
#3593,#3594,#3595,#3596,#3597,#3598,#3599,#3600,#3601,#3602,#3603,#3604,
#3605,#3606,#3607,#3608,#3609,#3610,#3611,#3612,#3613,#3614,#3615,#3616,
#3617,#3618,#3619,#3620,#3621,#3622,#3623,#3624,#3625,#3626,#3627,#3628,
#3629,#3630,#3631,#3632,#3633,#3634,#3635,#3636,#3637,#3638));
#532=EDGE_LOOP('',(#3639,#3640,#3641,#3642,#3643,#3644,#3645,#3646,#3647,
#3648,#3649,#3650,#3651,#3652,#3653,#3654,#3655,#3656,#3657,#3658,#3659,
#3660,#3661,#3662,#3663,#3664,#3665,#3666,#3667,#3668,#3669,#3670,#3671,
#3672,#3673,#3674,#3675,#3676,#3677,#3678,#3679,#3680,#3681,#3682,#3683,
#3684,#3685,#3686,#3687,#3688,#3689,#3690,#3691,#3692,#3693));
#533=EDGE_LOOP('',(#3694,#3695,#3696,#3697,#3698));
#534=EDGE_LOOP('',(#3699,#3700,#3701,#3702));
#535=EDGE_LOOP('',(#3703,#3704,#3705,#3706,#3707,#3708,#3709));
#536=EDGE_LOOP('',(#3710,#3711,#3712,#3713,#3714,#3715));
#537=EDGE_LOOP('',(#3716,#3717,#3718,#3719,#3720,#3721,#3722,#3723,#3724,
#3725));
#538=EDGE_LOOP('',(#3726));
#539=EDGE_LOOP('',(#3727,#3728,#3729,#3730));
#540=EDGE_LOOP('',(#3731,#3732,#3733,#3734,#3735,#3736,#3737,#3738));
#541=EDGE_LOOP('',(#3739));
#542=EDGE_LOOP('',(#3740,#3741,#3742,#3743));
#543=EDGE_LOOP('',(#3744,#3745,#3746,#3747));
#544=EDGE_LOOP('',(#3748,#3749,#3750,#3751));
#545=EDGE_LOOP('',(#3752,#3753,#3754,#3755));
#546=EDGE_LOOP('',(#3756,#3757,#3758,#3759));
#547=EDGE_LOOP('',(#3760,#3761,#3762,#3763));
#548=EDGE_LOOP('',(#3764,#3765,#3766,#3767));
#549=EDGE_LOOP('',(#3768,#3769,#3770,#3771,#3772,#3773,#3774));
#550=EDGE_LOOP('',(#3775,#3776,#3777,#3778));
#551=EDGE_LOOP('',(#3779,#3780,#3781,#3782));
#552=EDGE_LOOP('',(#3783,#3784,#3785,#3786));
#553=EDGE_LOOP('',(#3787,#3788,#3789,#3790));
#554=EDGE_LOOP('',(#3791,#3792,#3793,#3794));
#555=EDGE_LOOP('',(#3795,#3796,#3797,#3798));
#556=EDGE_LOOP('',(#3799,#3800,#3801,#3802));
#557=EDGE_LOOP('',(#3803,#3804,#3805,#3806));
#558=EDGE_LOOP('',(#3807,#3808,#3809,#3810));
#559=EDGE_LOOP('',(#3811,#3812,#3813,#3814));
#560=EDGE_LOOP('',(#3815,#3816,#3817,#3818,#3819));
#561=EDGE_LOOP('',(#3820,#3821,#3822,#3823));
#562=EDGE_LOOP('',(#3824,#3825,#3826,#3827));
#563=EDGE_LOOP('',(#3828,#3829,#3830,#3831));
#564=EDGE_LOOP('',(#3832,#3833,#3834,#3835));
#565=EDGE_LOOP('',(#3836,#3837,#3838,#3839));
#566=EDGE_LOOP('',(#3840,#3841,#3842,#3843));
#567=EDGE_LOOP('',(#3844,#3845,#3846,#3847));
#568=EDGE_LOOP('',(#3848,#3849,#3850,#3851));
#569=EDGE_LOOP('',(#3852,#3853,#3854,#3855,#3856,#3857,#3858,#3859,#3860,
#3861,#3862,#3863,#3864));
#570=EDGE_LOOP('',(#3865,#3866,#3867,#3868,#3869,#3870,#3871,#3872));
#571=EDGE_LOOP('',(#3873));
#572=EDGE_LOOP('',(#3874,#3875,#3876,#3877,#3878,#3879,#3880,#3881,#3882,
#3883,#3884,#3885));
#573=EDGE_LOOP('',(#3886,#3887,#3888,#3889,#3890,#3891,#3892,#3893));
#574=EDGE_LOOP('',(#3894));
#575=EDGE_LOOP('',(#3895,#3896,#3897,#3898,#3899));
#576=EDGE_LOOP('',(#3900,#3901,#3902,#3903,#3904,#3905,#3906));
#577=EDGE_LOOP('',(#3907,#3908));
#578=EDGE_LOOP('',(#3909));
#579=EDGE_LOOP('',(#3910));
#580=EDGE_LOOP('',(#3911,#3912,#3913,#3914,#3915,#3916,#3917,#3918));
#581=EDGE_LOOP('',(#3919,#3920,#3921,#3922,#3923));
#582=EDGE_LOOP('',(#3924,#3925,#3926,#3927));
#583=EDGE_LOOP('',(#3928));
#584=EDGE_LOOP('',(#3929,#3930,#3931,#3932));
#585=EDGE_LOOP('',(#3933,#3934,#3935,#3936));
#586=EDGE_LOOP('',(#3937));
#587=EDGE_LOOP('',(#3938,#3939,#3940,#3941,#3942));
#588=EDGE_LOOP('',(#3943));
#589=EDGE_LOOP('',(#3944,#3945,#3946,#3947));
#590=EDGE_LOOP('',(#3948));
#591=EDGE_LOOP('',(#3949));
#592=EDGE_LOOP('',(#3950));
#593=CIRCLE('',#4360,3.);
#594=CIRCLE('',#4361,3.);
#595=CIRCLE('',#4362,3.);
#596=CIRCLE('',#4364,0.5);
#597=CIRCLE('',#4366,3.5);
#598=CIRCLE('',#4367,24.7141941620437);
#599=CIRCLE('',#4368,9.);
#600=CIRCLE('',#4369,9.);
#601=CIRCLE('',#4370,4.445);
#602=CIRCLE('',#4373,9.);
#603=CIRCLE('',#4374,9.);
#604=CIRCLE('',#4375,24.7141941620437);
#605=CIRCLE('',#4376,3.5);
#606=CIRCLE('',#4377,4.445);
#607=CIRCLE('',#4379,0.5);
#608=CIRCLE('',#4388,4.445);
#609=CIRCLE('',#4389,4.445);
#610=CIRCLE('',#4392,3.99999999999999);
#611=CIRCLE('',#4393,3.99999999999999);
#612=CIRCLE('',#4396,4.00000000000001);
#613=CIRCLE('',#4397,4.00000000000001);
#614=CIRCLE('',#4400,4.00000000000001);
#615=CIRCLE('',#4401,4.00000000000001);
#616=CIRCLE('',#4404,4.00000000000001);
#617=CIRCLE('',#4405,4.00000000000001);
#618=CIRCLE('',#4407,6.99999999999999);
#619=CIRCLE('',#4408,6.99999999999999);
#620=CIRCLE('',#4410,9.9094315895918);
#621=CIRCLE('',#4411,9.9094315895918);
#622=CIRCLE('',#4413,5.);
#623=CIRCLE('',#4414,5.);
#624=CIRCLE('',#4417,5.99999999999999);
#625=CIRCLE('',#4418,5.99999999999999);
#626=CIRCLE('',#4421,5.99999999999999);
#627=CIRCLE('',#4422,5.99999999999999);
#628=CIRCLE('',#4425,7.);
#629=CIRCLE('',#4426,7.);
#630=CIRCLE('',#4432,3.22274999999998);
#631=CIRCLE('',#4449,5.);
#632=CIRCLE('',#4452,3.22274999999998);
#633=CIRCLE('',#4453,3.933);
#634=CIRCLE('',#4455,3.933);
#635=CIRCLE('',#4468,4.08499999999996);
#636=CIRCLE('',#4473,3.38975);
#637=CIRCLE('',#4478,3.38975);
#638=CIRCLE('',#4480,4.08499999999996);
#639=CIRCLE('',#4491,5.);
#640=CIRCLE('',#4492,5.);
#641=CIRCLE('',#4494,10.5388214764323);
#642=CIRCLE('',#4495,10.5388214764323);
#643=CIRCLE('',#4497,8.03882147643229);
#644=CIRCLE('',#4498,2.49999999999996);
#645=CIRCLE('',#4501,5.78096926885272);
#646=CIRCLE('',#4503,8.96120340959139);
#647=CIRCLE('',#4504,5.05765846207533);
#648=CIRCLE('',#4506,4.24999999999998);
#649=CIRCLE('',#4509,4.08499999999996);
#650=CIRCLE('',#4513,4.08499999999996);
#651=CIRCLE('',#4515,3.38975);
#652=CIRCLE('',#4519,3.38975);
#653=CIRCLE('',#4532,3.22274999999998);
#654=CIRCLE('',#4553,3.933);
#655=CIRCLE('',#4554,3.933);
#656=CIRCLE('',#4556,3.22274999999998);
#657=CIRCLE('',#4561,3.);
#658=CIRCLE('',#4562,3.);
#659=CIRCLE('',#4563,3.);
#660=CIRCLE('',#4565,0.5);
#661=CIRCLE('',#4567,9.);
#662=CIRCLE('',#4568,9.);
#663=CIRCLE('',#4569,24.7141941620437);
#664=CIRCLE('',#4570,3.5);
#665=CIRCLE('',#4571,4.445);
#666=CIRCLE('',#4574,3.5);
#667=CIRCLE('',#4575,24.7141941620437);
#668=CIRCLE('',#4576,9.);
#669=CIRCLE('',#4577,9.);
#670=CIRCLE('',#4578,4.445);
#671=CIRCLE('',#4580,0.5);
#672=CIRCLE('',#4589,4.445);
#673=CIRCLE('',#4590,4.445);
#674=CIRCLE('',#4593,3.99999999999999);
#675=CIRCLE('',#4594,3.99999999999999);
#676=CIRCLE('',#4597,4.00000000000001);
#677=CIRCLE('',#4598,4.00000000000001);
#678=CIRCLE('',#4601,4.00000000000001);
#679=CIRCLE('',#4602,4.00000000000001);
#680=CIRCLE('',#4605,4.00000000000001);
#681=CIRCLE('',#4606,4.00000000000001);
#682=CIRCLE('',#4608,6.99999999999999);
#683=CIRCLE('',#4609,6.99999999999999);
#684=CIRCLE('',#4611,9.9094315895918);
#685=CIRCLE('',#4612,9.9094315895918);
#686=CIRCLE('',#4614,5.);
#687=CIRCLE('',#4615,5.);
#688=CIRCLE('',#4618,5.99999999999999);
#689=CIRCLE('',#4619,5.99999999999999);
#690=CIRCLE('',#4622,5.99999999999999);
#691=CIRCLE('',#4623,5.99999999999999);
#692=CIRCLE('',#4626,7.);
#693=CIRCLE('',#4627,7.);
#694=CIRCLE('',#4633,5.);
#695=CIRCLE('',#4634,5.);
#696=CIRCLE('',#4636,5.);
#697=CIRCLE('',#4638,4.49999999999996);
#698=CIRCLE('',#4640,5.62967641351579);
#699=CIRCLE('',#4642,4.49999999999996);
#700=CIRCLE('',#4644,5.62967641351579);
#701=CIRCLE('',#4645,5.62967641351579);
#702=CIRCLE('',#4647,7.81234603703673);
#703=CIRCLE('',#4649,4.9623029756639);
#704=CIRCLE('',#4650,4.9623029756639);
#705=CIRCLE('',#4652,5.62967641351579);
#706=CIRCLE('',#4653,5.62967641351579);
#707=CIRCLE('',#4654,7.81234603703673);
#708=CIRCLE('',#4655,4.49999999999996);
#709=CIRCLE('',#4657,5.62967641351579);
#710=CIRCLE('',#4659,4.49999999999996);
#711=LINE('',#5537,#939);
#712=LINE('',#5541,#940);
#713=LINE('',#5545,#941);
#714=LINE('',#5549,#942);
#715=LINE('',#5551,#943);
#716=LINE('',#5553,#944);
#717=LINE('',#5556,#945);
#718=LINE('',#5559,#946);
#719=LINE('',#5561,#947);
#720=LINE('',#5569,#948);
#721=LINE('',#5572,#949);
#722=LINE('',#5577,#950);
#723=LINE('',#5578,#951);
#724=LINE('',#5583,#952);
#725=LINE('',#5590,#953);
#726=LINE('',#5596,#954);
#727=LINE('',#5598,#955);
#728=LINE('',#5599,#956);
#729=LINE('',#5601,#957);
#730=LINE('',#5603,#958);
#731=LINE('',#5605,#959);
#732=LINE('',#5608,#960);
#733=LINE('',#5611,#961);
#734=LINE('',#5612,#962);
#735=LINE('',#5617,#963);
#736=LINE('',#5622,#964);
#737=LINE('',#5624,#965);
#738=LINE('',#5626,#966);
#739=LINE('',#5627,#967);
#740=LINE('',#5632,#968);
#741=LINE('',#5636,#969);
#742=LINE('',#5638,#970);
#743=LINE('',#5639,#971);
#744=LINE('',#5644,#972);
#745=LINE('',#5648,#973);
#746=LINE('',#5650,#974);
#747=LINE('',#5651,#975);
#748=LINE('',#5656,#976);
#749=LINE('',#5660,#977);
#750=LINE('',#5662,#978);
#751=LINE('',#5663,#979);
#752=LINE('',#5672,#980);
#753=LINE('',#5675,#981);
#754=LINE('',#5683,#982);
#755=LINE('',#5687,#983);
#756=LINE('',#5689,#984);
#757=LINE('',#5690,#985);
#758=LINE('',#5695,#986);
#759=LINE('',#5699,#987);
#760=LINE('',#5701,#988);
#761=LINE('',#5702,#989);
#762=LINE('',#5707,#990);
#763=LINE('',#5711,#991);
#764=LINE('',#5713,#992);
#765=LINE('',#5714,#993);
#766=LINE('',#5719,#994);
#767=LINE('',#5722,#995);
#768=LINE('',#5723,#996);
#769=LINE('',#5730,#997);
#770=LINE('',#5862,#998);
#771=LINE('',#6296,#999);
#772=LINE('',#6706,#1000);
#773=LINE('',#7183,#1001);
#774=LINE('',#7718,#1002);
#775=LINE('',#8150,#1003);
#776=LINE('',#8599,#1004);
#777=LINE('',#9059,#1005);
#778=LINE('',#9518,#1006);
#779=LINE('',#9946,#1007);
#780=LINE('',#10389,#1008);
#781=LINE('',#10840,#1009);
#782=LINE('',#11296,#1010);
#783=LINE('',#11753,#1011);
#784=LINE('',#12292,#1012);
#785=LINE('',#12767,#1013);
#786=LINE('',#12776,#1014);
#787=LINE('',#12785,#1015);
#788=LINE('',#12794,#1016);
#789=LINE('',#12803,#1017);
#790=LINE('',#12812,#1018);
#791=LINE('',#12821,#1019);
#792=LINE('',#12828,#1020);
#793=LINE('',#12839,#1021);
#794=LINE('',#12848,#1022);
#795=LINE('',#12859,#1023);
#796=LINE('',#12870,#1024);
#797=LINE('',#12880,#1025);
#798=LINE('',#25104,#1026);
#799=LINE('',#25120,#1027);
#800=LINE('',#25341,#1028);
#801=LINE('',#25763,#1029);
#802=LINE('',#25836,#1030);
#803=LINE('',#26135,#1031);
#804=LINE('',#26483,#1032);
#805=LINE('',#26838,#1033);
#806=LINE('',#28049,#1034);
#807=LINE('',#28051,#1035);
#808=LINE('',#28053,#1036);
#809=LINE('',#28055,#1037);
#810=LINE('',#28057,#1038);
#811=LINE('',#28058,#1039);
#812=LINE('',#28061,#1040);
#813=LINE('',#28063,#1041);
#814=LINE('',#28064,#1042);
#815=LINE('',#28067,#1043);
#816=LINE('',#28068,#1044);
#817=LINE('',#28071,#1045);
#818=LINE('',#28072,#1046);
#819=LINE('',#28075,#1047);
#820=LINE('',#28076,#1048);
#821=LINE('',#28079,#1049);
#822=LINE('',#28080,#1050);
#823=LINE('',#28082,#1051);
#824=LINE('',#28089,#1052);
#825=LINE('',#28095,#1053);
#826=LINE('',#28115,#1054);
#827=LINE('',#28225,#1055);
#828=LINE('',#28597,#1056);
#829=LINE('',#29042,#1057);
#830=LINE('',#29322,#1058);
#831=LINE('',#29503,#1059);
#832=LINE('',#29856,#1060);
#833=LINE('',#30206,#1061);
#834=LINE('',#31864,#1062);
#835=LINE('',#31866,#1063);
#836=LINE('',#31868,#1064);
#837=LINE('',#31870,#1065);
#838=LINE('',#31872,#1066);
#839=LINE('',#31873,#1067);
#840=LINE('',#31876,#1068);
#841=LINE('',#31878,#1069);
#842=LINE('',#31879,#1070);
#843=LINE('',#31882,#1071);
#844=LINE('',#31883,#1072);
#845=LINE('',#31886,#1073);
#846=LINE('',#31887,#1074);
#847=LINE('',#31890,#1075);
#848=LINE('',#31891,#1076);
#849=LINE('',#31894,#1077);
#850=LINE('',#31895,#1078);
#851=LINE('',#31897,#1079);
#852=LINE('',#31903,#1080);
#853=LINE('',#32095,#1081);
#854=LINE('',#32527,#1082);
#855=LINE('',#32996,#1083);
#856=LINE('',#33439,#1084);
#857=LINE('',#33898,#1085);
#858=LINE('',#34349,#1086);
#859=LINE('',#34784,#1087);
#860=LINE('',#35231,#1088);
#861=LINE('',#35666,#1089);
#862=LINE('',#36109,#1090);
#863=LINE('',#36550,#1091);
#864=LINE('',#37013,#1092);
#865=LINE('',#37484,#1093);
#866=LINE('',#37927,#1094);
#867=LINE('',#38370,#1095);
#868=LINE('',#38837,#1096);
#869=LINE('',#39298,#1097);
#870=LINE('',#39737,#1098);
#871=LINE('',#40181,#1099);
#872=LINE('',#51257,#1100);
#873=LINE('',#51261,#1101);
#874=LINE('',#51265,#1102);
#875=LINE('',#51272,#1103);
#876=LINE('',#51276,#1104);
#877=LINE('',#51278,#1105);
#878=LINE('',#51279,#1106);
#879=LINE('',#51282,#1107);
#880=LINE('',#51286,#1108);
#881=LINE('',#51294,#1109);
#882=LINE('',#51295,#1110);
#883=LINE('',#51300,#1111);
#884=LINE('',#51301,#1112);
#885=LINE('',#51304,#1113);
#886=LINE('',#51312,#1114);
#887=LINE('',#51319,#1115);
#888=LINE('',#51321,#1116);
#889=LINE('',#51322,#1117);
#890=LINE('',#51324,#1118);
#891=LINE('',#51326,#1119);
#892=LINE('',#51328,#1120);
#893=LINE('',#51331,#1121);
#894=LINE('',#51334,#1122);
#895=LINE('',#51335,#1123);
#896=LINE('',#51340,#1124);
#897=LINE('',#51345,#1125);
#898=LINE('',#51347,#1126);
#899=LINE('',#51349,#1127);
#900=LINE('',#51350,#1128);
#901=LINE('',#51356,#1129);
#902=LINE('',#51359,#1130);
#903=LINE('',#51361,#1131);
#904=LINE('',#51362,#1132);
#905=LINE('',#51368,#1133);
#906=LINE('',#51371,#1134);
#907=LINE('',#51373,#1135);
#908=LINE('',#51374,#1136);
#909=LINE('',#51380,#1137);
#910=LINE('',#51383,#1138);
#911=LINE('',#51385,#1139);
#912=LINE('',#51386,#1140);
#913=LINE('',#51395,#1141);
#914=LINE('',#51398,#1142);
#915=LINE('',#51407,#1143);
#916=LINE('',#51410,#1144);
#917=LINE('',#51412,#1145);
#918=LINE('',#51413,#1146);
#919=LINE('',#51419,#1147);
#920=LINE('',#51422,#1148);
#921=LINE('',#51424,#1149);
#922=LINE('',#51425,#1150);
#923=LINE('',#51431,#1151);
#924=LINE('',#51434,#1152);
#925=LINE('',#51436,#1153);
#926=LINE('',#51437,#1154);
#927=LINE('',#51443,#1155);
#928=LINE('',#51445,#1156);
#929=LINE('',#51446,#1157);
#930=LINE('',#51453,#1158);
#931=LINE('',#51459,#1159);
#932=LINE('',#51460,#1160);
#933=LINE('',#51464,#1161);
#934=LINE('',#51490,#1162);
#935=LINE('',#51493,#1163);
#936=LINE('',#51504,#1164);
#937=LINE('',#51517,#1165);
#938=LINE('',#51523,#1166);
#939=VECTOR('',#4677,10.);
#940=VECTOR('',#4680,10.);
#941=VECTOR('',#4683,10.);
#942=VECTOR('',#4688,10.);
#943=VECTOR('',#4689,10.);
#944=VECTOR('',#4690,10.);
#945=VECTOR('',#4693,10.);
#946=VECTOR('',#4696,10.);
#947=VECTOR('',#4697,10.);
#948=VECTOR('',#4704,10.);
#949=VECTOR('',#4707,10.);
#950=VECTOR('',#4712,10.);
#951=VECTOR('',#4713,10.);
#952=VECTOR('',#4718,10.);
#953=VECTOR('',#4725,10.);
#954=VECTOR('',#4732,10.);
#955=VECTOR('',#4735,10.);
#956=VECTOR('',#4736,10.);
#957=VECTOR('',#4739,9.);
#958=VECTOR('',#4742,10.);
#959=VECTOR('',#4745,9.);
#960=VECTOR('',#4750,4.445);
#961=VECTOR('',#4753,10.);
#962=VECTOR('',#4754,10.);
#963=VECTOR('',#4759,4.445);
#964=VECTOR('',#4764,10.);
#965=VECTOR('',#4765,10.);
#966=VECTOR('',#4766,10.);
#967=VECTOR('',#4767,10.);
#968=VECTOR('',#4772,10.);
#969=VECTOR('',#4777,10.);
#970=VECTOR('',#4778,10.);
#971=VECTOR('',#4779,10.);
#972=VECTOR('',#4784,10.);
#973=VECTOR('',#4789,10.);
#974=VECTOR('',#4790,10.);
#975=VECTOR('',#4791,10.);
#976=VECTOR('',#4796,10.);
#977=VECTOR('',#4801,10.);
#978=VECTOR('',#4802,10.);
#979=VECTOR('',#4803,10.);
#980=VECTOR('',#4814,10.);
#981=VECTOR('',#4817,10.);
#982=VECTOR('',#4828,10.);
#983=VECTOR('',#4833,10.);
#984=VECTOR('',#4834,10.);
#985=VECTOR('',#4835,10.);
#986=VECTOR('',#4840,10.);
#987=VECTOR('',#4845,10.);
#988=VECTOR('',#4846,10.);
#989=VECTOR('',#4847,10.);
#990=VECTOR('',#4852,10.);
#991=VECTOR('',#4857,10.);
#992=VECTOR('',#4858,10.);
#993=VECTOR('',#4859,10.);
#994=VECTOR('',#4864,10.);
#995=VECTOR('',#4869,10.);
#996=VECTOR('',#4870,10.);
#997=VECTOR('',#4879,3.22274999999998);
#998=VECTOR('',#4884,3.22274999999998);
#999=VECTOR('',#4887,3.22274999999998);
#1000=VECTOR('',#4890,3.22274999999998);
#1001=VECTOR('',#4893,3.22274999999998);
#1002=VECTOR('',#4896,3.22274999999998);
#1003=VECTOR('',#4899,3.22274999999998);
#1004=VECTOR('',#4902,3.22274999999998);
#1005=VECTOR('',#4905,3.22274999999998);
#1006=VECTOR('',#4908,3.22274999999998);
#1007=VECTOR('',#4911,3.22274999999998);
#1008=VECTOR('',#4914,3.22274999999998);
#1009=VECTOR('',#4917,3.22274999999998);
#1010=VECTOR('',#4920,3.22274999999998);
#1011=VECTOR('',#4923,3.22274999999998);
#1012=VECTOR('',#4926,3.22274999999998);
#1013=VECTOR('',#4931,10.);
#1014=VECTOR('',#4932,10.);
#1015=VECTOR('',#4933,10.);
#1016=VECTOR('',#4934,10.);
#1017=VECTOR('',#4935,10.);
#1018=VECTOR('',#4936,10.);
#1019=VECTOR('',#4937,10.);
#1020=VECTOR('',#4938,10.);
#1021=VECTOR('',#4939,10.);
#1022=VECTOR('',#4940,10.);
#1023=VECTOR('',#4941,10.);
#1024=VECTOR('',#4942,10.);
#1025=VECTOR('',#4943,10.);
#1026=VECTOR('',#4980,4.08499999999997);
#1027=VECTOR('',#4985,4.08499999999997);
#1028=VECTOR('',#4988,4.08499999999997);
#1029=VECTOR('',#4991,4.08499999999997);
#1030=VECTOR('',#4994,3.38975);
#1031=VECTOR('',#4999,3.38975);
#1032=VECTOR('',#5002,3.38975);
#1033=VECTOR('',#5005,3.38975);
#1034=VECTOR('',#5016,10.);
#1035=VECTOR('',#5017,10.);
#1036=VECTOR('',#5018,10.);
#1037=VECTOR('',#5019,10.);
#1038=VECTOR('',#5020,10.);
#1039=VECTOR('',#5021,10.);
#1040=VECTOR('',#5024,10.);
#1041=VECTOR('',#5025,10.);
#1042=VECTOR('',#5026,10.);
#1043=VECTOR('',#5029,10.);
#1044=VECTOR('',#5030,10.);
#1045=VECTOR('',#5033,10.);
#1046=VECTOR('',#5034,10.);
#1047=VECTOR('',#5037,10.);
#1048=VECTOR('',#5038,10.);
#1049=VECTOR('',#5041,10.);
#1050=VECTOR('',#5042,10.);
#1051=VECTOR('',#5045,10.);
#1052=VECTOR('',#5054,5.);
#1053=VECTOR('',#5061,10.5388214764323);
#1054=VECTOR('',#5090,4.08499999999997);
#1055=VECTOR('',#5095,4.08499999999997);
#1056=VECTOR('',#5098,4.08499999999997);
#1057=VECTOR('',#5101,4.08499999999997);
#1058=VECTOR('',#5106,3.38975);
#1059=VECTOR('',#5111,3.38975);
#1060=VECTOR('',#5114,3.38975);
#1061=VECTOR('',#5117,3.38975);
#1062=VECTOR('',#5126,10.);
#1063=VECTOR('',#5127,10.);
#1064=VECTOR('',#5128,10.);
#1065=VECTOR('',#5129,10.);
#1066=VECTOR('',#5130,10.);
#1067=VECTOR('',#5131,10.);
#1068=VECTOR('',#5134,10.);
#1069=VECTOR('',#5135,10.);
#1070=VECTOR('',#5136,10.);
#1071=VECTOR('',#5139,10.);
#1072=VECTOR('',#5140,10.);
#1073=VECTOR('',#5143,10.);
#1074=VECTOR('',#5144,10.);
#1075=VECTOR('',#5147,10.);
#1076=VECTOR('',#5148,10.);
#1077=VECTOR('',#5151,10.);
#1078=VECTOR('',#5152,10.);
#1079=VECTOR('',#5155,10.);
#1080=VECTOR('',#5162,3.22274999999998);
#1081=VECTOR('',#5167,3.22274999999998);
#1082=VECTOR('',#5170,3.22274999999998);
#1083=VECTOR('',#5173,3.22274999999998);
#1084=VECTOR('',#5176,3.22274999999998);
#1085=VECTOR('',#5179,3.22274999999998);
#1086=VECTOR('',#5182,3.22274999999998);
#1087=VECTOR('',#5185,3.22274999999998);
#1088=VECTOR('',#5188,3.22274999999998);
#1089=VECTOR('',#5191,3.22274999999998);
#1090=VECTOR('',#5194,3.22274999999998);
#1091=VECTOR('',#5197,3.22274999999998);
#1092=VECTOR('',#5200,3.22274999999998);
#1093=VECTOR('',#5203,3.22274999999998);
#1094=VECTOR('',#5206,3.22274999999998);
#1095=VECTOR('',#5209,3.22274999999998);
#1096=VECTOR('',#5212,3.22274999999998);
#1097=VECTOR('',#5215,3.22274999999998);
#1098=VECTOR('',#5218,3.22274999999998);
#1099=VECTOR('',#5221,3.22274999999998);
#1100=VECTOR('',#5242,10.);
#1101=VECTOR('',#5245,10.);
#1102=VECTOR('',#5248,10.);
#1103=VECTOR('',#5251,10.);
#1104=VECTOR('',#5254,10.);
#1105=VECTOR('',#5255,10.);
#1106=VECTOR('',#5256,10.);
#1107=VECTOR('',#5259,10.);
#1108=VECTOR('',#5262,10.);
#1109=VECTOR('',#5269,10.);
#1110=VECTOR('',#5270,10.);
#1111=VECTOR('',#5275,10.);
#1112=VECTOR('',#5276,10.);
#1113=VECTOR('',#5279,10.);
#1114=VECTOR('',#5286,10.);
#1115=VECTOR('',#5295,10.);
#1116=VECTOR('',#5298,10.);
#1117=VECTOR('',#5299,10.);
#1118=VECTOR('',#5302,9.);
#1119=VECTOR('',#5305,10.);
#1120=VECTOR('',#5308,9.);
#1121=VECTOR('',#5313,4.445);
#1122=VECTOR('',#5316,10.);
#1123=VECTOR('',#5317,10.);
#1124=VECTOR('',#5322,4.445);
#1125=VECTOR('',#5327,10.);
#1126=VECTOR('',#5328,10.);
#1127=VECTOR('',#5329,10.);
#1128=VECTOR('',#5330,10.);
#1129=VECTOR('',#5337,10.);
#1130=VECTOR('',#5340,10.);
#1131=VECTOR('',#5341,10.);
#1132=VECTOR('',#5342,10.);
#1133=VECTOR('',#5349,10.);
#1134=VECTOR('',#5352,10.);
#1135=VECTOR('',#5353,10.);
#1136=VECTOR('',#5354,10.);
#1137=VECTOR('',#5361,10.);
#1138=VECTOR('',#5364,10.);
#1139=VECTOR('',#5365,10.);
#1140=VECTOR('',#5366,10.);
#1141=VECTOR('',#5377,10.);
#1142=VECTOR('',#5380,10.);
#1143=VECTOR('',#5393,10.);
#1144=VECTOR('',#5396,10.);
#1145=VECTOR('',#5397,10.);
#1146=VECTOR('',#5398,10.);
#1147=VECTOR('',#5405,10.);
#1148=VECTOR('',#5408,10.);
#1149=VECTOR('',#5409,10.);
#1150=VECTOR('',#5410,10.);
#1151=VECTOR('',#5417,10.);
#1152=VECTOR('',#5420,10.);
#1153=VECTOR('',#5421,10.);
#1154=VECTOR('',#5422,10.);
#1155=VECTOR('',#5429,10.);
#1156=VECTOR('',#5432,10.);
#1157=VECTOR('',#5433,10.);
#1158=VECTOR('',#5442,10.);
#1159=VECTOR('',#5447,10.);
#1160=VECTOR('',#5448,10.);
#1161=VECTOR('',#5453,5.);
#1162=VECTOR('',#5466,4.49999999999996);
#1163=VECTOR('',#5469,5.62967641351579);
#1164=VECTOR('',#5482,4.9623029756639);
#1165=VECTOR('',#5497,5.62967641351579);
#1166=VECTOR('',#5506,4.49999999999996);
#1167=B_SPLINE_CURVE_WITH_KNOTS('',3,(#5532,#5533,#5534,#5535),
 .UNSPECIFIED.,.F.,.F.,(4,4),(0.459706916456031,0.558076312618392),
 .UNSPECIFIED.);
#1168=B_SPLINE_CURVE_WITH_KNOTS('',3,(#5732,#5733,#5734,#5735,#5736,#5737,
#5738,#5739,#5740,#5741,#5742,#5743,#5744,#5745,#5746,#5747,#5748,#5749,
#5750,#5751,#5752,#5753,#5754,#5755,#5756,#5757,#5758,#5759,#5760,#5761,
#5762),.UNSPECIFIED.,.F.,.F.,(4,3,3,3,3,3,3,3,3,3,4),(135.088484104522,
135.183357452592,135.278085083771,135.37327950967,135.467774090023,135.562205452058,
135.656595638088,135.752356851307,135.846756258313,135.943198374639,136.039640490965),
 .UNSPECIFIED.);
#1169=B_SPLINE_CURVE_WITH_KNOTS('',3,(#5765,#5766,#5767,#5768,#5769,#5770,
#5771,#5772,#5773,#5774,#5775,#5776,#5777,#5778,#5779,#5780,#5781,#5782,
#5783,#5784,#5785,#5786,#5787,#5788,#5789,#5790,#5791,#5792,#5793,#5794,
#5795,#5796,#5797,#5798,#5799,#5800,#5801,#5802,#5803,#5804,#5805,#5806,
#5807,#5808,#5809,#5810,#5811,#5812,#5813,#5814,#5815,#5816,#5817,#5818,
#5819,#5820,#5821,#5822,#5823,#5824,#5825,#5826,#5827,#5828,#5829,#5830,
#5831,#5832,#5833,#5834,#5835,#5836,#5837,#5838,#5839,#5840,#5841,#5842,
#5843,#5844,#5845,#5846,#5847,#5848,#5849,#5850,#5851,#5852,#5853,#5854,
#5855,#5856,#5857,#5858),.UNSPECIFIED.,.F.,.F.,(4,2,2,2,2,2,2,2,2,2,2,2,
2,2,2,2,2,2,2,2,2,2,2,2,2,2,2,2,2,2,2,2,2,2,2,2,2,2,2,2,2,2,2,2,2,2,4),
(0.0057209449088494,0.103861911368512,0.131206262754794,0.138793528122716,
0.143482252567016,0.147782848695881,0.15330943057905,0.165272569137304,
0.237793745170985,0.29160869938094,0.297545267653851,0.300502332474027,
0.300522608840903,0.300543258027676,0.300564293317863,0.300585728630467,
0.300607578554829,0.300629858367842,0.300652584102735,0.300675772583853,
0.300699441476995,0.300723609353366,0.300748295753824,0.303095417880315,
0.30597791581334,0.311474715542388,0.34887979776667,0.401918797533959,0.431924592452901,
0.444711052939809,0.45474683107368,0.459923226535699,0.464135470813334,
0.468998551959832,0.477319251816791,0.512144776417391,0.51915990933343,
0.584122643035605,0.605243372488193,0.61769635853554,0.621638370754149,
0.624159844368455,0.626558058277041,0.629516330011378,0.636789063423376,
0.705917753616687,0.708678555662593),.UNSPECIFIED.);
#1170=B_SPLINE_CURVE_WITH_KNOTS('',3,(#5863,#5864,#5865,#5866,#5867,#5868,
#5869,#5870,#5871,#5872,#5873,#5874,#5875,#5876,#5877,#5878,#5879,#5880,
#5881,#5882,#5883,#5884,#5885,#5886,#5887,#5888,#5889,#5890,#5891,#5892,
#5893,#5894,#5895,#5896,#5897,#5898,#5899,#5900,#5901,#5902,#5903,#5904,
#5905,#5906,#5907,#5908,#5909,#5910,#5911,#5912,#5913,#5914,#5915,#5916,
#5917,#5918,#5919,#5920,#5921,#5922,#5923,#5924,#5925,#5926,#5927,#5928,
#5929,#5930,#5931,#5932,#5933,#5934,#5935,#5936,#5937,#5938,#5939,#5940,
#5941,#5942,#5943,#5944,#5945,#5946,#5947,#5948,#5949,#5950,#5951,#5952,
#5953,#5954,#5955,#5956,#5957,#5958,#5959,#5960,#5961,#5962,#5963,#5964,
#5965,#5966,#5967,#5968,#5969,#5970,#5971,#5972,#5973,#5974,#5975,#5976,
#5977,#5978,#5979,#5980,#5981,#5982,#5983,#5984,#5985,#5986,#5987,#5988,
#5989,#5990,#5991,#5992,#5993,#5994,#5995,#5996,#5997,#5998,#5999,#6000,
#6001,#6002,#6003,#6004,#6005,#6006,#6007,#6008,#6009,#6010,#6011,#6012,
#6013,#6014,#6015,#6016,#6017,#6018,#6019,#6020,#6021,#6022,#6023,#6024,
#6025,#6026,#6027,#6028,#6029,#6030,#6031,#6032,#6033,#6034,#6035,#6036,
#6037,#6038,#6039,#6040,#6041,#6042,#6043,#6044,#6045,#6046,#6047,#6048,
#6049,#6050,#6051,#6052,#6053,#6054,#6055,#6056,#6057,#6058,#6059,#6060,
#6061,#6062,#6063,#6064,#6065,#6066,#6067,#6068,#6069,#6070),
 .UNSPECIFIED.,.F.,.F.,(4,3,3,3,3,3,3,3,3,3,3,3,3,3,3,3,3,3,3,3,3,3,3,3,
3,3,3,3,3,3,3,3,3,3,3,3,3,3,3,3,3,3,3,3,3,3,3,3,3,3,3,3,3,3,3,3,3,3,3,3,
3,3,3,3,3,3,3,3,3,4),(128.80529879735,128.929991698112,129.054684598874,
129.147800779154,129.240791211017,129.333683471756,129.426508042657,129.519297567574,
129.612076820608,129.704870560763,129.797762815361,129.890706836103,129.983804530045,
130.052535440601,130.145654979342,130.238649150331,130.331545520457,130.424374733419,
130.517169225087,130.609953761454,130.702753093673,130.79565137859,130.888601682427,
130.981706002525,131.050386282328,131.143352725217,131.236193216463,131.328935523828,
131.421610721533,131.5142512722,131.606882118562,131.699528188761,131.792274812806,
131.885074106871,131.978030044583,132.048237124056,132.14151054607,132.23465782876,
132.327706349228,132.420685659563,132.513628936106,132.606560773306,132.699505749532,
132.792546233298,132.885637032366,132.978877645127,133.046087965783,133.139304490498,
133.232397384719,133.325394057745,133.418325495527,133.511223352139,133.60411225829,
133.697016830648,133.790021022654,133.883077764359,133.976288264225,134.043938807511,
134.136039163594,134.228013262994,134.319889832992,134.411703498339,134.503485161219,
134.595260602326,134.687055591602,134.778962943864,134.870927981932,134.963066833032,
135.041789649238,135.088484104361),.UNSPECIFIED.);
#1171=B_SPLINE_CURVE_WITH_KNOTS('',3,(#6071,#6072,#6073,#6074,#6075,#6076,
#6077,#6078,#6079,#6080,#6081,#6082,#6083,#6084,#6085,#6086,#6087,#6088,
#6089,#6090,#6091,#6092,#6093,#6094,#6095,#6096,#6097,#6098,#6099,#6100,
#6101,#6102,#6103,#6104,#6105,#6106,#6107,#6108,#6109,#6110,#6111,#6112,
#6113,#6114,#6115,#6116,#6117,#6118,#6119,#6120,#6121,#6122,#6123,#6124,
#6125,#6126,#6127,#6128,#6129,#6130,#6131,#6132,#6133,#6134,#6135,#6136,
#6137,#6138,#6139,#6140,#6141,#6142,#6143,#6144,#6145,#6146,#6147,#6148,
#6149,#6150,#6151,#6152,#6153,#6154,#6155,#6156,#6157,#6158,#6159,#6160,
#6161,#6162,#6163,#6164,#6165,#6166,#6167,#6168,#6169,#6170,#6171,#6172,
#6173,#6174,#6175,#6176,#6177,#6178,#6179,#6180,#6181,#6182,#6183,#6184,
#6185,#6186,#6187,#6188,#6189,#6190,#6191,#6192,#6193,#6194,#6195,#6196,
#6197,#6198,#6199,#6200,#6201,#6202,#6203,#6204,#6205,#6206,#6207,#6208,
#6209,#6210,#6211,#6212,#6213,#6214,#6215,#6216,#6217,#6218,#6219,#6220,
#6221,#6222,#6223,#6224,#6225,#6226,#6227,#6228,#6229,#6230,#6231,#6232,
#6233,#6234,#6235,#6236,#6237,#6238,#6239,#6240,#6241,#6242,#6243,#6244,
#6245,#6246,#6247,#6248,#6249,#6250,#6251,#6252,#6253,#6254,#6255,#6256,
#6257,#6258,#6259,#6260,#6261,#6262,#6263,#6264,#6265,#6266,#6267,#6268,
#6269,#6270,#6271,#6272,#6273,#6274,#6275,#6276,#6277,#6278,#6279,#6280,
#6281,#6282,#6283,#6284,#6285,#6286,#6287,#6288,#6289,#6290,#6291,#6292),
 .UNSPECIFIED.,.F.,.F.,(4,2,2,2,2,2,2,2,2,2,2,2,2,2,2,2,2,2,2,2,2,2,2,2,
2,2,2,2,2,2,2,2,2,2,2,2,2,2,2,2,2,2,2,2,2,2,2,2,2,2,2,2,2,2,2,2,2,2,2,2,
2,2,2,2,2,2,2,2,2,2,2,2,2,2,2,2,2,2,2,2,2,2,2,2,2,2,2,2,2,2,2,2,2,2,2,2,
2,2,2,2,2,2,2,2,2,2,2,2,2,2,4),(0.708678555662593,0.748782942643991,0.772922702532529,
0.780095352477205,0.784622173095557,0.788837082782898,0.794340571426341,
0.806601129882489,0.879417765593598,0.920425270664686,0.933095479641559,
0.941685625067459,0.94508716036817,0.947483975195023,0.949730252618617,
0.953555287368893,0.964101507653615,1.03042803317628,1.09240834791634,1.10151067405403,
1.10648471987993,1.11026484485518,1.1151165806436,1.12342447751245,1.15833689535541,
1.22663825629169,1.25999084264512,1.26525775098546,1.2680737677987,1.27043189604108,
1.27340843871699,1.2781448522497,1.30506424409905,1.33021297985093,1.36941582660573,
1.4143362359503,1.42235477472665,1.4275520376078,1.43174678235489,1.4365514636124,
1.4448924915533,1.48422852283635,1.52766876700422,1.57769265420215,1.5857982001687,
1.58890037360076,1.59112443660229,1.59355292734,1.59707265337207,1.60633841131265,
1.62034442202954,1.71955623966095,1.74030455069573,1.74736738309538,1.75188820093921,
1.75614231277469,1.76186267717969,1.77489705735033,1.7928118823639,1.8445755689971,
1.9001802182269,1.90821351613968,1.91130419222833,1.91352378887723,1.91595594649535,
1.91948892928184,1.92883239688369,1.94299463293385,2.04629108962734,2.06368208733208,
2.07028352174064,2.07426716567051,2.07852483246027,2.08424224073038,2.09723661782448,
2.11507613799312,2.16645374092106,2.22240976487947,2.2304379643149,2.23353035380687,
2.23575250962831,2.23818555558296,2.24172256417779,2.2510954368527,2.26531900898129,
2.31594572969656,2.37542367057146,2.3877449062705,2.39291475139969,2.39720189867906,
2.40150899436374,2.40776452549063,2.41492935379913,2.42792507971324,2.45870700168226,
2.52522355114272,2.54931724224462,2.55434447079601,2.55713212681062,2.55948361544353,
2.56247162777653,2.5686227413984,2.62051316394283,2.68786101994759,2.70728249431015,
2.71416416296146,2.718647805993,2.72264393838857,2.72680812058983,2.73206999633021,
2.73781577962203),.UNSPECIFIED.);
#1172=B_SPLINE_CURVE_WITH_KNOTS('',3,(#6297,#6298,#6299,#6300,#6301,#6302,
#6303,#6304,#6305,#6306,#6307,#6308,#6309,#6310,#6311,#6312,#6313,#6314,
#6315,#6316,#6317,#6318,#6319,#6320,#6321,#6322,#6323,#6324,#6325,#6326,
#6327,#6328,#6329,#6330,#6331,#6332,#6333,#6334,#6335,#6336,#6337,#6338,
#6339,#6340,#6341,#6342,#6343,#6344,#6345,#6346,#6347,#6348,#6349,#6350,
#6351,#6352,#6353,#6354,#6355,#6356,#6357,#6358,#6359,#6360,#6361,#6362,
#6363,#6364,#6365,#6366,#6367,#6368,#6369,#6370,#6371,#6372,#6373,#6374,
#6375,#6376,#6377,#6378,#6379,#6380,#6381,#6382,#6383,#6384,#6385,#6386,
#6387,#6388,#6389,#6390,#6391,#6392,#6393,#6394,#6395,#6396,#6397,#6398,
#6399,#6400,#6401,#6402,#6403,#6404,#6405,#6406,#6407,#6408,#6409,#6410,
#6411,#6412,#6413,#6414,#6415,#6416,#6417,#6418,#6419,#6420,#6421,#6422,
#6423,#6424,#6425,#6426,#6427,#6428,#6429,#6430,#6431,#6432,#6433,#6434,
#6435,#6436,#6437,#6438,#6439,#6440,#6441,#6442,#6443,#6444,#6445,#6446,
#6447,#6448,#6449,#6450,#6451,#6452,#6453,#6454,#6455,#6456,#6457,#6458,
#6459,#6460,#6461,#6462,#6463,#6464,#6465,#6466,#6467,#6468,#6469,#6470,
#6471,#6472,#6473,#6474,#6475,#6476,#6477,#6478,#6479,#6480,#6481,#6482,
#6483,#6484,#6485,#6486,#6487,#6488,#6489,#6490,#6491,#6492,#6493,#6494,
#6495,#6496,#6497,#6498,#6499,#6500,#6501,#6502,#6503,#6504),
 .UNSPECIFIED.,.F.,.F.,(4,3,3,3,3,3,3,3,3,3,3,3,3,3,3,3,3,3,3,3,3,3,3,3,
3,3,3,3,3,3,3,3,3,3,3,3,3,3,3,3,3,3,3,3,3,3,3,3,3,3,3,3,3,3,3,3,3,3,3,3,
3,3,3,3,3,3,3,3,3,4),(122.522113490002,122.617599580213,122.713164379506,
122.808908483514,122.904747907257,123.000792413016,123.067579548509,123.160674799028,
123.253644383959,123.346515905981,123.439319982668,123.532089169703,123.62484826403,
123.717622047648,123.810494779077,123.903419487396,123.99649841021,124.065430390237,
124.158526248507,124.251496449195,124.344368594077,124.43717330165,124.529943124285,
124.62270285815,124.715477284468,124.808350659465,124.901276012828,124.994355576363,
125.063281231964,125.156373615804,125.249340333502,125.342208991388,125.435010220104,
125.527776569966,125.62053284117,125.713303818973,125.806173788477,125.899095754988,
125.992171997024,126.061132073691,126.154229448072,126.247201144654,126.340074763607,
126.432880906914,126.525652141348,126.618413261588,126.711189047344,126.80406373209,
126.896990369618,126.990071162611,127.058982915419,127.152082698318,127.2450568592,
127.337932994276,127.430741720436,127.523515577764,127.616279357587,127.709057836291,
127.801935248434,127.894864636703,127.98794818957,128.056833757146,128.150391887151,
128.242254602021,128.334030345778,128.425745111084,128.520633532608,128.612328933846,
128.708813865514,128.805298797182),.UNSPECIFIED.);
#1173=B_SPLINE_CURVE_WITH_KNOTS('',3,(#6505,#6506,#6507,#6508,#6509,#6510,
#6511,#6512,#6513,#6514,#6515,#6516,#6517,#6518,#6519,#6520,#6521,#6522,
#6523,#6524,#6525,#6526,#6527,#6528,#6529,#6530,#6531,#6532,#6533,#6534,
#6535,#6536,#6537,#6538,#6539,#6540,#6541,#6542,#6543,#6544,#6545,#6546,
#6547,#6548,#6549,#6550,#6551,#6552,#6553,#6554,#6555,#6556,#6557,#6558,
#6559,#6560,#6561,#6562,#6563,#6564,#6565,#6566,#6567,#6568,#6569,#6570,
#6571,#6572,#6573,#6574,#6575,#6576,#6577,#6578,#6579,#6580,#6581,#6582,
#6583,#6584,#6585,#6586,#6587,#6588,#6589,#6590,#6591,#6592,#6593,#6594,
#6595,#6596,#6597,#6598,#6599,#6600,#6601,#6602,#6603,#6604,#6605,#6606,
#6607,#6608,#6609,#6610,#6611,#6612,#6613,#6614,#6615,#6616,#6617,#6618,
#6619,#6620,#6621,#6622,#6623,#6624,#6625,#6626,#6627,#6628,#6629,#6630,
#6631,#6632,#6633,#6634,#6635,#6636,#6637,#6638,#6639,#6640,#6641,#6642,
#6643,#6644,#6645,#6646,#6647,#6648,#6649,#6650,#6651,#6652,#6653,#6654,
#6655,#6656,#6657,#6658,#6659,#6660,#6661,#6662,#6663,#6664,#6665,#6666,
#6667,#6668,#6669,#6670,#6671,#6672,#6673,#6674,#6675,#6676,#6677,#6678,
#6679,#6680,#6681,#6682,#6683,#6684,#6685,#6686,#6687,#6688,#6689,#6690,
#6691,#6692,#6693,#6694,#6695,#6696,#6697,#6698,#6699,#6700,#6701,#6702),
 .UNSPECIFIED.,.F.,.F.,(4,2,2,2,2,2,2,2,2,2,2,2,2,2,2,2,2,2,2,2,2,2,2,2,
2,2,2,2,2,2,2,2,2,2,2,2,2,2,2,2,2,2,2,2,2,2,2,2,2,2,2,2,2,2,2,2,2,2,2,2,
2,2,2,2,2,2,2,2,2,2,2,2,2,2,2,2,2,2,2,2,2,2,2,2,2,2,2,2,2,2,2,2,2,2,2,2,
2,2,4),(0.00123641856443392,0.0677816156057305,0.128275151421882,0.137946939738651,
0.141528241670278,0.143970738293946,0.14618430044594,0.149243239419923,
0.157056842957665,0.218570542838502,0.279998979667933,0.290193460988853,
0.296257860872615,0.301545558887788,0.305639497662884,0.310133741016137,
0.317052529516095,0.336668786541449,0.437223046630292,0.451284103375782,
0.460580309110921,0.464107503933,0.466539726717936,0.468764759148168,0.4718672993043,
0.47996441925814,0.530841491770515,0.575776038492868,0.612972332189931,
0.62119311238409,0.625971368883615,0.630168539259352,0.635402123184994,
0.643540808168967,0.691935516511364,0.75647883328083,0.780328918877284,
0.785180678060024,0.787901045940586,0.790263163023318,0.793301829823471,
0.798361056364487,0.837991832148,0.893690639457914,0.921031188758042,0.933036913526042,
0.942580054022896,0.947640018094949,0.951419275461906,0.956181594110284,
0.9643290701301,0.995623213593347,1.07657046313531,1.10255582368811,1.10751815313142,
1.11026257949089,1.11262127136096,1.11567523096426,1.12067523167856,1.15504229037769,
1.20711992232119,1.25238046297746,1.26385821622653,1.2693020636188,1.2735217222203,
1.27817542647944,1.28582475963549,1.31167030776758,1.38073826029963,1.42406510506264,
1.42955817615089,1.43241513397301,1.4347656444174,1.43767859840649,1.44326654188307,
1.49039135801682,1.57456582415384,1.58624280399073,1.59172382345238,1.59594798814397,
1.60058232592772,1.60814419958438,1.6331784212617,1.7029498735112,1.74654194398789,
1.75203912186308,1.7548967987899,1.75724712215969,1.76015887297431,1.76574176004426,
1.80897166316429,1.89351458394855,1.90760243040227,1.9135061885,1.91779649706356,
1.92173660333723,1.9270749532319,1.94036234462692,2.03158365045162),
 .UNSPECIFIED.);
#1174=B_SPLINE_CURVE_WITH_KNOTS('',3,(#6707,#6708,#6709,#6710,#6711,#6712,
#6713,#6714,#6715,#6716,#6717,#6718,#6719,#6720,#6721,#6722,#6723,#6724,
#6725,#6726,#6727,#6728,#6729,#6730,#6731,#6732,#6733,#6734,#6735,#6736,
#6737,#6738,#6739,#6740,#6741,#6742,#6743,#6744,#6745,#6746,#6747,#6748,
#6749,#6750,#6751,#6752,#6753,#6754,#6755,#6756,#6757,#6758,#6759,#6760,
#6761,#6762,#6763,#6764,#6765,#6766,#6767,#6768,#6769,#6770,#6771,#6772,
#6773,#6774,#6775,#6776,#6777,#6778,#6779,#6780,#6781,#6782,#6783,#6784,
#6785,#6786,#6787,#6788,#6789,#6790,#6791,#6792,#6793,#6794,#6795,#6796,
#6797,#6798,#6799,#6800,#6801,#6802,#6803,#6804,#6805,#6806,#6807,#6808,
#6809,#6810,#6811,#6812,#6813,#6814,#6815,#6816,#6817,#6818,#6819,#6820,
#6821,#6822,#6823,#6824,#6825,#6826,#6827,#6828,#6829,#6830,#6831,#6832,
#6833,#6834,#6835,#6836,#6837,#6838,#6839,#6840,#6841,#6842,#6843,#6844,
#6845,#6846,#6847,#6848,#6849,#6850,#6851,#6852,#6853,#6854,#6855,#6856,
#6857,#6858,#6859,#6860,#6861,#6862,#6863,#6864,#6865,#6866,#6867,#6868,
#6869,#6870,#6871,#6872,#6873,#6874,#6875,#6876,#6877,#6878,#6879,#6880,
#6881,#6882,#6883,#6884,#6885,#6886,#6887,#6888,#6889,#6890,#6891,#6892,
#6893,#6894,#6895,#6896,#6897,#6898,#6899,#6900,#6901,#6902,#6903,#6904,
#6905,#6906,#6907,#6908,#6909,#6910,#6911,#6912,#6913,#6914,#6915,#6916,
#6917,#6918,#6919,#6920,#6921,#6922,#6923,#6924,#6925,#6926,#6927,#6928,
#6929,#6930,#6931,#6932,#6933,#6934,#6935,#6936,#6937,#6938,#6939,#6940,
#6941,#6942),.UNSPECIFIED.,.F.,.F.,(4,2,2,2,2,2,2,2,2,2,2,2,2,2,2,2,2,2,
2,2,2,2,2,2,2,2,2,2,2,2,2,2,2,2,2,2,2,2,2,2,2,2,2,2,2,2,2,2,2,2,2,2,2,2,
2,2,2,2,2,2,2,2,2,2,2,2,2,2,2,2,2,2,2,2,2,2,2,2,2,2,2,2,2,2,2,2,2,2,2,2,
2,2,2,2,2,2,2,2,2,2,2,2,2,2,2,2,2,2,2,2,2,2,2,2,2,2,2,4),(2.03108651980245,
2.05799265149469,2.12022779959758,2.13280091659172,2.13838566411232,2.14264032252365,
2.14718848448666,2.15435057938612,2.17804302546848,2.21953691392989,2.2851851115457,
2.29643757141376,2.3003626107332,2.30262921761593,2.30503146641448,2.30839460671581,
2.31663008999095,2.32858413587513,2.3655895006738,2.44383965386118,2.45567389466241,
2.46112605643676,2.46536013406124,2.46996631871562,2.47739489346602,2.5038223780982,
2.58643101373637,2.5939915804093,2.61693084811006,2.62189421505243,2.62466958514322,
2.62702560706743,2.63003853925066,2.63630514543607,2.6446735412035,2.66578274271971,
2.7305193536904,2.77138561500042,2.78002044516204,2.78494119648462,2.78871099010059,
2.79359435595854,2.80229571390002,2.8495413206444,2.89369677964559,2.93833062799393,
2.94391661959199,2.94682964123487,2.94918079590174,2.95203926479678,2.95753739424577,
3.00106613708808,3.07064583680315,3.09594198397455,3.10355172644917,3.1081975190175,
3.11242049617677,3.11788347674092,3.12945850297983,3.17547889411409,3.25358170137673,
3.26417671435543,3.26800972103492,3.27025823001799,3.27267261447915,3.27610347803792,
3.28476335177624,3.29754519120734,3.33908300070259,3.41064487986249,3.42296360826239,
3.42850329251727,3.43275070222199,3.43731755540097,3.44456568238514,3.46910560663978,
3.51299631491247,3.58034611516104,3.58781290348878,3.59081401570421,3.59301361805139,
3.59547465500316,3.59914113953224,3.60941127504253,3.62552207277897,3.69127031919621,
3.73844657849807,3.7472498644596,3.75224604997061,3.75633439896778,3.75647026840979,
3.7565914756702,3.7567004332773,3.75679903302306,3.75688878269824,3.75697090112621,
3.75704638582414,3.75711606218003,3.75718061986786,3.75724064024039,3.75729661724579,
3.75734897358605,3.75739807338706,3.75744423221015,3.7574877250313,3.76272154697002,
3.76857235197011,3.80273549208015,3.88986596894535,3.90764897091345,3.91229014690864,
3.91496522864601,3.91733787376142,3.92050902815266,3.92762182229513,3.95877841656303,
4.05167384684634,4.06186733040656),.UNSPECIFIED.);
#1175=B_SPLINE_CURVE_WITH_KNOTS('',3,(#6944,#6945,#6946,#6947,#6948,#6949,
#6950,#6951,#6952,#6953,#6954,#6955,#6956,#6957,#6958,#6959,#6960,#6961,
#6962,#6963,#6964,#6965,#6966,#6967,#6968,#6969,#6970,#6971,#6972,#6973,
#6974,#6975,#6976,#6977,#6978,#6979,#6980,#6981,#6982,#6983,#6984,#6985,
#6986,#6987,#6988,#6989,#6990,#6991,#6992,#6993,#6994,#6995,#6996,#6997,
#6998,#6999,#7000,#7001,#7002,#7003,#7004,#7005,#7006,#7007,#7008,#7009,
#7010,#7011,#7012,#7013,#7014,#7015,#7016,#7017,#7018,#7019,#7020,#7021,
#7022,#7023,#7024,#7025,#7026,#7027,#7028,#7029,#7030,#7031,#7032,#7033,
#7034,#7035,#7036,#7037,#7038,#7039,#7040,#7041,#7042,#7043,#7044,#7045,
#7046,#7047,#7048,#7049,#7050,#7051,#7052,#7053,#7054,#7055,#7056,#7057,
#7058,#7059,#7060,#7061,#7062,#7063,#7064,#7065,#7066,#7067,#7068,#7069,
#7070,#7071,#7072,#7073,#7074,#7075,#7076,#7077,#7078,#7079,#7080,#7081,
#7082,#7083,#7084,#7085,#7086,#7087,#7088,#7089,#7090,#7091,#7092,#7093,
#7094,#7095,#7096,#7097,#7098,#7099,#7100,#7101,#7102,#7103,#7104,#7105,
#7106,#7107,#7108,#7109,#7110,#7111,#7112,#7113,#7114,#7115,#7116,#7117,
#7118,#7119,#7120,#7121,#7122,#7123,#7124,#7125,#7126,#7127,#7128,#7129,
#7130,#7131,#7132,#7133,#7134,#7135,#7136,#7137,#7138,#7139,#7140,#7141,
#7142,#7143,#7144,#7145,#7146,#7147,#7148,#7149,#7150,#7151,#7152,#7153,
#7154,#7155,#7156,#7157,#7158,#7159,#7160,#7161,#7162,#7163,#7164,#7165,
#7166,#7167,#7168,#7169,#7170,#7171,#7172,#7173,#7174,#7175),
 .UNSPECIFIED.,.F.,.F.,(4,2,2,2,2,2,2,2,2,2,2,2,2,2,2,2,2,2,2,2,2,2,2,2,
2,2,2,2,2,2,2,2,2,2,2,2,2,2,2,2,2,2,2,2,2,2,2,2,2,2,2,2,2,2,2,2,2,2,2,2,
2,2,2,2,2,2,2,2,2,2,2,2,2,2,2,2,2,2,2,2,2,2,2,2,2,2,2,2,2,2,2,2,2,2,2,2,
2,2,2,2,2,2,2,2,2,2,2,2,2,2,2,2,2,2,2,4),(2.03158365045162,2.03183675089734,
2.06897030236158,2.07399098085856,2.07701850502147,2.07937954312591,2.082107541352,
2.08699405146832,2.11148236435685,2.16020461862623,2.22359754250598,2.23183653410937,
2.23710059476907,2.2413005264641,2.24605865805253,2.25418651919738,2.28984290371337,
2.33646636594381,2.3872900328422,2.39539640596704,2.39850011741762,2.40072545712093,
2.40315719251953,2.40668257234865,2.4159675873056,2.4300075298418,2.529914816234,
2.55011836158748,2.55711357394152,2.56162399496799,2.56589181759944,2.57166710887943,
2.58499216572997,2.60342550996571,2.65793042469855,2.70975742918681,2.71786190655743,
2.72096500311263,2.72318992883676,2.72562124732132,2.72914607433902,2.73842992547275,
2.75246836338354,2.85238251094338,2.87256207215379,2.87955341047536,2.88406246614374,
2.88832980652235,2.89410570493662,2.90743791101066,2.92588523826528,2.98047520506316,
2.98687273272193,2.99481874662263,3.03610760752572,3.04118537409018,3.04422889829452,
3.04659085343359,3.04930640850465,3.05413875698219,3.07765901654107,3.14017539615574,
3.19085513967979,3.19905005646943,3.20429960775176,3.2084966863313,3.21326095229262,
3.22142274467525,3.25767145160014,3.30594907640004,3.3276664585342,3.3382294314538,
3.35954925307577,3.36440701164568,3.36715706696493,3.36951370721529,3.3725560864371,
3.378983245884,3.38763078850444,3.40981333119848,3.47861236186263,3.49681523815673,
3.5170195076196,3.52401359453024,3.52852293837773,3.53278949060702,3.53856267218446,
3.55188108078516,3.57030396294056,3.62476447447846,3.67663637613913,3.68472341817868,
3.68782359383213,3.69004736014268,3.6924784999807,3.69565918182362,3.70382309162939,
3.71574036153947,3.7525734065989,3.8309973652987,3.8428000361503,3.84824369450076,
3.85247367225165,3.857077907669,3.86450890964671,3.89100794484308,3.93192639663793,
3.97074509242552,4.00307608630314,4.00800307102287,4.01103443792538,4.01338994254457,
4.0156162905569,4.01834914861004,4.02245881606929,4.06089890765304),
 .UNSPECIFIED.);
#1176=B_SPLINE_CURVE_WITH_KNOTS('',3,(#7176,#7177,#7178,#7179),
 .UNSPECIFIED.,.F.,.F.,(4,4),(0.00110109624755596,0.0013400475596189),
 .UNSPECIFIED.);
#1177=B_SPLINE_CURVE_WITH_KNOTS('',3,(#7185,#7186,#7187,#7188),
 .UNSPECIFIED.,.F.,.F.,(4,4),(4.06225937330911,4.06250570235455),
 .UNSPECIFIED.);
#1178=B_SPLINE_CURVE_WITH_KNOTS('',3,(#7189,#7190,#7191,#7192,#7193,#7194,
#7195,#7196,#7197,#7198,#7199,#7200,#7201,#7202,#7203,#7204,#7205,#7206,
#7207,#7208,#7209,#7210,#7211,#7212,#7213,#7214,#7215,#7216,#7217,#7218,
#7219,#7220,#7221,#7222,#7223,#7224,#7225,#7226,#7227,#7228,#7229,#7230,
#7231,#7232,#7233,#7234,#7235,#7236,#7237,#7238,#7239,#7240,#7241,#7242,
#7243,#7244,#7245,#7246,#7247,#7248,#7249,#7250,#7251,#7252,#7253,#7254,
#7255,#7256,#7257,#7258,#7259,#7260,#7261,#7262,#7263,#7264,#7265,#7266,
#7267,#7268,#7269,#7270,#7271,#7272,#7273,#7274,#7275,#7276,#7277,#7278,
#7279,#7280,#7281,#7282,#7283,#7284,#7285,#7286,#7287,#7288,#7289,#7290,
#7291,#7292,#7293,#7294,#7295,#7296,#7297,#7298,#7299,#7300,#7301,#7302,
#7303,#7304,#7305,#7306,#7307,#7308,#7309,#7310,#7311,#7312,#7313,#7314,
#7315,#7316,#7317,#7318,#7319,#7320,#7321,#7322,#7323,#7324,#7325,#7326,
#7327,#7328,#7329,#7330,#7331,#7332,#7333,#7334,#7335,#7336,#7337,#7338,
#7339,#7340,#7341,#7342,#7343,#7344,#7345,#7346,#7347,#7348,#7349,#7350,
#7351,#7352,#7353,#7354,#7355,#7356,#7357,#7358,#7359,#7360,#7361,#7362,
#7363,#7364,#7365,#7366,#7367,#7368,#7369,#7370,#7371,#7372,#7373,#7374,
#7375,#7376,#7377,#7378,#7379,#7380,#7381,#7382,#7383,#7384,#7385,#7386,
#7387,#7388,#7389,#7390,#7391,#7392,#7393,#7394,#7395,#7396,#7397,#7398,
#7399,#7400,#7401,#7402,#7403,#7404,#7405,#7406,#7407,#7408,#7409,#7410,
#7411,#7412,#7413,#7414,#7415,#7416,#7417,#7418,#7419,#7420,#7421,#7422,
#7423,#7424,#7425,#7426,#7427,#7428,#7429,#7430,#7431,#7432,#7433,#7434,
#7435,#7436,#7437,#7438,#7439,#7440,#7441,#7442,#7443,#7444,#7445,#7446,
#7447,#7448,#7449,#7450,#7451,#7452,#7453,#7454,#7455,#7456,#7457,#7458,
#7459,#7460,#7461,#7462,#7463,#7464,#7465,#7466,#7467,#7468,#7469,#7470,
#7471,#7472,#7473,#7474,#7475,#7476,#7477,#7478,#7479,#7480,#7481,#7482,
#7483,#7484,#7485,#7486,#7487,#7488,#7489,#7490,#7491,#7492,#7493,#7494,
#7495,#7496,#7497,#7498,#7499,#7500,#7501,#7502,#7503,#7504,#7505,#7506,
#7507,#7508),.UNSPECIFIED.,.F.,.F.,(4,2,2,2,2,2,2,2,2,2,2,2,2,2,2,2,2,2,
2,2,2,2,2,2,2,2,2,2,2,2,2,2,2,2,2,2,2,2,2,2,2,2,2,2,2,2,2,2,2,2,2,2,2,2,
2,2,2,2,2,2,2,2,2,2,2,2,2,2,2,2,2,2,2,2,2,2,2,2,2,2,2,2,2,2,2,2,2,2,2,2,
2,2,2,2,2,2,2,2,2,2,2,2,2,2,2,2,2,2,2,2,2,2,2,2,2,2,2,2,2,2,2,2,2,2,2,2,
2,2,2,2,2,2,2,2,2,2,2,2,2,2,2,2,2,2,2,2,2,2,2,2,2,2,2,2,2,2,2,2,2,4),(0.00111869507802623,
0.0346707320864722,0.0393382984862259,0.0423002843642449,0.0445921219449508,
0.0469465709571225,0.0497252332677127,0.0547067207279609,0.0779540567567848,
0.0848654127461771,0.123089164967028,0.155224727930418,0.192594780075219,
0.200825434674942,0.205605754085145,0.209802549278348,0.215032804565348,
0.223160794066955,0.271225141539507,0.350686734167333,0.358329923100332,
0.364112921647033,0.367019792324655,0.367028818940242,0.367037942371699,
0.367047163914033,0.367056484873357,0.367065906561771,0.367075430339832,
0.36708505756838,0.36709478960344,0.367104627870344,0.367114573800352,0.367124628862736,
0.367134794526613,0.367145072300748,0.367155463701468,0.367165970298893,
0.367176593658883,0.367187335374079,0.367198197055757,0.367209180388204,
0.367220287056655,0.367231518758393,0.367242877215067,0.367254364191546,
0.367265981493172,0.367277730952031,0.367289614413733,0.367301633790629,
0.367313790977865,0.367326087919605,0.367338526589154,0.367351108976622,
0.36736383714054,0.36737671318693,0.36738973918717,0.367402917310764,0.367416249730712,
0.367429738664116,0.36744338637168,0.367457195127561,0.367471167262364,
0.367485305143567,0.367499611167711,0.367514087747956,0.367528737394157,
0.367543562627308,0.367557153159669,0.36991900206317,0.372954787638147,
0.378004013932083,0.417071762226864,0.473206377051136,0.50062650535798,
0.512655777652281,0.522213721523594,0.527276812784424,0.531424624902641,
0.536320032952254,0.544847722221461,0.583626850929751,0.650048585915722,
0.681730061433135,0.686928400272485,0.689723324232265,0.692076617464239,
0.695061451147228,0.699830213431351,0.727586562803716,0.752413019782802,
0.792282613439576,0.821740748275609,0.834364180248572,0.84429308731521,
0.849432655190175,0.853623545945797,0.858471351220697,0.866788545467634,
0.901978768934724,0.970993838751653,1.00399173699691,1.00923479691719,1.01203929572447,
1.01439203743749,1.01736525159813,1.02209517036967,1.04891824059525,1.07430793646373,
1.10278572509421,1.15330356948103,1.16541989244579,1.1709823748974,1.1752180556021,
1.17925044980252,1.18610111681302,1.20521652883861,1.30640863378967,1.32049618328232,
1.32980574176163,1.33333525671414,1.33576822722659,1.33799340598454,1.34109524928743,
1.34918400312664,1.40218169951785,1.45590326279395,1.47419623269013,1.48744380736369,
1.49320718663859,1.49747434195323,1.5019915630707,1.50901280076575,1.52940562857986,
1.62906833330264,1.64309737918719,1.6523786206395,1.65590417520522,1.65833656065081,
1.66056291784519,1.66366864719864,1.67178442150596,1.72165332070677,1.7682260403789,
1.8048663784259,1.81305642912942,1.81782909927807,1.82202872607258,1.82727507081422,
1.83545247381546,1.88515648076462,1.94854753605004,1.97221739956403,1.9770605184349,
1.97977964637341,1.9821430659936,1.9851864548552,1.9902598483679,2.03084076488749,
2.03108651980245),.UNSPECIFIED.);
#1179=B_SPLINE_CURVE_WITH_KNOTS('',3,(#7509,#7510,#7511,#7512,#7513,#7514,
#7515,#7516,#7517,#7518,#7519,#7520,#7521,#7522,#7523,#7524,#7525,#7526,
#7527,#7528,#7529,#7530,#7531,#7532,#7533,#7534,#7535,#7536,#7537,#7538,
#7539,#7540,#7541,#7542,#7543,#7544,#7545,#7546,#7547,#7548,#7549,#7550,
#7551,#7552,#7553,#7554,#7555,#7556,#7557,#7558,#7559,#7560,#7561,#7562,
#7563,#7564,#7565,#7566,#7567,#7568,#7569,#7570,#7571,#7572,#7573,#7574,
#7575,#7576,#7577,#7578,#7579,#7580,#7581,#7582,#7583,#7584,#7585,#7586,
#7587,#7588,#7589,#7590,#7591,#7592,#7593,#7594,#7595,#7596,#7597,#7598,
#7599,#7600,#7601,#7602,#7603,#7604,#7605,#7606,#7607,#7608,#7609,#7610,
#7611,#7612,#7613,#7614,#7615,#7616,#7617,#7618,#7619,#7620,#7621,#7622,
#7623,#7624,#7625,#7626,#7627,#7628,#7629,#7630,#7631,#7632,#7633,#7634,
#7635,#7636,#7637,#7638,#7639,#7640,#7641,#7642,#7643,#7644,#7645,#7646,
#7647,#7648,#7649,#7650,#7651,#7652,#7653,#7654,#7655,#7656,#7657,#7658,
#7659,#7660,#7661,#7662,#7663,#7664,#7665,#7666,#7667,#7668,#7669,#7670,
#7671,#7672,#7673,#7674,#7675,#7676,#7677,#7678,#7679,#7680,#7681,#7682,
#7683,#7684,#7685,#7686,#7687,#7688,#7689,#7690,#7691,#7692,#7693,#7694,
#7695,#7696,#7697,#7698,#7699,#7700,#7701,#7702,#7703,#7704,#7705,#7706,
#7707,#7708,#7709,#7710,#7711,#7712,#7713,#7714),.UNSPECIFIED.,.F.,.F.,
(4,2,2,2,2,2,2,2,2,2,2,2,2,2,2,2,2,2,2,2,2,2,2,2,2,2,2,2,2,2,2,2,2,2,2,
2,2,2,2,2,2,2,2,2,2,2,2,2,2,2,2,2,2,2,2,2,2,2,2,2,2,2,2,2,2,2,2,2,2,2,2,
2,2,2,2,2,2,2,2,2,2,2,2,2,2,2,2,2,2,2,2,2,2,2,2,2,2,2,2,2,2,2,4),(0.0013400475596189,
0.062460897083141,0.0993597373398082,0.107562023802153,0.112335756122383,
0.116532677378207,0.121770846481562,0.129926168815735,0.178927808864556,
0.20875603014885,0.248554397764219,0.261024162353363,0.269427984894191,
0.272756873678616,0.275189824293852,0.277412762539173,0.280508564309726,
0.288560427938979,0.343586429761991,0.395796527808926,0.422985429972921,
0.430479913709594,0.435098769460633,0.439325828027745,0.444743085260552,
0.456397785439991,0.536240839669448,0.572159194354239,0.583900659867113,
0.592024996633251,0.595368797526696,0.597766652030345,0.600036913335066,
0.603984844683962,0.615414134880948,0.680888801237364,0.722347400740166,
0.746020502164547,0.753177811686764,0.757723098392572,0.761975171508534,
0.767556666693733,0.780123123268052,0.840208382040955,0.903866122695068,
0.913742610437099,0.917353044025897,0.919801444322793,0.922009171465023,
0.925046129469945,0.932730560407458,0.996397258520831,1.04268066625386,
1.06802203388068,1.07534570522573,1.07992716083896,1.08416572511621,1.08966202083245,
1.1017504281087,1.17690339063022,1.21585110749391,1.22816588786884,1.23658699804471,
1.23997879742136,1.24238498237208,1.24464169453353,1.2485212385943,1.2594583820186,
1.33706012708394,1.38311732862221,1.39469266572583,1.40015354195006,1.40437391343766,
1.40901584996815,1.41661700523665,1.4420338676837,1.51144022631826,1.55488841124938,
1.56038158430457,1.56323785579834,1.56558740120547,1.56849865824267,1.57408190781462,
1.61978096423188,1.6297108806708,1.67573076799502,1.71115724135569,1.71926906328463,
1.72402275606319,1.72822176151621,1.73348863542531,1.7417397581883,1.80268619993668,
1.87052589749619,1.8806562375186,1.88430201684389,1.88675762987702,1.88895891486739,
1.89197057409146,1.89958130078598,1.96534875952032,2.03091503449202,2.03102410849652),
 .UNSPECIFIED.);
#1180=B_SPLINE_CURVE_WITH_KNOTS('',3,(#7719,#7720,#7721,#7722,#7723,#7724,
#7725,#7726,#7727,#7728,#7729,#7730,#7731,#7732,#7733,#7734,#7735,#7736,
#7737,#7738,#7739,#7740,#7741,#7742,#7743,#7744,#7745,#7746,#7747,#7748,
#7749,#7750,#7751,#7752,#7753,#7754,#7755,#7756,#7757,#7758,#7759,#7760,
#7761,#7762,#7763,#7764,#7765,#7766,#7767,#7768,#7769,#7770,#7771,#7772,
#7773,#7774,#7775,#7776,#7777,#7778,#7779,#7780,#7781,#7782,#7783,#7784,
#7785,#7786,#7787,#7788,#7789,#7790,#7791,#7792,#7793,#7794,#7795,#7796,
#7797,#7798,#7799,#7800,#7801,#7802,#7803,#7804,#7805,#7806,#7807,#7808,
#7809,#7810,#7811,#7812,#7813,#7814,#7815,#7816,#7817,#7818,#7819,#7820,
#7821,#7822,#7823,#7824,#7825,#7826,#7827,#7828,#7829,#7830,#7831,#7832,
#7833,#7834,#7835,#7836,#7837,#7838,#7839,#7840,#7841,#7842,#7843,#7844,
#7845,#7846,#7847,#7848,#7849,#7850,#7851,#7852,#7853,#7854,#7855,#7856,
#7857,#7858,#7859,#7860,#7861,#7862,#7863,#7864,#7865,#7866,#7867,#7868,
#7869,#7870,#7871,#7872,#7873,#7874,#7875,#7876,#7877,#7878,#7879,#7880,
#7881,#7882,#7883,#7884,#7885,#7886,#7887,#7888,#7889,#7890,#7891,#7892,
#7893,#7894,#7895,#7896,#7897,#7898,#7899,#7900,#7901,#7902,#7903,#7904,
#7905,#7906,#7907,#7908,#7909,#7910,#7911,#7912,#7913,#7914,#7915,#7916,
#7917,#7918,#7919,#7920,#7921,#7922,#7923,#7924,#7925,#7926,#7927,#7928),
 .UNSPECIFIED.,.F.,.F.,(4,2,2,2,2,2,2,2,2,2,2,2,2,2,2,2,2,2,2,2,2,2,2,2,
2,2,2,2,2,2,2,2,2,2,2,2,2,2,2,2,2,2,2,2,2,2,2,2,2,2,2,2,2,2,2,2,2,2,2,2,
2,2,2,2,2,2,2,2,2,2,2,2,2,2,2,2,2,2,2,2,2,2,2,2,2,2,2,2,2,2,2,2,2,2,2,2,
2,2,2,2,2,2,2,2,4),(2.03190008286785,2.07977363910376,2.13446066374539,
2.144561461824,2.16431389066328,2.1690642552616,2.17179087983579,2.17391586994911,
2.17686909045172,2.18283405403035,2.19068941942356,2.27050931605199,2.31793496203556,
2.32604351323317,2.33126834329475,2.33546538521858,2.34025097474141,2.3485033876091,
2.3862363833622,2.43076221789267,2.48139102331639,2.48948748698368,2.49259008776981,
2.49481529832414,2.49724768520681,2.50077534327836,2.5100740521279,2.52414157736048,
2.62474370308302,2.64436841281063,2.65128847165212,2.65578306260333,2.66005946684776,
2.66588336640092,2.67949208349358,2.69844192487076,2.80384044773164,2.81209681550401,
2.81522004392104,2.81745068143635,2.81987815567379,2.8233807710882,2.83251193913524,
2.84623812506606,2.89351731596356,2.95736011873939,2.96866060178893,2.97479726756399,
2.9790879741144,2.98348658707277,2.98994844119316,3.00775850881061,3.03501376653203,
3.07685825613384,3.12637204719132,3.1344991864415,3.1376058197589,3.13983203173373,
3.14226331411159,3.14578571886053,3.15504964765729,3.16904624023057,3.26788304988401,
3.28897780356245,3.29608917532169,3.30062496082718,3.30488191909982,3.31058902757393,
3.32351849998876,3.34123900157135,3.4263046039849,3.43347946749547,3.45417033147242,
3.45898695644855,3.46172832064346,3.4640647828861,3.46711018335079,3.47354925991919,
3.48221649964425,3.50447087075489,3.58016178176387,3.60965873108932,3.61765844334337,
3.62238838501746,3.62617171075306,3.63127569604962,3.64103268665636,3.70524630603049,
3.77230139931496,3.77972756596522,3.78272101073167,3.78491813155336,3.78712378737464,
3.79039302266121,3.79843676072109,3.81020757208602,3.84627301351861,3.9259545786378,
3.93763389499367,3.94305624549346,3.94728460289099,3.95190217627877,3.9593885339276,
3.98647823277419,4.06225937330911),.UNSPECIFIED.);
#1181=B_SPLINE_CURVE_WITH_KNOTS('',3,(#7929,#7930,#7931,#7932,#7933,#7934,
#7935,#7936,#7937,#7938,#7939,#7940,#7941,#7942,#7943,#7944,#7945,#7946,
#7947,#7948,#7949,#7950,#7951,#7952,#7953,#7954,#7955,#7956,#7957,#7958,
#7959,#7960,#7961,#7962,#7963,#7964,#7965,#7966,#7967,#7968,#7969,#7970,
#7971,#7972,#7973,#7974,#7975,#7976,#7977,#7978,#7979,#7980,#7981,#7982,
#7983,#7984,#7985,#7986,#7987,#7988,#7989,#7990,#7991,#7992,#7993,#7994,
#7995,#7996,#7997,#7998,#7999,#8000,#8001,#8002,#8003,#8004,#8005,#8006,
#8007,#8008,#8009,#8010,#8011,#8012,#8013,#8014,#8015,#8016,#8017,#8018,
#8019,#8020,#8021,#8022,#8023,#8024,#8025,#8026,#8027,#8028,#8029,#8030,
#8031,#8032,#8033,#8034,#8035,#8036,#8037,#8038,#8039,#8040,#8041,#8042,
#8043,#8044,#8045,#8046,#8047,#8048,#8049,#8050,#8051,#8052,#8053,#8054,
#8055,#8056,#8057,#8058,#8059,#8060,#8061,#8062,#8063,#8064,#8065,#8066,
#8067,#8068,#8069,#8070,#8071,#8072,#8073,#8074,#8075,#8076,#8077,#8078,
#8079,#8080,#8081,#8082,#8083,#8084,#8085,#8086,#8087,#8088,#8089,#8090,
#8091,#8092,#8093,#8094,#8095,#8096,#8097,#8098,#8099,#8100,#8101,#8102,
#8103,#8104,#8105,#8106,#8107,#8108,#8109,#8110,#8111,#8112,#8113,#8114,
#8115,#8116,#8117,#8118,#8119,#8120,#8121,#8122,#8123,#8124,#8125,#8126,
#8127,#8128,#8129,#8130,#8131,#8132,#8133,#8134,#8135,#8136,#8137,#8138,
#8139,#8140,#8141,#8142,#8143,#8144,#8145,#8146),.UNSPECIFIED.,.F.,.F.,
(4,2,2,2,2,2,2,2,2,2,2,2,2,2,2,2,2,2,2,2,2,2,2,2,2,2,2,2,2,2,2,2,2,2,2,
2,2,2,2,2,2,2,2,2,2,2,2,2,2,2,2,2,2,2,2,2,2,2,2,2,2,2,2,2,2,2,2,2,2,2,2,
2,2,2,2,2,2,2,2,2,2,2,2,2,2,2,2,2,2,2,2,2,2,2,2,2,2,2,2,2,2,2,2,2,2,2,2,
2,4),(2.03102410849652,2.03956001958603,2.04494502964436,2.04915612514696,
2.05383829019968,2.06162328646331,2.0923457163036,2.15849044276081,2.19930894983273,
2.20438168325408,2.2074238021063,2.20978567501983,2.21250231315925,2.21733935844911,
2.24094137470707,2.30395272082228,2.35407602431123,2.36225920440289,2.36750529867725,
2.37170221323921,2.37646909037772,2.38464238161448,2.42107760980727,2.46988313640751,
2.49521368967327,2.52217724186554,2.52691123800625,2.52988497017717,2.53223670976782,
2.53503829881938,2.54027140563818,2.57301583289198,2.6418034164573,2.67744879076333,
2.68579250804491,2.69064489391482,2.69483323608056,2.69996144464477,2.70984222298223,
2.72238862327668,2.75158321810497,2.79167779618078,2.81589587792283,2.84427688193517,
2.84906914118907,2.85206028642371,2.85441290132757,2.85720030294585,2.86236722664191,
2.89322246417659,2.93703971901881,2.99842501694261,3.00664819113256,3.01190607744833,
3.01610358928176,3.02086166448348,3.02899613349939,3.0648067240458,3.11187343865224,
3.16202177648116,3.17011789054082,3.17321920968406,3.17544321365416,3.17787393490828,
3.18139857862447,3.19068586740167,3.20473294144917,3.30494861826134,3.32484325360536,
3.33179613451347,3.33629593100398,3.34056567539944,3.34636228058863,3.35982255192645,
3.37850464596329,3.47793378420726,3.49103774008786,3.49519952982131,3.49776699663231,
3.50017547725813,3.50358296369839,3.51210636104867,3.52462352413051,3.56469247098305,
3.5943776452994,3.64320785512963,3.65135655874794,3.65659181986569,3.66078730369643,
3.66556036427294,3.67333669735231,3.7025768799795,3.76442289533049,3.81059529882349,
3.81617716488816,3.81908779863048,3.8214368914524,3.82429266854063,3.82952495521428,
3.86264196085627,3.91453396581379,3.96533475118296,3.9735313397,3.9787811118797,
3.98297782358756,3.98774108898918,3.99269916895108,4.00019602089878,4.06019991115425),
 .UNSPECIFIED.);
#1182=B_SPLINE_CURVE_WITH_KNOTS('',3,(#8151,#8152,#8153,#8154,#8155,#8156,
#8157,#8158,#8159,#8160,#8161,#8162,#8163,#8164,#8165,#8166,#8167,#8168,
#8169,#8170,#8171,#8172,#8173,#8174,#8175,#8176,#8177,#8178,#8179,#8180,
#8181,#8182,#8183,#8184,#8185,#8186,#8187,#8188,#8189,#8190,#8191,#8192,
#8193,#8194,#8195,#8196,#8197,#8198,#8199,#8200,#8201,#8202,#8203,#8204,
#8205,#8206,#8207,#8208,#8209,#8210,#8211,#8212,#8213,#8214,#8215,#8216,
#8217,#8218,#8219,#8220,#8221,#8222,#8223,#8224,#8225,#8226,#8227,#8228,
#8229,#8230,#8231,#8232,#8233,#8234,#8235,#8236,#8237,#8238,#8239,#8240,
#8241,#8242,#8243,#8244,#8245,#8246,#8247,#8248,#8249,#8250,#8251,#8252,
#8253,#8254,#8255,#8256,#8257,#8258,#8259,#8260,#8261,#8262,#8263,#8264,
#8265,#8266,#8267,#8268,#8269,#8270,#8271,#8272,#8273,#8274,#8275,#8276,
#8277,#8278,#8279,#8280,#8281,#8282,#8283,#8284,#8285,#8286,#8287,#8288,
#8289,#8290,#8291,#8292,#8293,#8294,#8295,#8296,#8297,#8298,#8299,#8300,
#8301,#8302,#8303,#8304,#8305,#8306,#8307,#8308,#8309,#8310,#8311,#8312,
#8313,#8314,#8315,#8316,#8317,#8318,#8319,#8320,#8321,#8322,#8323,#8324,
#8325,#8326,#8327,#8328,#8329,#8330,#8331,#8332,#8333,#8334,#8335,#8336,
#8337,#8338,#8339,#8340,#8341,#8342,#8343,#8344,#8345,#8346,#8347,#8348,
#8349,#8350,#8351,#8352,#8353,#8354,#8355,#8356,#8357,#8358,#8359,#8360,
#8361,#8362,#8363,#8364,#8365,#8366,#8367,#8368,#8369,#8370),
 .UNSPECIFIED.,.F.,.F.,(4,2,2,2,2,2,2,2,2,2,2,2,2,2,2,2,2,2,2,2,2,2,2,2,
2,2,2,2,2,2,2,2,2,2,2,2,2,2,2,2,2,2,2,2,2,2,2,2,2,2,2,2,2,2,2,2,2,2,2,2,
2,2,2,2,2,2,2,2,2,2,2,2,2,2,2,2,2,2,2,2,2,2,2,2,2,2,2,2,2,2,2,2,2,2,2,2,
2,2,2,2,2,2,2,2,2,2,2,2,2,4),(0.00130988952596835,0.0573674019543287,0.0650598693452133,
0.070099528425691,0.0749205816804568,0.0791131909454157,0.0842866522297215,
0.0922281214241368,0.135080471076808,0.169959837947393,0.222962547915876,
0.231969975323028,0.235498218217464,0.237930400164034,0.240154928260367,
0.243255956739319,0.251343268609958,0.304289159884606,0.311753615946756,
0.359968175821831,0.377181560599029,0.389738872619975,0.395230142819384,
0.399504920928421,0.404002469072135,0.410936548051482,0.430668585815097,
0.531087240987262,0.545143147082112,0.554436804479322,0.557963568358079,
0.560395678679199,0.562620897863997,0.565723880097549,0.573823682389663,
0.62625816110239,0.680372592547324,0.698736546604477,0.712022760612445,
0.717792138967529,0.722059680352674,0.726573572468589,0.733581938031989,
0.753880900196495,0.853633052030626,0.867663827799383,0.876945472320145,
0.880470693852264,0.88290269550838,0.885128577912581,0.8882334838035,0.896345874885187,
0.946250153616599,0.993570979887993,1.02948690398614,1.03763186603329,1.04239416831188,
1.04659425747777,1.05185385447603,1.06007667833684,1.12140113878597,1.17501470565662,
1.18966304777984,1.19924408653291,1.20281317138764,1.2052538702163,1.20747067408061,
1.21054081957405,1.21841899930135,1.27877304694429,1.32727236713757,1.34454583447853,
1.35722390976516,1.36288755631765,1.36713843368776,1.37113991173009,1.37782836943332,
1.39579746872806,1.49841056385381,1.51255130733836,1.521886918665,1.52542037745119,
1.52785419710441,1.5300786626776,1.53317756424001,1.54124444626687,1.59598467826236,
1.6484309151698,1.67569421819001,1.68319782892231,1.6878201898786,1.69204906363819,
1.69746673126553,1.70911472469393,1.78909679388562,1.83987945120788,1.84586310434081,
1.84882021507066,1.85094578598968,1.85367005151241,1.85840946591991,1.87800963932858,
1.88828271382747,1.97181547965497,1.99837075662635,2.0058105219466,2.01041879466552,
2.01465155583869,2.02009751099426,2.03190008286785),.UNSPECIFIED.);
#1183=B_SPLINE_CURVE_WITH_KNOTS('',3,(#8372,#8373,#8374,#8375),
 .UNSPECIFIED.,.F.,.F.,(4,4),(4.06019991115425,4.06049199751014),
 .UNSPECIFIED.);
#1184=B_SPLINE_CURVE_WITH_KNOTS('',3,(#8376,#8377,#8378,#8379,#8380,#8381,
#8382,#8383,#8384,#8385,#8386,#8387,#8388,#8389,#8390,#8391,#8392,#8393,
#8394,#8395,#8396,#8397,#8398,#8399,#8400,#8401,#8402,#8403,#8404,#8405,
#8406,#8407,#8408,#8409,#8410,#8411,#8412,#8413,#8414,#8415,#8416,#8417,
#8418,#8419,#8420,#8421,#8422,#8423,#8424,#8425,#8426,#8427,#8428,#8429,
#8430,#8431,#8432,#8433,#8434,#8435,#8436,#8437,#8438,#8439,#8440,#8441,
#8442,#8443,#8444,#8445,#8446,#8447,#8448,#8449,#8450,#8451,#8452,#8453,
#8454,#8455,#8456,#8457,#8458,#8459,#8460,#8461,#8462,#8463,#8464,#8465,
#8466,#8467,#8468,#8469,#8470,#8471,#8472,#8473,#8474,#8475,#8476,#8477,
#8478,#8479,#8480,#8481,#8482,#8483,#8484,#8485,#8486,#8487,#8488,#8489,
#8490,#8491,#8492,#8493,#8494,#8495,#8496,#8497,#8498,#8499,#8500,#8501,
#8502,#8503,#8504,#8505,#8506,#8507,#8508,#8509,#8510,#8511,#8512,#8513,
#8514,#8515,#8516,#8517,#8518,#8519,#8520,#8521,#8522,#8523,#8524,#8525,
#8526,#8527,#8528,#8529,#8530,#8531,#8532,#8533,#8534,#8535,#8536,#8537,
#8538,#8539,#8540,#8541,#8542,#8543,#8544,#8545,#8546,#8547,#8548,#8549,
#8550,#8551,#8552,#8553,#8554,#8555,#8556,#8557,#8558,#8559,#8560,#8561,
#8562,#8563,#8564,#8565,#8566,#8567,#8568,#8569,#8570,#8571,#8572,#8573,
#8574,#8575,#8576,#8577,#8578,#8579,#8580,#8581,#8582,#8583,#8584,#8585,
#8586,#8587,#8588,#8589,#8590,#8591,#8592,#8593,#8594,#8595),
 .UNSPECIFIED.,.F.,.F.,(4,2,2,2,2,2,2,2,2,2,2,2,2,2,2,2,2,2,2,2,2,2,2,2,
2,2,2,2,2,2,2,2,2,2,2,2,2,2,2,2,2,2,2,2,2,2,2,2,2,2,2,2,2,2,2,2,2,2,2,2,
2,2,2,2,2,2,2,2,2,2,2,2,2,2,2,2,2,2,2,2,2,2,2,2,2,2,2,2,2,2,2,2,2,2,2,2,
2,2,2,2,2,2,2,2,2,2,2,2,2,4),(0.000994439833694746,0.0659502631595153,0.0733296487053945,
0.0773660603147175,0.080891760506465,0.0833233080423989,0.0855481362709591,
0.0886507210913307,0.0967505802559279,0.14792612363284,0.18619872495472,
0.228442905746919,0.237113053470544,0.241218972857156,0.245439703015733,
0.250084169382157,0.257694363837813,0.28318741069681,0.366143308611974,
0.396385679007049,0.401659909442459,0.404470730843828,0.406822660667148,
0.40978709472243,0.414488742025188,0.440878130615305,0.526769176470696,
0.553630067711241,0.561095538639456,0.565708227825213,0.569937403213718,
0.575368125474658,0.587094867669498,0.666242590443618,0.702604141897903,
0.714431981881784,0.72260148295881,0.725952799465748,0.728352049571391,
0.730620321913657,0.73455775775061,0.745909229444491,0.811475512277769,
0.852945551138045,0.876623294234471,0.883781357468483,0.888326981503506,
0.892579271878954,0.898160909614941,0.910727063761941,0.970583230225985,
1.0209508256157,1.03513934063388,1.04449712275035,1.04803282886827,1.0504662620616,
1.05268882218408,1.05578302789872,1.06382323123028,1.11975718681435,1.17130842716486,
1.18918744312778,1.20220397536833,1.20792586619817,1.21218478301565,1.21671418513933,
1.22379782664218,1.24467792128572,1.34371676738214,1.35771710571413,1.36698330342056,
1.37050568046181,1.37293667390736,1.37516238360264,1.37826801694417,1.38638972937924,
1.43606074743629,1.44709540424683,1.49506885089472,1.52096100607504,1.52833787513419,
1.53293147103154,1.53716703446471,1.54263940599612,1.55459241529065,1.63144074207897,
1.66927999831409,1.68138986810137,1.68970583154832,1.69308111037679,1.69548468895388,
1.69774647544496,1.70165041605265,1.71275824843856,1.77854845336969,1.82008939109822,
1.84379349825791,1.85095468750353,1.85550124382183,1.8597536741489,1.8653344336001,
1.87789397151222,1.94029182340544,2.00184670814057,2.01158899706795,2.01518070129991,
2.0176255280612,2.01983717678426,2.02288870598913,2.03065902089388),
 .UNSPECIFIED.);
#1185=B_SPLINE_CURVE_WITH_KNOTS('',3,(#8601,#8602,#8603,#8604,#8605,#8606,
#8607,#8608,#8609,#8610,#8611,#8612,#8613,#8614,#8615,#8616,#8617,#8618,
#8619,#8620,#8621,#8622,#8623,#8624,#8625,#8626,#8627,#8628,#8629,#8630,
#8631,#8632,#8633,#8634,#8635,#8636,#8637,#8638,#8639,#8640,#8641,#8642,
#8643,#8644,#8645,#8646,#8647,#8648,#8649,#8650,#8651,#8652,#8653,#8654,
#8655,#8656,#8657,#8658,#8659,#8660,#8661,#8662,#8663,#8664,#8665,#8666,
#8667,#8668,#8669,#8670,#8671,#8672,#8673,#8674,#8675,#8676,#8677,#8678,
#8679,#8680,#8681,#8682,#8683,#8684,#8685,#8686,#8687,#8688,#8689,#8690,
#8691,#8692,#8693,#8694,#8695,#8696,#8697,#8698,#8699,#8700,#8701,#8702,
#8703,#8704,#8705,#8706,#8707,#8708,#8709,#8710,#8711,#8712,#8713,#8714,
#8715,#8716,#8717,#8718,#8719,#8720,#8721,#8722,#8723,#8724,#8725,#8726,
#8727,#8728,#8729,#8730,#8731,#8732,#8733,#8734,#8735,#8736,#8737,#8738,
#8739,#8740,#8741,#8742,#8743,#8744,#8745,#8746,#8747,#8748,#8749,#8750,
#8751,#8752,#8753,#8754,#8755,#8756,#8757,#8758,#8759,#8760,#8761,#8762,
#8763,#8764,#8765,#8766,#8767,#8768,#8769,#8770,#8771,#8772,#8773,#8774,
#8775,#8776,#8777,#8778,#8779,#8780,#8781,#8782,#8783,#8784,#8785,#8786,
#8787,#8788,#8789,#8790,#8791,#8792,#8793,#8794,#8795,#8796,#8797,#8798,
#8799,#8800,#8801,#8802,#8803,#8804,#8805,#8806,#8807,#8808,#8809,#8810,
#8811,#8812,#8813,#8814,#8815,#8816,#8817,#8818,#8819,#8820,#8821,#8822,
#8823,#8824),.UNSPECIFIED.,.F.,.F.,(4,2,2,2,2,2,2,2,2,2,2,2,2,2,2,2,2,2,
2,2,2,2,2,2,2,2,2,2,2,2,2,2,2,2,2,2,2,2,2,2,2,2,2,2,2,2,2,2,2,2,2,2,2,2,
2,2,2,2,2,2,2,2,2,2,2,2,2,2,2,2,2,2,2,2,2,2,2,2,2,2,2,2,2,2,2,2,2,2,2,2,
2,2,2,2,2,2,2,2,2,2,2,2,2,2,2,2,2,2,2,2,2,4),(2.03118787455235,2.03624725675821,
2.03928615281083,2.04164853071416,2.04436928762826,2.04922203066296,2.07308122157576,
2.1376664293898,2.1860662189869,2.19420566582604,2.1994396559146,2.20363713626479,
2.20841573420626,2.21663710656503,2.25384133694866,2.29873065790328,2.34957053914338,
2.35766596939636,2.36076826798253,2.36299328522015,2.36542548806491,2.36895292457676,
2.37825131015617,2.3923185751308,2.4929351512513,2.51253956156871,2.51945658846259,
2.52395028502474,2.52822661672449,2.53405164456053,2.54766874288209,2.56663442277931,
2.6654652165202,2.67869098458684,2.68286875689106,2.68544063857928,2.68784886625183,
2.69124968209712,2.69972422074796,2.71214367071196,2.75165759357714,2.78169765236756,
2.83093151813495,2.83909495281487,2.84433614742495,2.84853412694834,2.85330759423796,
2.86150575398539,2.89831852066463,2.94536845441438,2.94793593314125,2.96969841540064,
2.97745146849416,2.99952343365957,3.00443316892829,3.00719573006907,3.00955203211667,
3.01257972026627,3.01892636700058,3.02743356966184,3.04907330692725,3.11639516208406,
3.15411539810479,3.16258719939068,3.1674698811342,3.17165829725855,3.1767539905184,
3.18647004198533,3.24946051795983,3.31791938087541,3.3252741972512,3.32825539195769,
3.33066760118873,3.33318565277603,3.33711947277431,3.34952430452682,3.37054977835078,
3.43481817839165,3.47616765338134,3.48406044143621,3.48921905771577,3.49341079467507,
3.49824322712112,3.50671384163061,3.54862803699206,3.60750270921351,3.60961678988223,
3.6433254055801,3.64830047924921,3.651346915815,3.65370476216334,3.65645397276523,
3.66143906965294,3.68758516587915,3.77031735367454,3.79991793479009,3.80792562488444,
3.81265713522846,3.81643997556057,3.82044939222957,3.82809058534521,3.86040976074722,
3.90639870016087,3.96162577993268,3.96966331704312,3.97275722226204,3.97497979798098,
3.97741350831253,3.98095009110326,3.98500250769485,3.99242424884924,4.06083257184693),
 .UNSPECIFIED.);
#1186=B_SPLINE_CURVE_WITH_KNOTS('',3,(#8825,#8826,#8827,#8828),
 .UNSPECIFIED.,.F.,.F.,(4,4),(0.00101359709204687,0.00130988952596835),
 .UNSPECIFIED.);
#1187=B_SPLINE_CURVE_WITH_KNOTS('',3,(#8830,#8831,#8832,#8833,#8834,#8835,
#8836,#8837,#8838,#8839,#8840,#8841,#8842,#8843,#8844,#8845,#8846,#8847,
#8848,#8849,#8850,#8851,#8852,#8853,#8854,#8855,#8856,#8857,#8858,#8859,
#8860,#8861,#8862,#8863,#8864,#8865,#8866,#8867,#8868,#8869,#8870,#8871,
#8872,#8873,#8874,#8875,#8876,#8877,#8878,#8879,#8880,#8881,#8882,#8883,
#8884,#8885,#8886,#8887,#8888,#8889,#8890,#8891,#8892,#8893,#8894,#8895,
#8896,#8897,#8898,#8899,#8900,#8901,#8902,#8903,#8904,#8905,#8906,#8907,
#8908,#8909,#8910,#8911,#8912,#8913,#8914,#8915,#8916,#8917,#8918,#8919,
#8920,#8921,#8922,#8923,#8924,#8925,#8926,#8927,#8928,#8929,#8930,#8931,
#8932,#8933,#8934,#8935,#8936,#8937,#8938,#8939,#8940,#8941,#8942,#8943,
#8944,#8945,#8946,#8947,#8948,#8949,#8950,#8951,#8952,#8953,#8954,#8955,
#8956,#8957,#8958,#8959,#8960,#8961,#8962,#8963,#8964,#8965,#8966,#8967,
#8968,#8969,#8970,#8971,#8972,#8973,#8974,#8975,#8976,#8977,#8978,#8979,
#8980,#8981,#8982,#8983,#8984,#8985,#8986,#8987,#8988,#8989,#8990,#8991,
#8992,#8993,#8994,#8995,#8996,#8997,#8998,#8999,#9000,#9001,#9002,#9003,
#9004,#9005,#9006,#9007,#9008,#9009,#9010,#9011,#9012,#9013,#9014,#9015,
#9016,#9017,#9018,#9019,#9020,#9021,#9022,#9023,#9024,#9025,#9026,#9027,
#9028,#9029,#9030,#9031,#9032,#9033,#9034,#9035,#9036,#9037,#9038,#9039,
#9040,#9041,#9042,#9043,#9044,#9045,#9046,#9047,#9048,#9049,#9050,#9051),
 .UNSPECIFIED.,.F.,.F.,(4,2,2,2,2,2,2,2,2,2,2,2,2,2,2,2,2,2,2,2,2,2,2,2,
2,2,2,2,2,2,2,2,2,2,2,2,2,2,2,2,2,2,2,2,2,2,2,2,2,2,2,2,2,2,2,2,2,2,2,2,
2,2,2,2,2,2,2,2,2,2,2,2,2,2,2,2,2,2,2,2,2,2,2,2,2,2,2,2,2,2,2,2,2,2,2,2,
2,2,2,2,2,2,2,2,2,2,2,2,2,2,4),(2.03065902089388,2.04206362365894,2.07628240140505,
2.15899822527557,2.17032810560539,2.17574318636432,2.17995849926214,2.18462565439367,
2.19233952964678,2.22213609654879,2.28127762630686,2.33021015762429,2.33526795804928,
2.33830600785598,2.34066778836801,2.34338790739053,2.34823960975793,2.37209527496487,
2.4366731149445,2.4850667005546,2.49320447884936,2.49843728182706,2.50263372953709,
2.50741105888515,2.51562999543571,2.55281679747204,2.59770897459972,2.64854814924202,
2.65664218822806,2.65974380451698,2.6619682934422,2.66439986128824,2.66792625884059,
2.67722119348805,2.69128248530843,2.7917870906739,2.81147141139176,2.81839794470002,
2.82289293970401,2.82716697410541,2.83298330238232,2.84655397545899,2.86543597981326,
2.9691715943992,2.97870275544258,2.98237447516457,2.98459091913283,2.98703010138349,
2.99059507906017,3.00015361392844,3.01475878370679,3.06806380130599,3.12973866491161,
3.13799011728958,3.14325723122961,3.14745647678121,3.15221049273746,3.16032300839317,
3.19575837993672,3.24180305128279,3.2560282901354,3.29735870700056,3.30292438171499,
3.30583191437005,3.30818149028723,3.31104148642996,3.31655228514208,3.3610509220796,
3.4332378307528,3.45555781694311,3.46281282118754,3.46737914811334,3.47162272960065,
3.47724880029418,3.48972470070686,3.50664127262168,3.55344089936151,3.61625648081801,
3.623977499376,3.62702041337682,3.62922953798543,3.63167597545541,3.63527755095458,
3.64509264791623,3.70779093407981,3.76895962647601,3.78153107957739,3.78711309638645,
3.79136488400043,3.79299891134299,3.79305305852087,3.79310035613465,3.79319654675188,
3.79329026326948,3.79338166958506,3.79347091807018,3.79355815061592,3.79847576906934,
3.80864753015346,3.82183990298838,3.85332254606539,3.88265825429793,3.93807574898,
3.9461143581825,3.94920793378023,3.95143007220191,3.9538630573551,3.95739815317952,
3.96675441255142,3.9809423358345,4.06033164206889),.UNSPECIFIED.);
#1188=B_SPLINE_CURVE_WITH_KNOTS('',3,(#9052,#9053,#9054,#9055),
 .UNSPECIFIED.,.F.,.F.,(4,4),(0.00112887916970517,0.00138569478241305),
 .UNSPECIFIED.);
#1189=B_SPLINE_CURVE_WITH_KNOTS('',3,(#9061,#9062,#9063,#9064),
 .UNSPECIFIED.,.F.,.F.,(4,4),(4.05989386051375,4.06014004056529),
 .UNSPECIFIED.);
#1190=B_SPLINE_CURVE_WITH_KNOTS('',3,(#9065,#9066,#9067,#9068,#9069,#9070,
#9071,#9072,#9073,#9074,#9075,#9076,#9077,#9078,#9079,#9080,#9081,#9082,
#9083,#9084,#9085,#9086,#9087,#9088,#9089,#9090,#9091,#9092,#9093,#9094,
#9095,#9096,#9097,#9098,#9099,#9100,#9101,#9102,#9103,#9104,#9105,#9106,
#9107,#9108,#9109,#9110,#9111,#9112,#9113,#9114,#9115,#9116,#9117,#9118,
#9119,#9120,#9121,#9122,#9123,#9124,#9125,#9126,#9127,#9128,#9129,#9130,
#9131,#9132,#9133,#9134,#9135,#9136,#9137,#9138,#9139,#9140,#9141,#9142,
#9143,#9144,#9145,#9146,#9147,#9148,#9149,#9150,#9151,#9152,#9153,#9154,
#9155,#9156,#9157,#9158,#9159,#9160,#9161,#9162,#9163,#9164,#9165,#9166,
#9167,#9168,#9169,#9170,#9171,#9172,#9173,#9174,#9175,#9176,#9177,#9178,
#9179,#9180,#9181,#9182,#9183,#9184,#9185,#9186,#9187,#9188,#9189,#9190,
#9191,#9192,#9193,#9194,#9195,#9196,#9197,#9198,#9199,#9200,#9201,#9202,
#9203,#9204,#9205,#9206,#9207,#9208,#9209,#9210,#9211,#9212,#9213,#9214,
#9215,#9216,#9217,#9218,#9219,#9220,#9221,#9222,#9223,#9224,#9225,#9226,
#9227,#9228,#9229,#9230,#9231,#9232,#9233,#9234,#9235,#9236,#9237,#9238,
#9239,#9240,#9241,#9242,#9243,#9244,#9245,#9246,#9247,#9248,#9249,#9250,
#9251,#9252,#9253,#9254,#9255,#9256,#9257,#9258,#9259,#9260,#9261,#9262,
#9263,#9264,#9265,#9266,#9267,#9268),.UNSPECIFIED.,.F.,.F.,(4,2,2,2,2,2,
2,2,2,2,2,2,2,2,2,2,2,2,2,2,2,2,2,2,2,2,2,2,2,2,2,2,2,2,2,2,2,2,2,2,2,2,
2,2,2,2,2,2,2,2,2,2,2,2,2,2,2,2,2,2,2,2,2,2,2,2,2,2,2,2,2,2,2,2,2,2,2,2,
2,2,2,2,2,2,2,2,2,2,2,2,2,2,2,2,2,2,2,2,2,2,2,4),(0.00111348523567152,0.0224816007626239,
0.0901262012177608,0.100246350923435,0.103891281144555,0.10634714547644,
0.108549302474072,0.111562989800143,0.11910739814605,0.185509403693803,
0.229997598019453,0.246416065213366,0.25850663970398,0.263970423952956,
0.268226907461397,0.272764194180999,0.279882144044013,0.301033111249466,
0.399755124484115,0.4137431033698,0.423003543322421,0.426525378231244,0.428956524058265,
0.431182806531379,0.434289821560384,0.442419689913735,0.491956264196637,
0.53382936746426,0.561093271252557,0.578905500369908,0.585367538732415,
0.589766078637995,0.594056557024971,0.600192630588166,0.611491173796425,
0.670690552486911,0.735223835276311,0.745156642648614,0.748775685157619,
0.751226377402732,0.753433425081234,0.756465955988553,0.764120796493412,
0.828642753807549,0.895388726786414,0.904992749063346,0.910065418588115,
0.91421365812635,0.919100911398923,0.927592444692042,0.965684890353983,
1.0326688752449,1.06453190964363,1.06973662846895,1.07253292432333,1.07488613900785,
1.077869303875,1.08263246935774,1.11025244246143,1.19497168802161,1.21266583818951,
1.22557956722103,1.23128403640875,1.23554067053093,1.24007764965408,1.24719413334218,
1.26833238620149,1.36706965935031,1.38105830085798,1.39031907372458,1.39384096572875,
1.39627212890743,1.39849840963472,1.40160539910848,1.40973502039596,1.45927656418336,
1.50115852666669,1.52841438255367,1.54622286092332,1.5526844026193,1.55708285156407,
1.56137343093722,1.56750998060345,1.57881026456769,1.64235146004286,1.70288101210086,
1.7125563503411,1.71613883844027,1.71858208944097,1.72079601302236,1.72385546363711,
1.73167025832051,1.79317603254048,1.8408980902137,1.86671052084986,1.87408054325659,
1.87867305987981,1.88290977622055,1.88838666419224,1.90036204480245,1.97696467006013,
2.03118787455235),.UNSPECIFIED.);
#1191=B_SPLINE_CURVE_WITH_KNOTS('',3,(#9269,#9270,#9271,#9272,#9273,#9274,
#9275,#9276,#9277,#9278,#9279,#9280,#9281,#9282,#9283,#9284,#9285,#9286,
#9287,#9288,#9289,#9290,#9291,#9292,#9293,#9294,#9295,#9296,#9297,#9298,
#9299,#9300,#9301,#9302,#9303,#9304,#9305,#9306,#9307,#9308,#9309,#9310,
#9311,#9312,#9313,#9314,#9315,#9316,#9317,#9318,#9319,#9320,#9321,#9322,
#9323,#9324,#9325,#9326,#9327,#9328,#9329,#9330,#9331,#9332,#9333,#9334,
#9335,#9336,#9337,#9338,#9339,#9340,#9341,#9342,#9343,#9344,#9345,#9346,
#9347,#9348,#9349,#9350,#9351,#9352,#9353,#9354,#9355,#9356,#9357,#9358,
#9359,#9360,#9361,#9362,#9363,#9364,#9365,#9366,#9367,#9368,#9369,#9370,
#9371,#9372,#9373,#9374,#9375,#9376,#9377,#9378,#9379,#9380,#9381,#9382,
#9383,#9384,#9385,#9386,#9387,#9388,#9389,#9390,#9391,#9392,#9393,#9394,
#9395,#9396,#9397,#9398,#9399,#9400,#9401,#9402,#9403,#9404,#9405,#9406,
#9407,#9408,#9409,#9410,#9411,#9412,#9413,#9414,#9415,#9416,#9417,#9418,
#9419,#9420,#9421,#9422,#9423,#9424,#9425,#9426,#9427,#9428,#9429,#9430,
#9431,#9432,#9433,#9434,#9435,#9436,#9437,#9438,#9439,#9440,#9441,#9442,
#9443,#9444,#9445,#9446,#9447,#9448,#9449,#9450,#9451,#9452,#9453,#9454,
#9455,#9456,#9457,#9458,#9459,#9460,#9461,#9462,#9463,#9464,#9465,#9466,
#9467,#9468,#9469,#9470,#9471,#9472,#9473,#9474,#9475,#9476,#9477,#9478,
#9479,#9480,#9481,#9482,#9483,#9484,#9485,#9486,#9487,#9488,#9489,#9490,
#9491,#9492,#9493,#9494,#9495,#9496,#9497,#9498,#9499,#9500,#9501,#9502,
#9503,#9504,#9505,#9506,#9507,#9508,#9509,#9510,#9511,#9512,#9513,#9514),
 .UNSPECIFIED.,.F.,.F.,(4,2,2,2,2,2,2,2,2,2,2,2,2,2,2,2,2,2,2,2,2,2,2,2,
2,2,2,2,2,2,2,2,2,2,2,2,2,2,2,2,2,2,2,2,2,2,2,2,2,2,2,2,2,2,2,2,2,2,2,2,
2,2,2,2,2,2,2,2,2,2,2,2,2,2,2,2,2,2,2,2,2,2,2,2,2,2,2,2,2,2,2,2,2,2,2,2,
2,2,2,2,2,2,2,2,2,2,2,2,2,2,2,2,2,2,2,2,2,2,2,2,2,2,4),(0.00138569478241305,
0.0267213414297853,0.0408251368465114,0.0462378673492938,0.0503775404732197,
0.0543978425872758,0.0589295209120385,0.0660224417239157,0.08696289358787,
0.115688684107862,0.155137456901873,0.204341363940377,0.210423711120401,
0.213399555807341,0.21552628154065,0.218235077329387,0.222910379132293,
0.241786800393865,0.259796115646,0.318478283315475,0.346593894146785,0.358827616224174,
0.368432488138858,0.373476715932667,0.37351491088737,0.373555770386838,
0.373599488837467,0.373646275847383,0.373696357497504,0.373749977729205,
0.373807399865922,0.373868908246732,0.373934809986602,0.374005436893115,
0.374081147488881,0.374162329195859,0.374249400619812,0.378441099864665,
0.383607964054376,0.391528942332894,0.432499708934886,0.497034964896065,
0.528138629967786,0.533315707151181,0.536105822897071,0.53845904938096,
0.541448851836776,0.546235015476269,0.574430401252419,0.658606133568633,
0.676252530802476,0.689139071104937,0.694838170496325,0.699093347876914,
0.703631160320024,0.710753956023984,0.731953135923117,0.830612365047775,
0.844596881256467,0.853855268463663,0.857376425466993,0.859807131914509,
0.86203302249243,0.865139489799158,0.873267899031018,0.922812835964177,
0.964702884909765,0.991947171916137,1.00974951825666,1.0162095182313,1.02060709900641,
1.02489696537361,1.03103272023084,1.04233208688768,1.1058367902302,1.16639282644824,
1.17606915969118,1.17965140193449,1.18209429452891,1.18430773159755,1.18796243260164,
1.19738494437535,1.30131284910325,1.32020849299303,1.33378560522356,1.33960322662293,
1.34387765679379,1.34837256205309,1.35529793890983,1.37497210811089,1.47544378061878,
1.4895000366673,1.49879330955964,1.50231946935156,1.50475101417417,1.50697558476106,
1.51007747627904,1.51817301458386,1.56909105305033,1.6140955276345,1.65117090383273,
1.65938349986985,1.66415942851689,1.66835600617083,1.67359075817074,1.68173496178498,
1.73035500514378,1.79467135058144,1.81062226787019,1.82081769722814,1.82447262464397,
1.8269302756948,1.8291302134018,1.83213601309703,1.83963587039484,1.9065834288418,
1.97084737961853,1.98060519909095,1.98570875135073,1.98949137605346,1.99421996306415,
2.00221618307605,2.03141751110446),.UNSPECIFIED.);
#1192=B_SPLINE_CURVE_WITH_KNOTS('',3,(#9519,#9520,#9521,#9522,#9523,#9524,
#9525,#9526,#9527,#9528,#9529,#9530,#9531,#9532,#9533,#9534,#9535,#9536,
#9537,#9538,#9539,#9540,#9541,#9542,#9543,#9544,#9545,#9546,#9547,#9548,
#9549,#9550,#9551,#9552,#9553,#9554,#9555,#9556,#9557,#9558,#9559,#9560,
#9561,#9562,#9563,#9564,#9565,#9566,#9567,#9568,#9569,#9570,#9571,#9572,
#9573,#9574,#9575,#9576,#9577,#9578,#9579,#9580,#9581,#9582,#9583,#9584,
#9585,#9586,#9587,#9588,#9589,#9590,#9591,#9592,#9593,#9594,#9595,#9596,
#9597,#9598,#9599,#9600,#9601,#9602,#9603,#9604,#9605,#9606,#9607,#9608,
#9609,#9610,#9611,#9612,#9613,#9614,#9615,#9616,#9617,#9618,#9619,#9620,
#9621,#9622,#9623,#9624,#9625,#9626,#9627,#9628,#9629,#9630,#9631,#9632,
#9633,#9634,#9635,#9636,#9637,#9638,#9639,#9640,#9641,#9642,#9643,#9644,
#9645,#9646,#9647,#9648,#9649,#9650,#9651,#9652,#9653,#9654,#9655,#9656,
#9657,#9658,#9659,#9660,#9661,#9662,#9663,#9664,#9665,#9666,#9667,#9668,
#9669,#9670,#9671,#9672,#9673,#9674,#9675,#9676,#9677,#9678,#9679,#9680,
#9681,#9682,#9683,#9684,#9685,#9686,#9687,#9688,#9689,#9690,#9691,#9692,
#9693,#9694,#9695,#9696,#9697,#9698,#9699,#9700,#9701,#9702,#9703,#9704,
#9705,#9706,#9707,#9708,#9709,#9710,#9711,#9712,#9713,#9714,#9715,#9716,
#9717,#9718,#9719,#9720,#9721,#9722,#9723,#9724,#9725,#9726,#9727,#9728,
#9729,#9730,#9731,#9732,#9733,#9734,#9735,#9736),.UNSPECIFIED.,.F.,.F.,
(4,2,2,2,2,2,2,2,2,2,2,2,2,2,2,2,2,2,2,2,2,2,2,2,2,2,2,2,2,2,2,2,2,2,2,
2,2,2,2,2,2,2,2,2,2,2,2,2,2,2,2,2,2,2,2,2,2,2,2,2,2,2,2,2,2,2,2,2,2,2,2,
2,2,2,2,2,2,2,2,2,2,2,2,2,2,2,2,2,2,2,2,2,2,2,2,2,2,2,2,2,2,2,2,2,2,2,2,
2,4),(2.03078233277413,2.05701474884909,2.06473078008979,2.06939792509912,
2.07361238998611,2.07902521861311,2.09034612622446,2.13438924023311,2.18871322588318,
2.22220599552371,2.22717223774696,2.23021557887311,2.2325725205178,2.23532240679641,
2.24031298585521,2.26691708277014,2.35435241548298,2.37955708470908,2.38714104364052,
2.39177888272704,2.39599969979284,2.40146708392961,2.41307917357678,2.45943370353251,
2.53655785716989,2.54751133360523,2.55139279923023,2.55364965670384,2.55605514036883,
2.5594446101676,2.56785311667929,2.58014540046924,2.6189750865854,2.6943339615967,
2.70640696476809,2.71189995836232,2.71613747650923,2.72071929588646,2.72804683584302,
2.75343799314438,2.7998749849234,2.86320462922567,2.87089746669002,2.87393548423825,
2.87614320917402,2.87859067704753,2.88219819085504,2.89205693805071,2.95545406107523,
3.0158398079194,3.02840593896334,3.0339866498923,3.03823786678702,3.0427819956265,
3.04993698955352,3.07359870563441,3.11502762492672,3.18052306976554,3.19187636999115,
3.1958133020623,3.19808101783125,3.20047945327617,3.20382930585367,3.21199360710417,
3.22381397324974,3.26014505159502,3.33934521446711,3.34990240154371,3.35524315227204,
3.35918272682049,3.36347023621106,3.36936612660064,3.38341581095883,3.45295128470277,
3.50717823148167,3.51524274842077,3.51833980134792,3.52056273438184,3.52299461512872,
3.52652484035116,3.53584934819174,3.5499726453274,3.65221007564477,3.67044300038479,
3.6771662715017,3.68117223256025,3.68541577713138,3.69073923512959,3.70239876617017,
3.71803415508925,3.75909665197433,3.82346919710859,3.83610422941879,3.84020825199906,
3.84276275113584,3.84517776000279,3.84862175762956,3.85737947082623,3.87035951401955,
3.9381573549767,3.96722909062668,3.99112001235569,3.99855299014072,4.0031571303506,
4.00738614355311,4.01151265483841,4.01689034996646,4.03172592743479,4.05989386051375),
 .UNSPECIFIED.);
#1193=B_SPLINE_CURVE_WITH_KNOTS('',3,(#9737,#9738,#9739,#9740,#9741,#9742,
#9743,#9744,#9745,#9746,#9747,#9748,#9749,#9750,#9751,#9752,#9753,#9754,
#9755,#9756,#9757,#9758,#9759,#9760,#9761,#9762,#9763,#9764,#9765,#9766,
#9767,#9768,#9769,#9770,#9771,#9772,#9773,#9774,#9775,#9776,#9777,#9778,
#9779,#9780,#9781,#9782,#9783,#9784,#9785,#9786,#9787,#9788,#9789,#9790,
#9791,#9792,#9793,#9794,#9795,#9796,#9797,#9798,#9799,#9800,#9801,#9802,
#9803,#9804,#9805,#9806,#9807,#9808,#9809,#9810,#9811,#9812,#9813,#9814,
#9815,#9816,#9817,#9818,#9819,#9820,#9821,#9822,#9823,#9824,#9825,#9826,
#9827,#9828,#9829,#9830,#9831,#9832,#9833,#9834,#9835,#9836,#9837,#9838,
#9839,#9840,#9841,#9842,#9843,#9844,#9845,#9846,#9847,#9848,#9849,#9850,
#9851,#9852,#9853,#9854,#9855,#9856,#9857,#9858,#9859,#9860,#9861,#9862,
#9863,#9864,#9865,#9866,#9867,#9868,#9869,#9870,#9871,#9872,#9873,#9874,
#9875,#9876,#9877,#9878,#9879,#9880,#9881,#9882,#9883,#9884,#9885,#9886,
#9887,#9888,#9889,#9890,#9891,#9892,#9893,#9894,#9895,#9896,#9897,#9898,
#9899,#9900,#9901,#9902,#9903,#9904,#9905,#9906,#9907,#9908,#9909,#9910,
#9911,#9912,#9913,#9914,#9915,#9916,#9917,#9918,#9919,#9920,#9921,#9922,
#9923,#9924,#9925,#9926,#9927,#9928,#9929,#9930,#9931,#9932,#9933,#9934,
#9935,#9936,#9937,#9938,#9939,#9940,#9941,#9942),.UNSPECIFIED.,.F.,.F.,
(4,2,2,2,2,2,2,2,2,2,2,2,2,2,2,2,2,2,2,2,2,2,2,2,2,2,2,2,2,2,2,2,2,2,2,
2,2,2,2,2,2,2,2,2,2,2,2,2,2,2,2,2,2,2,2,2,2,2,2,2,2,2,2,2,2,2,2,2,2,2,2,
2,2,2,2,2,2,2,2,2,2,2,2,2,2,2,2,2,2,2,2,2,2,2,2,2,2,2,2,2,2,2,4),(2.03141751110446,
2.03161830192352,2.09123891434952,2.13952401981648,2.14458719413026,2.14762663706429,
2.14998834914161,2.15270704310881,2.15755302771701,2.18131190211232,2.24528898181316,
2.29433678003636,2.30249303325431,2.30773114366241,2.31192762581724,2.31670043479166,
2.32490008025686,2.36176996849567,2.4068735926888,2.45783800300492,2.46593108065273,
2.46903234995985,2.47125659537007,2.473687903252,2.47721393412981,2.48650796173833,
2.50056793355411,2.60106680936354,2.62074474348472,2.62766996689504,2.63216435541657,
2.63643798923999,2.64225404948089,2.65582538994824,2.67470925824242,2.77853019570927,
2.78798409861485,2.79164334825657,2.79385727399629,2.79629851129585,2.79987463715443,
2.80951198480618,2.8695049850929,2.93366203436167,2.94495486772932,2.95108801564918,
2.95537656629576,2.95977321855179,2.96623264768075,2.98403888376495,3.01129067961153,
3.05311352647787,3.10260650690707,3.11073056980414,3.11383583214611,3.11606101290349,
3.11849110028305,3.12201163711483,3.13126983827728,3.14525693852776,3.24395678793102,
3.26513162701057,3.27225016583536,3.27678608273155,3.28104005029894,3.28673839608964,
3.29962711084333,3.31727719145908,3.40156538659544,3.42954704371025,3.4343229838228,
3.43730918281886,3.43966142643616,3.44245254966432,3.44763718099059,3.47898369327795,
3.54420209592779,3.55667822944215,3.5857464284422,3.59371174068327,3.59843277690088,
3.60221532014369,3.60732652410096,3.61712569014735,3.68273673647865,3.74808621824093,
3.75563632499945,3.75865015644376,3.76085167085968,3.76325665991628,3.76665422237609,
3.77067044364147,3.77799813593805,3.79535607494124,3.87515547019287,3.90757173847285,
3.91569716153532,3.92049941471741,3.92469135940706,3.92988425143375,3.94008589735922,
4.00006936679343,4.06108277158193),.UNSPECIFIED.);
#1194=B_SPLINE_CURVE_WITH_KNOTS('',3,(#9947,#9948,#9949,#9950,#9951,#9952,
#9953,#9954,#9955,#9956,#9957,#9958,#9959,#9960,#9961,#9962,#9963,#9964,
#9965,#9966,#9967,#9968,#9969,#9970,#9971,#9972,#9973,#9974,#9975,#9976,
#9977,#9978,#9979,#9980,#9981,#9982,#9983,#9984,#9985,#9986,#9987,#9988,
#9989,#9990,#9991,#9992,#9993,#9994,#9995,#9996,#9997,#9998,#9999,#10000,
#10001,#10002,#10003,#10004,#10005,#10006,#10007,#10008,#10009,#10010,#10011,
#10012,#10013,#10014,#10015,#10016,#10017,#10018,#10019,#10020,#10021,#10022,
#10023,#10024,#10025,#10026,#10027,#10028,#10029,#10030,#10031,#10032,#10033,
#10034,#10035,#10036,#10037,#10038,#10039,#10040,#10041,#10042,#10043,#10044,
#10045,#10046,#10047,#10048,#10049,#10050,#10051,#10052,#10053,#10054,#10055,
#10056,#10057,#10058,#10059,#10060,#10061,#10062,#10063,#10064,#10065,#10066,
#10067,#10068,#10069,#10070,#10071,#10072,#10073,#10074,#10075,#10076,#10077,
#10078,#10079,#10080,#10081,#10082,#10083,#10084,#10085,#10086,#10087,#10088,
#10089,#10090,#10091,#10092,#10093,#10094,#10095,#10096,#10097,#10098,#10099,
#10100,#10101,#10102,#10103,#10104,#10105,#10106,#10107,#10108,#10109,#10110,
#10111,#10112,#10113,#10114,#10115,#10116,#10117,#10118,#10119,#10120,#10121,
#10122,#10123,#10124,#10125,#10126,#10127,#10128,#10129,#10130,#10131,#10132,
#10133,#10134,#10135,#10136,#10137,#10138,#10139,#10140,#10141,#10142,#10143,
#10144,#10145,#10146,#10147,#10148,#10149,#10150,#10151,#10152,#10153,#10154,
#10155,#10156,#10157,#10158,#10159,#10160),.UNSPECIFIED.,.F.,.F.,(4,2,2,
2,2,2,2,2,2,2,2,2,2,2,2,2,2,2,2,2,2,2,2,2,2,2,2,2,2,2,2,2,2,2,2,2,2,2,2,
2,2,2,2,2,2,2,2,2,2,2,2,2,2,2,2,2,2,2,2,2,2,2,2,2,2,2,2,2,2,2,2,2,2,2,2,
2,2,2,2,2,2,2,2,2,2,2,2,2,2,2,2,2,2,2,2,2,2,2,2,2,2,2,2,2,2,2,4),(0.00133785408364666,
0.0856446905644938,0.122424369273886,0.130619548823976,0.135391751336176,
0.139588895196584,0.144829411282487,0.152992426471294,0.202280327718648,
0.232371091602562,0.271726767326629,0.284116017797875,0.289917394424944,
0.294484431904405,0.297168247421122,0.299441867234976,0.302455039434137,
0.307319419132626,0.337606206181498,0.400229279607729,0.429283530695928,
0.441789773401134,0.451645353802899,0.456769108232272,0.460958096126468,
0.465816054162684,0.47418138133987,0.510146124647116,0.578701652886667,
0.600755850148186,0.609370945059377,0.615780121469759,0.618819460377261,
0.621176317749108,0.623929610123252,0.628800016880675,0.650298526928026,
0.658625984900809,0.741936234768132,0.759505277556927,0.772348261240176,
0.778039530209684,0.782293290394936,0.786833758300268,0.79396951646743,
0.81528193128391,0.832037407607788,0.90082236936071,0.933577603067133,0.938811250509593,
0.941613160343803,0.943965183938087,0.946939334546403,0.951674161147222,
0.978643077751603,1.06393850810934,1.09071853919903,1.09817571901747,1.10278602781095,
1.10701484654733,1.11244765221054,1.12418915702739,1.20316690973005,1.25446502501371,
1.26060306725689,1.26358957727483,1.26571721569795,1.26841800222674,1.27305964407883,
1.29152930041788,1.30297675943305,1.35687929893693,1.40552039177682,1.41741174239851,
1.42293145473048,1.42715963511997,1.43177285553398,1.43924283045255,1.46345611036264,
1.53390562619572,1.57774569770444,1.58324526712038,1.58610286705057,1.58845239375949,
1.59136227229474,1.59693913841422,1.63945863497612,1.65236283912661,1.69852166868732,
1.73399920493521,1.74211419439026,1.746868593284,1.75106753235136,1.75633341305377,
1.764581211114,1.8294960181138,1.88010504815956,1.89432755814597,1.90370156891809,
1.90723944827798,1.90967314008361,1.91189496461671,1.91498689290402,1.92301254776039,
1.97924609245589,2.03056810395715,2.03078233277413),.UNSPECIFIED.);
#1195=B_SPLINE_CURVE_WITH_KNOTS('',3,(#10162,#10163,#10164,#10165),
 .UNSPECIFIED.,.F.,.F.,(4,4),(4.06108277158193,4.06123005647539),
 .UNSPECIFIED.);
#1196=B_SPLINE_CURVE_WITH_KNOTS('',3,(#10166,#10167,#10168,#10169,#10170,
#10171,#10172,#10173,#10174,#10175,#10176,#10177,#10178,#10179,#10180,#10181,
#10182,#10183,#10184,#10185,#10186,#10187,#10188,#10189,#10190,#10191,#10192,
#10193,#10194,#10195,#10196,#10197,#10198,#10199,#10200,#10201,#10202,#10203,
#10204,#10205,#10206,#10207,#10208,#10209,#10210,#10211,#10212,#10213,#10214,
#10215,#10216,#10217,#10218,#10219,#10220,#10221,#10222,#10223,#10224,#10225,
#10226,#10227,#10228,#10229,#10230,#10231,#10232,#10233,#10234,#10235,#10236,
#10237,#10238,#10239,#10240,#10241,#10242,#10243,#10244,#10245,#10246,#10247,
#10248,#10249,#10250,#10251,#10252,#10253,#10254,#10255,#10256,#10257,#10258,
#10259,#10260,#10261,#10262,#10263,#10264,#10265,#10266,#10267,#10268,#10269,
#10270,#10271,#10272,#10273,#10274,#10275,#10276,#10277,#10278,#10279,#10280,
#10281,#10282,#10283,#10284,#10285,#10286,#10287,#10288,#10289,#10290,#10291,
#10292,#10293,#10294,#10295,#10296,#10297,#10298,#10299,#10300,#10301,#10302,
#10303,#10304,#10305,#10306,#10307,#10308,#10309,#10310,#10311,#10312,#10313,
#10314,#10315,#10316,#10317,#10318,#10319,#10320,#10321,#10322,#10323,#10324,
#10325,#10326,#10327,#10328,#10329,#10330,#10331,#10332,#10333,#10334,#10335,
#10336,#10337,#10338,#10339,#10340,#10341,#10342,#10343,#10344,#10345,#10346,
#10347,#10348,#10349,#10350,#10351,#10352,#10353,#10354,#10355,#10356,#10357,
#10358,#10359,#10360,#10361,#10362,#10363,#10364,#10365,#10366,#10367,#10368,
#10369,#10370,#10371,#10372,#10373,#10374,#10375,#10376,#10377,#10378,#10379,
#10380,#10381,#10382,#10383,#10384,#10385),.UNSPECIFIED.,.F.,.F.,(4,2,2,
2,2,2,2,2,2,2,2,2,2,2,2,2,2,2,2,2,2,2,2,2,2,2,2,2,2,2,2,2,2,2,2,2,2,2,2,
2,2,2,2,2,2,2,2,2,2,2,2,2,2,2,2,2,2,2,2,2,2,2,2,2,2,2,2,2,2,2,2,2,2,2,2,
2,2,2,2,2,2,2,2,2,2,2,2,2,2,2,2,2,2,2,2,2,2,2,2,2,2,2,2,2,2,2,2,2,2,4),
(0.00121494437820566,0.0110361665019738,0.0175286064381429,0.0202186781558045,
0.0224361585553646,0.024688223990178,0.0277264892490866,0.0341297955183033,
0.0525492195787883,0.101534616884938,0.16712361780516,0.176925211388578,
0.182037979192517,0.186226504471999,0.191093539198829,0.199498524411382,
0.236051393496236,0.311691777226034,0.328721898705432,0.335955557793333,
0.3399364298102,0.343377037528105,0.345766590671855,0.34798396783837,0.351660042345005,
0.361218153486806,0.464967376756704,0.483854905481767,0.497427387690942,
0.503244014607295,0.507518077682627,0.512012927590382,0.518938889311041,
0.538619475515404,0.639075929909461,0.653130982850428,0.662423521828384,
0.665949443411343,0.668380836701181,0.670605278814104,0.673707004490731,
0.681802209719301,0.732653298747103,0.779291827000504,0.814950317454205,
0.823076865996563,0.827833875829596,0.832032598530283,0.837294854313059,
0.845530379778327,0.909080647558641,0.96032546087957,0.975017586554573,
0.984618643950791,0.988189693159059,0.990630049122151,0.992845200938749,
0.996510324930135,1.00599994239505,1.10982373079634,1.12871278344703,1.14228576587521,
1.14810211707737,1.15237579747298,1.15687008115234,1.16379483847946,1.18346964695222,
1.28392037135659,1.29797416392352,1.30726583912665,1.31079141301791,1.31322256024172,
1.3154467721997,1.31854817036355,1.32664247140017,1.37751960319005,1.42413134557623,
1.45977802037419,1.46790322919262,1.47265964171562,1.47685795019831,1.48211983672294,
1.49035507813956,1.55373945001163,1.60273633120165,1.62687127579128,1.63173735238195,
1.63446027282125,1.63682102982063,1.63985342979978,1.64489294222184,1.68329757418375,
1.74675996326157,1.78209350692148,1.79019907981403,1.79495120894009,1.7991501047521,
1.80441853144757,1.81267540833835,1.87404164475143,1.92751968150728,1.94214609837832,
1.95171531626248,1.9552815328654,1.95772073749243,1.95993654073915,1.96300574714687,
1.97088400219229,2.03074823704563,2.03104238026227),.UNSPECIFIED.);
#1197=B_SPLINE_CURVE_WITH_KNOTS('',3,(#10391,#10392,#10393,#10394,#10395,
#10396,#10397,#10398,#10399,#10400,#10401,#10402,#10403,#10404,#10405,#10406,
#10407,#10408,#10409,#10410,#10411,#10412,#10413,#10414,#10415,#10416,#10417,
#10418,#10419,#10420,#10421,#10422,#10423,#10424,#10425,#10426,#10427,#10428,
#10429,#10430,#10431,#10432,#10433,#10434,#10435,#10436,#10437,#10438,#10439,
#10440,#10441,#10442,#10443,#10444,#10445,#10446,#10447,#10448,#10449,#10450,
#10451,#10452,#10453,#10454,#10455,#10456,#10457,#10458,#10459,#10460,#10461,
#10462,#10463,#10464,#10465,#10466,#10467,#10468,#10469,#10470,#10471,#10472,
#10473,#10474,#10475,#10476,#10477,#10478,#10479,#10480,#10481,#10482,#10483,
#10484,#10485,#10486,#10487,#10488,#10489,#10490,#10491,#10492,#10493,#10494,
#10495,#10496,#10497,#10498,#10499,#10500,#10501,#10502,#10503,#10504,#10505,
#10506,#10507,#10508,#10509,#10510,#10511,#10512,#10513,#10514,#10515,#10516,
#10517,#10518,#10519,#10520,#10521,#10522,#10523,#10524,#10525,#10526,#10527,
#10528,#10529,#10530,#10531,#10532,#10533,#10534,#10535,#10536,#10537,#10538,
#10539,#10540,#10541,#10542,#10543,#10544,#10545,#10546,#10547,#10548,#10549,
#10550,#10551,#10552,#10553,#10554,#10555,#10556,#10557,#10558,#10559,#10560,
#10561,#10562,#10563,#10564,#10565,#10566,#10567,#10568,#10569,#10570,#10571,
#10572,#10573,#10574,#10575,#10576,#10577,#10578,#10579,#10580,#10581,#10582,
#10583,#10584,#10585,#10586,#10587,#10588,#10589,#10590,#10591,#10592,#10593,
#10594,#10595,#10596,#10597,#10598,#10599,#10600,#10601,#10602,#10603,#10604,
#10605,#10606,#10607,#10608,#10609,#10610,#10611,#10612,#10613,#10614),
 .UNSPECIFIED.,.F.,.F.,(4,2,2,2,2,2,2,2,2,2,2,2,2,2,2,2,2,2,2,2,2,2,2,2,
2,2,2,2,2,2,2,2,2,2,2,2,2,2,2,2,2,2,2,2,2,2,2,2,2,2,2,2,2,2,2,2,2,2,2,2,
2,2,2,2,2,2,2,2,2,2,2,2,2,2,2,2,2,2,2,2,2,2,2,2,2,2,2,2,2,2,2,2,2,2,2,2,
2,2,2,2,2,2,2,2,2,2,2,2,2,2,2,4),(2.03130412200221,2.03159818914461,2.08772320577085,
2.0957527707976,2.09884565652699,2.10106805355868,2.10350221507385,2.10704053262685,
2.11641413762186,2.13063628820749,2.18122394352423,2.24087321478513,2.25344102976112,
2.25902336299018,2.2632761588798,2.26782230738462,2.27498118413346,2.29866252645453,
2.34013626646325,2.4057494348067,2.41700386422519,2.42092813416422,2.42319393413138,
2.4255950129249,2.42895601204101,2.43718379074069,2.44912471045109,2.48607261896767,
2.56435277197644,2.57617548651034,2.58162409555845,2.58585614438439,2.59046085540838,
2.59788868383068,2.62433201270105,2.70710180167611,2.71421797542152,2.73733688044322,
2.74231078912408,2.74508781395693,2.74744251782633,2.75045027257915,2.75669431730239,
2.76502503589402,2.78599701818555,2.84994284859199,2.89167719950095,2.89957689543349,
2.90473754649871,2.90892929991236,2.91375993323543,2.92222262214858,2.96397581402302,
3.02099412247387,3.05874272827858,3.0637727282486,3.06680282896265,3.06916395463783,
3.07188981872865,3.07676721488255,3.10109110451491,3.1499163565872,3.2133563160021,
3.22159426090094,3.22685773909182,3.23105726818484,3.23581501581692,3.2439424182159,
3.27960156205471,3.32624072037417,3.37703053618904,3.38512501366353,3.3882269225244,
3.3904516541001,3.39288353752763,3.39641049889102,3.40570756356702,3.41977277016236,
3.52037034318773,3.53997711545056,3.54689389225322,3.55138714413535,3.55566284828734,
3.56148669911958,3.57509953733178,3.59405818932627,3.6950714440059,3.70656512687793,
3.71052198386052,3.7127941338675,3.71514342943226,3.71836722028747,3.7220390594721,
3.72847385963401,3.74284904014334,3.79450484163212,3.858238837025,3.8664742612871,
3.87173682841542,3.87593607615401,3.88069398203353,3.88882284477652,3.92451054746185,
4.00299342900153,4.02155406800738,4.02995181813464,4.03343836083613,4.03583835866016,
4.03803438413862,4.04055012496013,4.04412071707633,4.06112080728385),
 .UNSPECIFIED.);
#1198=B_SPLINE_CURVE_WITH_KNOTS('',3,(#10615,#10616,#10617,#10618),
 .UNSPECIFIED.,.F.,.F.,(4,4),(0.00120377071706689,0.00133785408364666),
 .UNSPECIFIED.);
#1199=B_SPLINE_CURVE_WITH_KNOTS('',3,(#10619,#10620,#10621,#10622,#10623,
#10624,#10625,#10626,#10627,#10628,#10629,#10630,#10631,#10632,#10633,#10634,
#10635,#10636,#10637,#10638,#10639,#10640,#10641,#10642,#10643,#10644,#10645,
#10646,#10647,#10648,#10649,#10650,#10651,#10652,#10653,#10654,#10655,#10656,
#10657,#10658,#10659,#10660,#10661,#10662,#10663,#10664,#10665,#10666,#10667,
#10668,#10669,#10670,#10671,#10672,#10673,#10674,#10675,#10676,#10677,#10678,
#10679,#10680,#10681,#10682,#10683,#10684,#10685,#10686,#10687,#10688,#10689,
#10690,#10691,#10692,#10693,#10694,#10695,#10696,#10697,#10698,#10699,#10700,
#10701,#10702,#10703,#10704,#10705,#10706,#10707,#10708,#10709,#10710,#10711,
#10712,#10713,#10714,#10715,#10716,#10717,#10718,#10719,#10720,#10721,#10722,
#10723,#10724,#10725,#10726,#10727,#10728,#10729,#10730,#10731,#10732,#10733,
#10734,#10735,#10736,#10737,#10738,#10739,#10740,#10741,#10742,#10743,#10744,
#10745,#10746,#10747,#10748,#10749,#10750,#10751,#10752,#10753,#10754,#10755,
#10756,#10757,#10758,#10759,#10760,#10761,#10762,#10763,#10764,#10765,#10766,
#10767,#10768,#10769,#10770,#10771,#10772,#10773,#10774,#10775,#10776,#10777,
#10778,#10779,#10780,#10781,#10782,#10783,#10784,#10785,#10786,#10787,#10788,
#10789,#10790,#10791,#10792,#10793,#10794,#10795,#10796,#10797,#10798,#10799,
#10800,#10801,#10802,#10803,#10804,#10805,#10806,#10807,#10808,#10809,#10810,
#10811,#10812,#10813,#10814,#10815,#10816,#10817,#10818,#10819,#10820,#10821,
#10822,#10823,#10824,#10825,#10826,#10827,#10828,#10829,#10830,#10831,#10832,
#10833,#10834,#10835,#10836),.UNSPECIFIED.,.F.,.F.,(4,2,2,2,2,2,2,2,2,2,
2,2,2,2,2,2,2,2,2,2,2,2,2,2,2,2,2,2,2,2,2,2,2,2,2,2,2,2,2,2,2,2,2,2,2,2,
2,2,2,2,2,2,2,2,2,2,2,2,2,2,2,2,2,2,2,2,2,2,2,2,2,2,2,2,2,2,2,2,2,2,2,2,
2,2,2,2,2,2,2,2,2,2,2,2,2,2,2,2,2,2,2,2,2,2,2,2,2,2,4),(2.03104238026227,
2.09724542452292,2.10958014687469,2.11470220533646,2.11897823506359,2.12339070044557,
2.12992747070857,2.14831097586602,2.17680989517851,2.23818411945571,2.25279894878368,
2.27166408981011,2.2763375696431,2.27904552430693,2.28117169927647,2.28414695405555,
2.2902286742074,2.33944382197764,2.39958941507056,2.42716490016722,2.43498533056113,
2.43967496086213,2.44388403670093,2.44925442402646,2.46035559345829,2.50271421110341,
2.57034551267571,2.59339390432458,2.5983622924609,2.60113743175028,2.60349129734894,
2.6064989339772,2.61274592863724,2.62108258912497,2.64208060718408,2.70620503857858,
2.74769742203716,2.75558830570707,2.76074520127322,2.76493521875067,2.76976530601767,
2.77823083738869,2.82009296209893,2.8773436686462,2.91471534053356,2.91973776613717,
2.92276505414384,2.92512508999524,2.92785096815099,2.93273139858635,2.95713760355033,
3.00588638951751,3.06927598660031,3.07751105570501,3.0827725961731,3.08697050810402,
3.09172634172455,3.09985025279019,3.13548882473561,3.18208799443039,3.23290457360636,
3.24099645609327,3.24409724081228,3.24632113203405,3.24875204502355,3.25227749035114,
3.26156990065317,3.27562736098389,3.37610367943317,3.39578374012999,3.40270854645824,
3.40720236150998,3.4114752311517,3.41728990700404,3.43085641042182,3.44973238587553,
3.55341670789118,3.5629638718,3.56663749073389,3.56885388471243,3.57129186371868,
3.57485315179539,3.58439029039193,3.5989524292132,3.65195911205504,3.71396163534035,
3.72294157396361,3.7279756972016,3.73207673277969,3.7368718033689,3.7419813495068,
3.76258159138641,3.79614747560425,3.87553996959618,3.88520074504443,3.88889174257148,
3.89111147880631,3.89354631154953,3.89709157713696,3.90651843912977,3.92085221103114,
3.97223147174009,4.0190802381283,4.04007701665561,4.04702611149955,4.05158544928812,
4.0556183792297,4.05837181477896,4.0604205322052),.UNSPECIFIED.);
#1200=B_SPLINE_CURVE_WITH_KNOTS('',3,(#10841,#10842,#10843,#10844,#10845,
#10846,#10847,#10848,#10849,#10850,#10851,#10852,#10853,#10854,#10855,#10856,
#10857,#10858,#10859,#10860,#10861,#10862,#10863,#10864,#10865,#10866,#10867,
#10868,#10869,#10870,#10871,#10872,#10873,#10874,#10875,#10876,#10877,#10878,
#10879,#10880,#10881,#10882,#10883,#10884,#10885,#10886,#10887,#10888,#10889,
#10890,#10891,#10892,#10893,#10894,#10895,#10896,#10897,#10898,#10899,#10900,
#10901,#10902,#10903,#10904,#10905,#10906,#10907,#10908,#10909,#10910,#10911,
#10912,#10913,#10914,#10915,#10916,#10917,#10918,#10919,#10920,#10921,#10922,
#10923,#10924,#10925,#10926,#10927,#10928,#10929,#10930,#10931,#10932,#10933,
#10934,#10935,#10936,#10937,#10938,#10939,#10940,#10941,#10942,#10943,#10944,
#10945,#10946,#10947,#10948,#10949,#10950,#10951,#10952,#10953,#10954,#10955,
#10956,#10957,#10958,#10959,#10960,#10961,#10962,#10963,#10964,#10965,#10966,
#10967,#10968,#10969,#10970,#10971,#10972,#10973,#10974,#10975,#10976,#10977,
#10978,#10979,#10980,#10981,#10982,#10983,#10984,#10985,#10986,#10987,#10988,
#10989,#10990,#10991,#10992,#10993,#10994,#10995,#10996,#10997,#10998,#10999,
#11000,#11001,#11002,#11003,#11004,#11005,#11006,#11007,#11008,#11009,#11010,
#11011,#11012,#11013,#11014,#11015,#11016,#11017,#11018,#11019,#11020,#11021,
#11022,#11023,#11024,#11025,#11026,#11027,#11028,#11029,#11030,#11031,#11032,
#11033,#11034,#11035,#11036,#11037,#11038,#11039,#11040,#11041,#11042,#11043,
#11044,#11045,#11046,#11047,#11048,#11049,#11050,#11051,#11052),
 .UNSPECIFIED.,.F.,.F.,(4,2,2,2,2,2,2,2,2,2,2,2,2,2,2,2,2,2,2,2,2,2,2,2,
2,2,2,2,2,2,2,2,2,2,2,2,2,2,2,2,2,2,2,2,2,2,2,2,2,2,2,2,2,2,2,2,2,2,2,2,
2,2,2,2,2,2,2,2,2,2,2,2,2,2,2,2,2,2,2,2,2,2,2,2,2,2,2,2,2,2,2,2,2,2,2,2,
2,2,2,2,2,2,2,2,2,4),(0.00125155003270578,0.0033132412163655,0.00662460547463569,
0.0106349599505179,0.0171288983854706,0.0347121459144986,0.0495379607755764,
0.131385330900832,0.158297684923628,0.163303816321884,0.166057685301177,
0.168415134003331,0.171455391128603,0.176409326417822,0.209498440746812,
0.28220805351899,0.314242264093352,0.322126805827004,0.326106965746669,
0.330209623558016,0.335034045232269,0.343522013722197,0.382132439440515,
0.4486397705076,0.470079459925927,0.482653924452503,0.486607217852261,0.489129572222461,
0.491538883006436,0.494509113523836,0.501800706094395,0.570913410083924,
0.613759433789263,0.637929535964344,0.645138775441384,0.649696029864435,
0.653944780123184,0.659500971845563,0.671919822664633,0.740922541111079,
0.784229319441231,0.797311548801108,0.806122767466081,0.809576359706321,
0.811994288352569,0.814547929292512,0.818643395444061,0.831197085470782,
0.930913367662087,0.949882764852105,0.963500452931096,0.96932533312387,
0.973601394208901,0.978094657373839,0.98501072290671,1.00461068785063,1.10517155477238,
1.11923159298535,1.12852693568994,1.13205365404792,1.13448551638714,1.13671033581554,
1.13981253432267,1.14790859197987,1.198751894151,1.24539996395251,1.28106393319932,
1.28919181023295,1.29394964434165,1.2981491289487,1.30341239195831,1.31164961417293,
1.37505710353216,1.42408445425791,1.44819072459155,1.453056224355,1.45577948855589,
1.45814098678398,1.46117492215529,1.46621819634657,1.50479408533015,1.56126770394926,
1.60279868470962,1.61125074238818,1.61607900129604,1.62027083121103,1.62543430950392,
1.63334342010044,1.67536297205957,1.73901509700709,1.75993072288712,1.77229137240521,
1.77621987335247,1.77873664981951,1.78114945965377,1.78413336161747,1.7915044553703,
1.85984085796907,1.90314070661222,1.92746935502212,1.93469420114988,1.93925460590421,
1.94350166857908,1.94904900641244,1.96141952355341,2.03130412200221),
 .UNSPECIFIED.);
#1201=B_SPLINE_CURVE_WITH_KNOTS('',3,(#11053,#11054,#11055,#11056,#11057,
#11058,#11059,#11060,#11061,#11062,#11063,#11064,#11065,#11066,#11067,#11068,
#11069,#11070,#11071,#11072,#11073,#11074,#11075,#11076,#11077,#11078,#11079,
#11080,#11081,#11082,#11083,#11084,#11085,#11086,#11087,#11088,#11089,#11090,
#11091,#11092,#11093,#11094,#11095,#11096,#11097,#11098,#11099,#11100,#11101,
#11102,#11103,#11104,#11105,#11106,#11107,#11108,#11109,#11110,#11111,#11112,
#11113,#11114,#11115,#11116,#11117,#11118,#11119,#11120,#11121,#11122,#11123,
#11124,#11125,#11126,#11127,#11128,#11129,#11130,#11131,#11132,#11133,#11134,
#11135,#11136,#11137,#11138,#11139,#11140,#11141,#11142,#11143,#11144,#11145,
#11146,#11147,#11148,#11149,#11150,#11151,#11152,#11153,#11154,#11155,#11156,
#11157,#11158,#11159,#11160,#11161,#11162,#11163,#11164,#11165,#11166,#11167,
#11168,#11169,#11170,#11171,#11172,#11173,#11174,#11175,#11176,#11177,#11178,
#11179,#11180,#11181,#11182,#11183,#11184,#11185,#11186,#11187,#11188,#11189,
#11190,#11191,#11192,#11193,#11194,#11195,#11196,#11197,#11198,#11199,#11200,
#11201,#11202,#11203,#11204,#11205,#11206,#11207,#11208,#11209,#11210,#11211,
#11212,#11213,#11214,#11215,#11216,#11217,#11218,#11219,#11220,#11221,#11222,
#11223,#11224,#11225,#11226,#11227,#11228,#11229,#11230,#11231,#11232,#11233,
#11234,#11235,#11236,#11237,#11238,#11239,#11240,#11241,#11242,#11243,#11244,
#11245,#11246,#11247,#11248,#11249,#11250,#11251,#11252,#11253,#11254,#11255,
#11256,#11257,#11258,#11259,#11260,#11261,#11262,#11263,#11264,#11265,#11266,
#11267,#11268,#11269,#11270,#11271,#11272,#11273,#11274,#11275,#11276,#11277,
#11278,#11279,#11280,#11281,#11282,#11283,#11284,#11285,#11286,#11287,#11288,
#11289,#11290,#11291,#11292),.UNSPECIFIED.,.F.,.F.,(4,2,2,2,2,2,2,2,2,2,
2,2,2,2,2,2,2,2,2,2,2,2,2,2,2,2,2,2,2,2,2,2,2,2,2,2,2,2,2,2,2,2,2,2,2,2,
2,2,2,2,2,2,2,2,2,2,2,2,2,2,2,2,2,2,2,2,2,2,2,2,2,2,2,2,2,2,2,2,2,2,2,2,
2,2,2,2,2,2,2,2,2,2,2,2,2,2,2,2,2,2,2,2,2,2,2,2,2,2,2,2,2,2,2,2,2,2,2,2,
2,4),(0.00124959457603072,0.00492543247451525,0.0116818150862804,0.0377034604979688,
0.114471961733272,0.135439625127425,0.14376941206842,0.150013273990401,
0.153020890359151,0.155375465320991,0.158152271004239,0.163125656412322,
0.186235736995255,0.193494712808228,0.221420716211356,0.274843012937881,
0.293078382164194,0.306293226992382,0.311840961930181,0.311988334968319,
0.312135099985741,0.312281944293211,0.31242960352371,0.312578881378219,
0.312730674935975,0.312886007992206,0.313046076134992,0.313212309449408,
0.313386462370007,0.313570746834712,0.313661175647747,0.313791566679259,
0.313990742769881,0.317857527833423,0.322759921545408,0.331593068575246,
0.379990737876284,0.44455792119756,0.468410828991787,0.473262591831226,
0.475982894394741,0.478344913456056,0.481383408228347,0.486442256031224,
0.535421646772217,0.566639068530259,0.617071005605761,0.629176502670673,
0.634736499732904,0.638971294402423,0.643568014306446,0.650958642964771,
0.67444457057856,0.770475177984643,0.784348615058876,0.793552960890251,
0.797066440625881,0.799495953831366,0.801724041088134,0.805454421680962,
0.815373917829648,0.918700270757783,0.937573655740761,0.951139134054692,
0.956955364302162,0.961230093736521,0.965726515877643,0.972656666995343,
0.992361705031603,1.09281642674985,1.10687367921614,1.11616783475831,1.11969447597409,
1.12212639910168,1.12435135276931,1.12745382685068,1.13555124869866,1.18618535191786,
1.23070715505844,1.26849478271473,1.27674958652149,1.28153518284876,1.28573139859682,
1.29095410627343,1.29905716419411,1.34635659010491,1.41188863489402,1.43589232881538,
1.4407524741973,1.44347466216422,1.4458364755782,1.44887237338436,1.45392209825609,
1.49290057670856,1.50954595970559,1.55565038421919,1.5911142191012,1.59923018326806,
1.60398568942568,1.60818592485367,1.61345384759458,1.62170564350074,1.68305717564142,
1.72689190888643,1.75771603732155,1.76288353189489,1.76567187486503,1.76802565509607,
1.77101877603656,1.77581516977206,1.80424916536834,1.85887737188161,1.90342876299138,
1.91796652879128,1.92394369465665,1.92824742385816,1.93217256159791,1.93744941525408,
1.95037299426595,2.03151358947421),.UNSPECIFIED.);
#1202=B_SPLINE_CURVE_WITH_KNOTS('',3,(#11297,#11298,#11299,#11300,#11301,
#11302,#11303,#11304,#11305,#11306,#11307,#11308,#11309,#11310,#11311,#11312,
#11313,#11314,#11315,#11316,#11317,#11318,#11319,#11320,#11321,#11322,#11323,
#11324,#11325,#11326,#11327,#11328,#11329,#11330,#11331,#11332,#11333,#11334,
#11335,#11336,#11337,#11338,#11339,#11340,#11341,#11342,#11343,#11344,#11345,
#11346,#11347,#11348,#11349,#11350,#11351,#11352,#11353,#11354,#11355,#11356,
#11357,#11358,#11359,#11360,#11361,#11362,#11363,#11364,#11365,#11366,#11367,
#11368,#11369,#11370,#11371,#11372,#11373,#11374,#11375,#11376,#11377,#11378,
#11379,#11380,#11381,#11382,#11383,#11384,#11385,#11386,#11387,#11388,#11389,
#11390,#11391,#11392,#11393,#11394,#11395,#11396,#11397,#11398,#11399,#11400,
#11401,#11402,#11403,#11404,#11405,#11406,#11407,#11408,#11409,#11410,#11411,
#11412,#11413,#11414,#11415,#11416,#11417,#11418,#11419,#11420,#11421,#11422,
#11423,#11424,#11425,#11426,#11427,#11428,#11429,#11430,#11431,#11432,#11433,
#11434,#11435,#11436,#11437,#11438,#11439,#11440,#11441,#11442,#11443,#11444,
#11445,#11446,#11447,#11448,#11449,#11450,#11451,#11452,#11453,#11454,#11455,
#11456,#11457,#11458,#11459,#11460,#11461,#11462,#11463,#11464,#11465,#11466,
#11467,#11468,#11469,#11470,#11471,#11472,#11473,#11474,#11475,#11476,#11477,
#11478,#11479,#11480,#11481,#11482,#11483,#11484,#11485,#11486,#11487,#11488,
#11489,#11490,#11491,#11492,#11493,#11494,#11495,#11496,#11497,#11498,#11499,
#11500,#11501,#11502,#11503,#11504,#11505,#11506,#11507,#11508,#11509,#11510,
#11511,#11512,#11513,#11514,#11515,#11516),.UNSPECIFIED.,.F.,.F.,(4,2,2,
2,2,2,2,2,2,2,2,2,2,2,2,2,2,2,2,2,2,2,2,2,2,2,2,2,2,2,2,2,2,2,2,2,2,2,2,
2,2,2,2,2,2,2,2,2,2,2,2,2,2,2,2,2,2,2,2,2,2,2,2,2,2,2,2,2,2,2,2,2,2,2,2,
2,2,2,2,2,2,2,2,2,2,2,2,2,2,2,2,2,2,2,2,2,2,2,2,2,2,2,2,2,2,2,2,2,2,4),
(2.03073768813154,2.11072975512029,2.12234333454239,2.12775320390847,2.13197944191807,
2.136602429535,2.14411497645868,2.17150650529066,2.22440946936597,2.27841097866719,
2.28647353178428,2.28957086092473,2.29179425912932,2.29422696006808,2.29775889429554,
2.30709091128042,2.32122821912819,2.42377002578307,2.44178602378642,2.44847921611095,
2.45248021059465,2.45672809294067,2.46238351711885,2.47502514037414,2.49223477848027,
2.54044248844621,2.54664704473423,2.60074121370944,2.60883564648511,2.61193696324897,
2.61416112680092,2.61659222238102,2.62011776362682,2.6294094896026,2.64346521996227,
2.74389551145599,2.7636108902075,2.77054072289667,2.77503590122977,2.77930870117297,
2.78512114230213,2.79867252370822,2.81752042894719,2.92052646222894,2.93061782703941,
2.93437258328928,2.93660467497578,2.93902868209343,2.94251798554393,2.95156812592516,
2.96513276971133,3.01140327684648,3.07648032594718,3.08776076166595,3.0938904673702,
3.09817824927165,3.10257549351041,3.10903838043567,3.12687129045731,3.15418090070068,
3.20979388129932,3.24941162964769,3.25446822808309,3.25750549108827,3.25986662399677,
3.26258597571072,3.26743628011954,3.29128495022569,3.35584900595195,3.40420923089798,
3.41234396785359,3.41757507662633,3.42177034105811,3.42654651884582,3.43476398690763,
3.47195577295523,3.5168166377711,3.56762680974727,3.57571799429181,3.57881866410196,
3.58104251271806,3.58347343761378,3.58699901986224,3.5962925126977,3.61035237130263,
3.71091566817458,3.73051012943634,3.73728664320116,3.74171521995412,3.74573931209866,
3.74602017566641,3.74631065043745,3.74661625993346,3.74694250778996,3.7533028847529,
3.77040267249736,3.7961692600928,3.83979136985615,3.88987827349401,3.89797329345074,
3.90107409025273,3.90329769576141,3.90572796582772,3.90925195165624,3.91853751959072,
3.9325821291337,4.03280542314696,4.05202382614655,4.05720470954994,4.06024052944633),
 .UNSPECIFIED.);
#1203=B_SPLINE_CURVE_WITH_KNOTS('',3,(#11518,#11519,#11520,#11521,#11522,
#11523,#11524,#11525,#11526,#11527,#11528,#11529,#11530,#11531,#11532,#11533,
#11534,#11535,#11536,#11537,#11538,#11539,#11540,#11541,#11542,#11543,#11544,
#11545,#11546,#11547,#11548,#11549,#11550,#11551,#11552,#11553,#11554,#11555,
#11556,#11557,#11558,#11559,#11560,#11561,#11562,#11563,#11564,#11565,#11566,
#11567,#11568,#11569,#11570,#11571,#11572,#11573,#11574,#11575,#11576,#11577,
#11578,#11579,#11580,#11581,#11582,#11583,#11584,#11585,#11586,#11587,#11588,
#11589,#11590,#11591,#11592,#11593,#11594,#11595,#11596,#11597,#11598,#11599,
#11600,#11601,#11602,#11603,#11604,#11605,#11606,#11607,#11608,#11609,#11610,
#11611,#11612,#11613,#11614,#11615,#11616,#11617,#11618,#11619,#11620,#11621,
#11622,#11623,#11624,#11625,#11626,#11627,#11628,#11629,#11630,#11631,#11632,
#11633,#11634,#11635,#11636,#11637,#11638,#11639,#11640,#11641,#11642,#11643,
#11644,#11645,#11646,#11647,#11648,#11649,#11650,#11651,#11652,#11653,#11654,
#11655,#11656,#11657,#11658,#11659,#11660,#11661,#11662,#11663,#11664,#11665,
#11666,#11667,#11668,#11669,#11670,#11671,#11672,#11673,#11674,#11675,#11676,
#11677,#11678,#11679,#11680,#11681,#11682,#11683,#11684,#11685,#11686,#11687,
#11688,#11689,#11690,#11691,#11692,#11693,#11694,#11695,#11696,#11697,#11698,
#11699,#11700,#11701,#11702,#11703,#11704,#11705,#11706,#11707,#11708,#11709,
#11710,#11711,#11712,#11713,#11714,#11715,#11716,#11717,#11718,#11719,#11720,
#11721,#11722,#11723,#11724,#11725,#11726,#11727,#11728,#11729,#11730,#11731,
#11732,#11733,#11734,#11735,#11736,#11737,#11738,#11739,#11740,#11741,#11742,
#11743,#11744,#11745),.UNSPECIFIED.,.F.,.F.,(4,2,2,2,2,2,2,2,2,2,2,2,2,
2,2,2,2,2,2,2,2,2,2,2,2,2,2,2,2,2,2,2,2,2,2,2,2,2,2,2,2,2,2,2,2,2,2,2,2,
2,2,2,2,2,2,2,2,2,2,2,2,2,2,2,2,2,2,2,2,2,2,2,2,2,2,2,2,2,2,2,2,2,2,2,2,
2,2,2,2,2,2,2,2,2,2,2,2,2,2,2,2,2,2,2,2,2,2,2,2,2,2,2,2,4),(2.03151358947421,
2.03179279629966,2.07934242230676,2.08493183850827,2.08784507076267,2.09019551517515,
2.09305203002042,2.0985432905786,2.14174761963465,2.21047983714227,2.2367551795405,
2.24445258535579,2.24911666327236,2.25333360557995,2.25875694838213,2.27012733002251,
2.31454045187498,2.3733550174524,2.3835803675052,2.40320846220856,2.40794896053077,
2.41067301154721,2.41279787424561,2.41575331764715,2.42173113411769,2.45341399541341,
2.5223699682621,2.52421233111449,2.55797513019204,2.56619990527858,2.57102649160007,
2.57521878205303,2.58038526940911,2.59044747216621,2.6032853402125,2.63349537403812,
2.67269619515577,2.69798114073147,2.72477341442969,2.72950142514258,2.7324738966228,
2.73482633783964,2.73763078196616,2.74287455373235,2.77589984591938,2.84495539878062,
2.8801411781844,2.88845761097629,2.89330483261521,2.89749512882616,2.90263384752023,
2.91256073392481,2.92518022432155,2.95462430648263,2.99446680045347,3.01917949875696,
3.04701462729239,3.05178593330778,3.05477132472137,3.05712433871354,3.05991804051801,
3.06511179797319,3.09667169775675,3.16265954969188,3.20200902523218,3.21056557897601,
3.21546702999504,3.21961386608028,3.22466827030457,3.23418681047777,3.30184721346629,
3.36547964700241,3.37316439571593,3.37620158875579,3.37840953731662,3.38085822139737,
3.38446915809363,3.39434737263569,3.45802040604519,3.51816343832614,3.53073345281895,
3.53631587068988,3.54056837177271,3.5451138522323,3.55227091686359,3.57593861676319,
3.61737549323501,3.68243986239268,3.69416704299009,3.69815523259854,3.70043354833431,
3.70277939126246,3.70596798518041,3.70960262062157,3.71594266015058,3.73001422510341,
3.83076929402906,3.85025218777052,3.85715208789866,3.86164152914446,3.86591879301661,
3.87175295172683,3.88542826978344,3.90450174863351,3.97648544401523,3.99690977804572,
4.015266653672,4.01989911977734,4.02259783855968,4.02490759915752,4.02722459528333,
4.0302635598406,4.03511993261798,4.06121199284332),.UNSPECIFIED.);
#1204=B_SPLINE_CURVE_WITH_KNOTS('',3,(#11746,#11747,#11748,#11749),
 .UNSPECIFIED.,.F.,.F.,(4,4),(0.00115314525638064,0.00134934797194002),
 .UNSPECIFIED.);
#1205=B_SPLINE_CURVE_WITH_KNOTS('',3,(#11755,#11756,#11757,#11758),
 .UNSPECIFIED.,.F.,.F.,(4,4),(4.06070745563291,4.06091392182859),
 .UNSPECIFIED.);
#1206=B_SPLINE_CURVE_WITH_KNOTS('',3,(#11759,#11760,#11761,#11762,#11763,
#11764,#11765,#11766,#11767,#11768,#11769,#11770,#11771,#11772,#11773,#11774,
#11775,#11776,#11777,#11778,#11779,#11780,#11781,#11782,#11783,#11784,#11785,
#11786,#11787,#11788,#11789,#11790,#11791,#11792,#11793,#11794,#11795,#11796,
#11797,#11798,#11799,#11800,#11801,#11802,#11803,#11804,#11805,#11806,#11807,
#11808,#11809,#11810,#11811,#11812,#11813,#11814,#11815,#11816,#11817,#11818,
#11819,#11820,#11821,#11822,#11823,#11824,#11825,#11826,#11827,#11828,#11829,
#11830,#11831,#11832,#11833,#11834,#11835,#11836,#11837,#11838,#11839,#11840,
#11841,#11842,#11843,#11844,#11845,#11846,#11847,#11848,#11849,#11850,#11851,
#11852,#11853,#11854,#11855,#11856,#11857,#11858,#11859,#11860,#11861,#11862,
#11863,#11864,#11865,#11866,#11867,#11868,#11869,#11870,#11871,#11872,#11873,
#11874,#11875,#11876,#11877,#11878,#11879,#11880,#11881,#11882,#11883,#11884,
#11885,#11886,#11887,#11888,#11889,#11890,#11891,#11892,#11893,#11894,#11895,
#11896,#11897,#11898,#11899,#11900,#11901,#11902,#11903,#11904,#11905,#11906,
#11907,#11908,#11909,#11910,#11911,#11912,#11913,#11914,#11915,#11916,#11917,
#11918,#11919,#11920,#11921,#11922,#11923,#11924,#11925,#11926,#11927,#11928,
#11929,#11930,#11931,#11932,#11933,#11934,#11935,#11936,#11937,#11938,#11939,
#11940,#11941,#11942,#11943,#11944,#11945,#11946,#11947,#11948,#11949,#11950,
#11951,#11952,#11953,#11954,#11955,#11956,#11957,#11958,#11959,#11960,#11961,
#11962,#11963,#11964,#11965,#11966,#11967,#11968,#11969,#11970,#11971,#11972,
#11973,#11974,#11975,#11976,#11977,#11978,#11979,#11980,#11981,#11982,#11983,
#11984,#11985,#11986,#11987,#11988,#11989,#11990,#11991,#11992,#11993,#11994,
#11995,#11996,#11997,#11998,#11999,#12000,#12001,#12002,#12003,#12004,#12005,
#12006,#12007,#12008,#12009,#12010,#12011,#12012,#12013,#12014,#12015,#12016,
#12017,#12018,#12019,#12020,#12021,#12022,#12023,#12024,#12025,#12026,#12027,
#12028,#12029,#12030,#12031,#12032,#12033,#12034,#12035,#12036,#12037,#12038,
#12039,#12040,#12041,#12042,#12043,#12044,#12045,#12046,#12047,#12048,#12049,
#12050,#12051,#12052,#12053,#12054,#12055,#12056,#12057,#12058,#12059,#12060,
#12061,#12062,#12063,#12064,#12065,#12066,#12067,#12068,#12069,#12070,#12071,
#12072,#12073,#12074,#12075,#12076),.UNSPECIFIED.,.F.,.F.,(4,2,2,2,2,2,
2,2,2,2,2,2,2,2,2,2,2,2,2,2,2,2,2,2,2,2,2,2,2,2,2,2,2,2,2,2,2,2,2,2,2,2,
2,2,2,2,2,2,2,2,2,2,2,2,2,2,2,2,2,2,2,2,2,2,2,2,2,2,2,2,2,2,2,2,2,2,2,2,
2,2,2,2,2,2,2,2,2,2,2,2,2,2,2,2,2,2,2,2,2,2,2,2,2,2,2,2,2,2,2,2,2,2,2,2,
2,2,2,2,2,2,2,2,2,2,2,2,2,2,2,2,2,2,2,2,2,2,2,2,2,2,2,2,2,2,2,2,2,2,2,2,
2,2,2,2,2,2,2,2,4),(0.0011683366425719,0.0190896020491265,0.0283003389842762,
0.0314305038094561,0.0337794422462348,0.0360500179959316,0.03867520572741,
0.0430940587683594,0.0584996142433649,0.0781669975701139,0.144699861170873,
0.182131045967224,0.190364861544194,0.195145680566725,0.199342117590731,
0.204570882354306,0.212694534858354,0.26063603369651,0.340144243133286,
0.347825600067614,0.353637852873017,0.356547027409714,0.356556090594668,
0.356565251946185,0.356574512743948,0.356583874305357,0.356593337926219,
0.35660290494184,0.356612576718678,0.3566223546711,0.356632240186353,0.356642234676561,
0.356652339593405,0.356662556402393,0.356672886621523,0.356683331769095,
0.356693893376627,0.356704573011764,0.356715372269769,0.356726292743829,
0.356737336103744,0.356748504013963,0.356759798167156,0.356771220283469,
0.356782772095619,0.356794455395882,0.356806271966298,0.356818223651303,
0.356830312311093,0.356842539837938,0.356854908156969,0.356867419181249,
0.356880074908092,0.356892877369787,0.356905828591294,0.356918930631532,
0.356932185603303,0.356945595658919,0.356959162951516,0.356972889719226,
0.356986778198209,0.35700083064486,0.357015049370485,0.357029436715151,
0.357043995074483,0.357058726855779,0.357073634520072,0.357087567614488,
0.359449163843749,0.362483776215833,0.367529307757795,0.406352867542073,
0.462663543957239,0.490124566921263,0.502165718298953,0.511730999589201,
0.516795422044643,0.520943042183884,0.525836723338703,0.534357590478075,
0.573013838138699,0.63953096591555,0.671241181096845,0.676440275088906,
0.679235254969947,0.68158838521942,0.684572744869096,0.689340250253382,
0.717071548480294,0.74191579905805,0.781769880483295,0.811238141615489,
0.82386421530927,0.833794630911215,0.838934314057546,0.843124970321952,
0.84797213668555,0.856287325214198,0.891281214684261,0.960360345705921,
0.993478224151555,0.998724916628295,1.00153007969029,1.00388262013799,1.00685461880762,
1.01158082515537,1.03826646163187,1.12385642139954,1.15067895566725,1.15814142597914,
1.1627537517932,1.1669835887318,1.1724165478094,1.18415374005488,1.26322890060629,
1.29963058690042,1.3114664199087,1.3196402330663,1.32299244914599,1.32539203415961,
1.32766038047844,1.33159744983048,1.34294460252838,1.40851258456327,1.44998298901275,
1.47366122691284,1.48081977160036,1.48536579390186,1.48961852692549,1.49520085480276,
1.50776909209673,1.56807797856574,1.63153210129232,1.64139638053063,1.64500543149153,
1.64745381621774,1.64966225972668,1.6527011527735,1.66039551518431,1.72382918450427,
1.79172218512908,1.80124302074416,1.80629796889047,1.81044490924899,1.81534609060657,
1.82390118518987,1.86322967892115,1.92917909746166,1.95050083483856,1.95892428125475,
1.96522257041947,1.96824067357641,1.97059594373311,1.97336479316313,1.9783032936595,
2.0008347999481,2.00595072121192,2.03046255456567,2.03073768813154),
 .UNSPECIFIED.);
#1207=B_SPLINE_CURVE_WITH_KNOTS('',3,(#12077,#12078,#12079,#12080,#12081,
#12082,#12083,#12084,#12085,#12086,#12087,#12088,#12089,#12090,#12091,#12092,
#12093,#12094,#12095,#12096,#12097,#12098,#12099,#12100,#12101,#12102,#12103,
#12104,#12105,#12106,#12107,#12108,#12109,#12110,#12111,#12112,#12113,#12114,
#12115,#12116,#12117,#12118,#12119,#12120,#12121,#12122,#12123,#12124,#12125,
#12126,#12127,#12128,#12129,#12130,#12131,#12132,#12133,#12134,#12135,#12136,
#12137,#12138,#12139,#12140,#12141,#12142,#12143,#12144,#12145,#12146,#12147,
#12148,#12149,#12150,#12151,#12152,#12153,#12154,#12155,#12156,#12157,#12158,
#12159,#12160,#12161,#12162,#12163,#12164,#12165,#12166,#12167,#12168,#12169,
#12170,#12171,#12172,#12173,#12174,#12175,#12176,#12177,#12178,#12179,#12180,
#12181,#12182,#12183,#12184,#12185,#12186,#12187,#12188,#12189,#12190,#12191,
#12192,#12193,#12194,#12195,#12196,#12197,#12198,#12199,#12200,#12201,#12202,
#12203,#12204,#12205,#12206,#12207,#12208,#12209,#12210,#12211,#12212,#12213,
#12214,#12215,#12216,#12217,#12218,#12219,#12220,#12221,#12222,#12223,#12224,
#12225,#12226,#12227,#12228,#12229,#12230,#12231,#12232,#12233,#12234,#12235,
#12236,#12237,#12238,#12239,#12240,#12241,#12242,#12243,#12244,#12245,#12246,
#12247,#12248,#12249,#12250,#12251,#12252,#12253,#12254,#12255,#12256,#12257,
#12258,#12259,#12260,#12261,#12262,#12263,#12264,#12265,#12266,#12267,#12268,
#12269,#12270,#12271,#12272,#12273,#12274,#12275,#12276,#12277,#12278,#12279,
#12280,#12281,#12282,#12283,#12284,#12285,#12286,#12287,#12288),
 .UNSPECIFIED.,.F.,.F.,(4,2,2,2,2,2,2,2,2,2,2,2,2,2,2,2,2,2,2,2,2,2,2,2,
2,2,2,2,2,2,2,2,2,2,2,2,2,2,2,2,2,2,2,2,2,2,2,2,2,2,2,2,2,2,2,2,2,2,2,2,
2,2,2,2,2,2,2,2,2,2,2,2,2,2,2,2,2,2,2,2,2,2,2,2,2,2,2,2,2,2,2,2,2,2,2,2,
2,2,2,2,2,2,2,2,2,4),(0.00134934797194002,0.0473229576046848,0.0884279385639762,
0.111973379278365,0.119117812896877,0.123660543946948,0.12791414356444,
0.133503334842215,0.146112060610572,0.207310082891032,0.253587591268638,
0.269425402852969,0.276306795270276,0.280152369345684,0.283419464021521,
0.285802081023537,0.288027161629884,0.291130856559744,0.299239359548236,
0.348635487090537,0.396302272346622,0.432338649785541,0.440489056114836,
0.445251522061218,0.449449929275014,0.454704996760686,0.462915983169359,
0.527049013724587,0.578372956499178,0.592699642405142,0.602124597077341,
0.605670215129057,0.608105640788178,0.610326186133742,0.614019057283122,
0.623687729027518,0.727297067802172,0.746178682778632,0.759747888110035,
0.7655639122917,0.769837827112304,0.774332789110485,0.78125946676895,0.800945943482425,
0.901393568363701,0.915448136692731,0.924740405160243,0.928266256754718,
0.930697612106519,0.932922027750942,0.936023727307062,0.944118945279267,
0.994911647752351,1.03970809255952,1.07707492367711,1.08530408200541,1.09008339212788,
1.0942792113274,1.09950812576685,1.10763377327201,1.15566687551174,1.2205057997157,
1.23651230161904,1.24673330847152,1.25039158276503,1.25284980801153,1.25504897094317,
1.25805208327741,1.26553695239642,1.3326489107978,1.37668430654995,1.4012668318682,
1.40851608814383,1.41308118086029,1.41732524892068,1.42285812571963,1.43515133050792,
1.50696829250819,1.54822468315412,1.560953429463,1.56958567336523,1.57301080261353,
1.57542293533072,1.57767078127043,1.58150556451832,1.59212474990427,1.69454598316592,
1.71337563602228,1.72691605468796,1.73272680255419,1.73699943990992,1.74149542539934,
1.74842848287844,1.76816724739095,1.86853746743152,1.88258784581406,1.89187778603315,
1.89540304348089,1.8978340805981,1.90005827810948,1.90315976908588,1.91125516024819,
1.9616825875539,2.0058667471811,2.0311634453307,2.03132451219564),
 .UNSPECIFIED.);
#1208=B_SPLINE_CURVE_WITH_KNOTS('',3,(#12294,#12295,#12296,#12297),
 .UNSPECIFIED.,.F.,.F.,(4,4),(4.06083740610103,4.06111488809983),
 .UNSPECIFIED.);
#1209=B_SPLINE_CURVE_WITH_KNOTS('',3,(#12299,#12300,#12301,#12302,#12303,
#12304,#12305,#12306,#12307,#12308,#12309,#12310,#12311,#12312,#12313,#12314,
#12315,#12316,#12317,#12318,#12319,#12320,#12321,#12322,#12323,#12324,#12325,
#12326,#12327,#12328,#12329,#12330,#12331,#12332,#12333,#12334,#12335,#12336,
#12337,#12338,#12339,#12340,#12341,#12342,#12343,#12344,#12345,#12346,#12347,
#12348,#12349,#12350,#12351,#12352,#12353,#12354,#12355,#12356,#12357,#12358,
#12359,#12360,#12361,#12362,#12363,#12364,#12365,#12366,#12367,#12368,#12369,
#12370,#12371,#12372,#12373,#12374,#12375,#12376,#12377,#12378,#12379,#12380,
#12381,#12382,#12383,#12384,#12385,#12386,#12387,#12388,#12389,#12390,#12391,
#12392,#12393,#12394,#12395,#12396,#12397,#12398,#12399,#12400,#12401,#12402,
#12403,#12404,#12405,#12406,#12407,#12408,#12409,#12410,#12411,#12412,#12413,
#12414,#12415,#12416,#12417,#12418,#12419,#12420,#12421,#12422,#12423,#12424,
#12425,#12426,#12427,#12428,#12429,#12430,#12431,#12432,#12433,#12434,#12435,
#12436,#12437,#12438,#12439,#12440,#12441,#12442,#12443,#12444,#12445,#12446,
#12447,#12448,#12449,#12450,#12451,#12452,#12453,#12454,#12455,#12456,#12457,
#12458,#12459,#12460,#12461,#12462,#12463,#12464,#12465,#12466,#12467,#12468,
#12469,#12470,#12471,#12472,#12473,#12474,#12475,#12476,#12477,#12478,#12479,
#12480,#12481,#12482,#12483,#12484,#12485,#12486,#12487,#12488,#12489,#12490,
#12491,#12492,#12493,#12494),.UNSPECIFIED.,.F.,.F.,(4,2,2,2,2,2,2,2,2,2,
2,2,2,2,2,2,2,2,2,2,2,2,2,2,2,2,2,2,2,2,2,2,2,2,2,2,2,2,2,2,2,2,2,2,2,2,
2,2,2,2,2,2,2,2,2,2,2,2,2,2,2,2,2,2,2,2,2,2,2,2,2,2,2,2,2,2,2,2,2,2,2,2,
2,2,2,2,2,2,2,2,2,2,2,2,2,2,2,4),(0.00105193336829144,0.074271434275133,
0.0828669383037076,0.0892649539556792,0.0923023120117424,0.0946591793586463,
0.0974142605159078,0.102291905373549,0.123895849262207,0.134072461991593,
0.185084519971552,0.221242007588178,0.242839577362775,0.249508341103851,
0.253449005727344,0.257648024539186,0.262907018089082,0.271130323091447,
0.333385818722025,0.386221732369265,0.400761692043544,0.410289940472626,
0.413850784359742,0.416289363818054,0.418507008444209,0.422184054678848,
0.43174767616498,0.53549632692033,0.554384637010092,0.567957724552597,0.573774647016554,
0.578048940536365,0.582544044867368,0.589470423091558,0.609152366496295,
0.709613996600506,0.723669807503864,0.732962849858252,0.736488963911017,
0.738920490389783,0.741145054737096,0.744246951342368,0.752342606342695,
0.803194090118001,0.848093780819342,0.885322932162282,0.893544496917441,
0.898322360808603,0.902518679749868,0.907750537846343,0.915885255553501,
0.964193141839613,1.02879071133128,1.05264659624483,1.05749805548636,1.06021807237497,
1.06257976767387,1.06561775005651,1.07067554718112,1.11026134068559,1.16597776442856,
1.1933190804272,1.20532433836122,1.21486683467606,1.21992613151303,1.22407303455375,
1.22896993998142,1.23750676257852,1.27648312124341,1.34273525537125,1.37436349056789,
1.37955922301171,1.38235326889992,1.38470613002344,1.38769078361802,1.39245993338831,
1.42024115869083,1.4450439541917,1.48492594308059,1.51436799222037,1.52698614878675,
1.53691140947995,1.54204963767549,1.54623969913531,1.55108683376348,1.55940357334363,
1.59460323965626,1.66361222672057,1.69659629369557,1.70183815578237,1.70464207579407,
1.70699436215234,1.70996701612311,1.71469605882798,1.74151342011804,1.76673937606761,
1.82401017269133,1.84306999215748),.UNSPECIFIED.);
#1210=B_SPLINE_CURVE_WITH_KNOTS('',3,(#12496,#12497,#12498,#12499,#12500,
#12501),.UNSPECIFIED.,.F.,.F.,(4,2,4),(0.320887946935547,0.378623714396801,
0.396029912319007),.UNSPECIFIED.);
#1211=B_SPLINE_CURVE_WITH_KNOTS('',3,(#12502,#12503,#12504,#12505,#12506,
#12507,#12508,#12509,#12510,#12511,#12512,#12513,#12514,#12515,#12516,#12517,
#12518,#12519,#12520,#12521,#12522,#12523,#12524,#12525,#12526,#12527,#12528,
#12529,#12530,#12531,#12532,#12533,#12534,#12535,#12536,#12537,#12538,#12539,
#12540,#12541,#12542,#12543,#12544,#12545,#12546,#12547,#12548,#12549,#12550,
#12551,#12552,#12553,#12554,#12555,#12556,#12557,#12558,#12559,#12560,#12561,
#12562,#12563,#12564,#12565,#12566,#12567,#12568,#12569,#12570,#12571,#12572,
#12573,#12574,#12575,#12576,#12577,#12578,#12579,#12580,#12581,#12582,#12583,
#12584,#12585,#12586,#12587,#12588,#12589,#12590,#12591,#12592,#12593,#12594,
#12595,#12596,#12597,#12598,#12599,#12600,#12601,#12602,#12603,#12604,#12605,
#12606,#12607,#12608,#12609,#12610,#12611,#12612,#12613,#12614,#12615,#12616,
#12617,#12618,#12619,#12620,#12621,#12622,#12623,#12624,#12625,#12626,#12627,
#12628,#12629,#12630,#12631,#12632,#12633,#12634,#12635,#12636,#12637,#12638,
#12639,#12640,#12641,#12642,#12643,#12644,#12645,#12646,#12647,#12648,#12649,
#12650,#12651,#12652,#12653,#12654,#12655,#12656,#12657,#12658,#12659,#12660,
#12661,#12662,#12663,#12664,#12665,#12666,#12667,#12668,#12669,#12670,#12671,
#12672,#12673,#12674,#12675,#12676,#12677,#12678,#12679,#12680,#12681,#12682,
#12683,#12684,#12685,#12686,#12687,#12688,#12689,#12690,#12691,#12692,#12693,
#12694,#12695,#12696,#12697,#12698,#12699,#12700,#12701,#12702,#12703,#12704,
#12705,#12706,#12707,#12708,#12709,#12710,#12711,#12712,#12713,#12714,#12715,
#12716,#12717,#12718,#12719,#12720,#12721,#12722,#12723,#12724,#12725,#12726,
#12727,#12728,#12729,#12730,#12731,#12732,#12733,#12734,#12735,#12736,#12737,
#12738,#12739,#12740,#12741,#12742,#12743,#12744,#12745),.UNSPECIFIED.,
 .F.,.F.,(4,2,2,2,2,2,2,2,2,2,2,2,2,2,2,2,2,2,2,2,2,2,2,2,2,2,2,2,2,2,2,
2,2,2,2,2,2,2,2,2,2,2,2,2,2,2,2,2,2,2,2,2,2,2,2,2,2,2,2,2,2,2,2,2,2,2,2,
2,2,2,2,2,2,2,2,2,2,2,2,2,2,2,2,2,2,2,2,2,2,2,2,2,2,2,2,2,2,2,2,2,2,2,2,
2,2,2,2,2,2,2,2,2,2,2,2,2,2,2,2,2,2,4),(0.112200587611434,0.117175410522727,
0.152928885655975,0.182368339026361,0.21521303229137,0.222288891030475,
0.225452486921332,0.227823212755877,0.230500246255892,0.235154078995901,
0.253105054356244,0.271276271681732,0.330837168835884,0.358965543661657,
0.371203219709213,0.380802311059297,0.385849987467527,0.385885864854495,
0.385924240245527,0.385965296738259,0.386009231980911,0.38605625943733,
0.386106609776702,0.386160532405191,0.386218297123432,0.386280195938184,
0.38634654503799,0.386417686918759,0.386493992700438,0.386575864618516,
0.386663738676338,0.38675808745914,0.38682414110453,0.391023904951597,0.396289955575155,
0.404536323115612,0.467610196584102,0.519735038112093,0.534175511413127,
0.543655736077999,0.547209648218229,0.549646896227527,0.551866046008907,
0.555550783543033,0.565164220475125,0.668704244943297,0.687664391154196,
0.701276728938032,0.707100380253507,0.711375927596264,0.71586900356524,
0.722785494212219,0.742391705638046,0.84293352866078,0.856991887461833,
0.866286185003037,0.86981254943419,0.872244181194704,0.874468800429131,
0.87757073386914,0.885666205273227,0.936422404891006,0.981159832924879,
1.01861025676021,1.0268447872605,1.03162556575424,1.0358216955753,1.04104972168781,
1.04917153804975,1.09706939478725,1.16202809251959,1.18593997382092,1.19079458878314,
1.19351534527639,1.19587701578634,1.19891414433071,1.20396883989234,1.24333621222392,
1.29921079114077,1.32658528985591,1.33860040646458,1.34814913730591,1.3532098253402,
1.35735691343316,1.3622529244792,1.37078537360544,1.40967598947049,1.47598956667862,
1.50763639647932,1.51283286572484,1.51562712244927,1.51798005664305,1.52096469302807,
1.52573362273362,1.5535080962,1.57831182100707,1.61818755394369,1.64762955939873,
1.66024770207484,1.67017299312081,1.67531132566215,1.67950152330356,1.68434887857098,
1.69266617114479,1.72787307314038,1.79686729467227,1.82984558844559,1.83508734395831,
1.83789129580703,1.84024366822052,1.84321652918665,1.84794609616524,1.87477440902351,
1.89996443843373,1.95724441004869,1.97662465914178,1.99046610892694,1.99632899760937,
2.00061207621772,2.00509388709481,2.01195454307251,2.03100183139203),
 .UNSPECIFIED.);
#1212=B_SPLINE_CURVE_WITH_KNOTS('',3,(#12749,#12750,#12751,#12752,#12753,
#12754,#12755,#12756),.UNSPECIFIED.,.F.,.F.,(4,2,2,4),(-0.0831448232791332,
-0.0490560578977458,-0.00142471500823912,-0.000102382691227175),
 .UNSPECIFIED.);
#1213=B_SPLINE_CURVE_WITH_KNOTS('',3,(#12760,#12761,#12762,#12763,#12764,
#12765),.UNSPECIFIED.,.F.,.F.,(4,2,4),(-0.0960086291905594,-0.0470065127227869,
-0.0454387767918283),.UNSPECIFIED.);
#1214=B_SPLINE_CURVE_WITH_KNOTS('',3,(#12769,#12770,#12771,#12772,#12773,
#12774),.UNSPECIFIED.,.F.,.F.,(4,2,4),(-0.0932727713439407,-0.047751044771726,
-0.00126085793865929),.UNSPECIFIED.);
#1215=B_SPLINE_CURVE_WITH_KNOTS('',3,(#12778,#12779,#12780,#12781,#12782,
#12783),.UNSPECIFIED.,.F.,.F.,(4,2,4),(-0.0950156675258279,-0.0473137239138524,
-0.000590793973779404),.UNSPECIFIED.);
#1216=B_SPLINE_CURVE_WITH_KNOTS('',3,(#12787,#12788,#12789,#12790,#12791,
#12792),.UNSPECIFIED.,.F.,.F.,(4,2,4),(-0.0929898096602351,-0.0473375247997017,
-0.00112505768103942),.UNSPECIFIED.);
#1217=B_SPLINE_CURVE_WITH_KNOTS('',3,(#12796,#12797,#12798,#12799,#12800,
#12801),.UNSPECIFIED.,.F.,.F.,(4,2,4),(-0.0942916337962443,-0.0469654289747836,
-0.000383531894571019),.UNSPECIFIED.);
#1218=B_SPLINE_CURVE_WITH_KNOTS('',3,(#12805,#12806,#12807,#12808,#12809,
#12810),.UNSPECIFIED.,.F.,.F.,(4,2,4),(-0.0930000698261243,-0.0474064095804956,
-2.37639472703122E-5),.UNSPECIFIED.);
#1219=B_SPLINE_CURVE_WITH_KNOTS('',3,(#12814,#12815,#12816,#12817,#12818,
#12819),.UNSPECIFIED.,.F.,.F.,(4,2,4),(-0.0938672630693478,-0.0468733216732729,
-0.00100573708691378),.UNSPECIFIED.);
#1220=B_SPLINE_CURVE_WITH_KNOTS('',3,(#12823,#12824,#12825,#12826),
 .UNSPECIFIED.,.F.,.F.,(4,4),(-0.0936312282255871,-0.0913169723171845),
 .UNSPECIFIED.);
#1221=B_SPLINE_CURVE_WITH_KNOTS('',3,(#12830,#12831,#12832,#12833,#12834,
#12835,#12836,#12837),.UNSPECIFIED.,.F.,.F.,(4,2,2,4),(-0.0958223528200869,
-0.0488517447323541,-0.00155186802867582,-0.000922707505804365),
 .UNSPECIFIED.);
#1222=B_SPLINE_CURVE_WITH_KNOTS('',3,(#12841,#12842,#12843,#12844,#12845,
#12846),.UNSPECIFIED.,.F.,.F.,(4,2,4),(-0.0931685739517461,-0.0489870992666756,
-0.00144168232493454),.UNSPECIFIED.);
#1223=B_SPLINE_CURVE_WITH_KNOTS('',3,(#12850,#12851,#12852,#12853,#12854,
#12855,#12856,#12857),.UNSPECIFIED.,.F.,.F.,(4,2,2,4),(-0.0945405801644211,
-0.0487921724313465,-0.00154988310282899,-0.00035365744226039),
 .UNSPECIFIED.);
#1224=B_SPLINE_CURVE_WITH_KNOTS('',3,(#12861,#12862,#12863,#12864,#12865,
#12866,#12867,#12868),.UNSPECIFIED.,.F.,.F.,(4,2,2,4),(-0.092843423921612,
-0.0486414832741236,-0.00140880394837164,-0.00070368441099022),
 .UNSPECIFIED.);
#1225=B_SPLINE_CURVE_WITH_KNOTS('',3,(#12872,#12873,#12874,#12875,#12876,
#12877,#12878,#12879),.UNSPECIFIED.,.F.,.F.,(4,2,2,4),(-0.0945127436503505,
-0.0484329844501563,-0.00154044317359045,-0.000351343130144288),
 .UNSPECIFIED.);
#1226=B_SPLINE_CURVE_WITH_KNOTS('',3,(#12883,#12884,#12885,#12886),
 .UNSPECIFIED.,.F.,.F.,(4,4),(-0.026106848360131,0.),.UNSPECIFIED.);
#1227=B_SPLINE_CURVE_WITH_KNOTS('',3,(#12888,#12889,#12890,#12891),
 .UNSPECIFIED.,.F.,.F.,(4,4),(0.984691230773821,1.02983398123988),
 .UNSPECIFIED.);
#1228=B_SPLINE_CURVE_WITH_KNOTS('',3,(#12893,#12894,#12895,#12896,#12897,
#12898,#12899,#12900),.UNSPECIFIED.,.F.,.F.,(4,2,2,4),(-0.0860848159738799,
-0.0428840848156451,-0.00102967768936712,-0.000703274869736634),
 .UNSPECIFIED.);
#1229=B_SPLINE_CURVE_WITH_KNOTS('',3,(#12902,#12903,#12904,#12905,#12906,
#12907),.UNSPECIFIED.,.F.,.F.,(4,2,4),(0.679792780811918,0.754908335318789,
0.769264950774119),.UNSPECIFIED.);
#1230=B_SPLINE_CURVE_WITH_KNOTS('',3,(#12908,#12909,#12910,#12911,#12912,
#12913,#12914,#12915,#12916,#12917,#12918,#12919,#12920,#12921,#12922,#12923,
#12924,#12925,#12926,#12927,#12928,#12929,#12930,#12931,#12932,#12933,#12934,
#12935,#12936,#12937,#12938,#12939,#12940,#12941,#12942,#12943,#12944,#12945,
#12946,#12947,#12948,#12949,#12950,#12951,#12952,#12953,#12954,#12955,#12956,
#12957,#12958,#12959,#12960,#12961,#12962,#12963),.UNSPECIFIED.,.F.,.F.,
(4,2,2,2,2,2,2,2,2,2,2,2,2,2,2,2,2,2,2,2,2,2,2,2,2,2,2,4),(-0.325036416517763,
-0.287179950509608,-0.236779639746712,-0.200445653912114,-0.181391465406389,
-0.177124007539468,-0.174887587830202,-0.174466868660744,-0.174240191480089,
-0.174070434879753,-0.173884176187582,-0.17361100981857,-0.172814926867466,
-0.172526825059135,-0.123766680032299,-0.117959327419192,-0.111861646552513,
-0.105409658342378,-0.0985371190589346,-0.0911704642285506,-0.0832352014871189,
-0.0746399665009568,-0.065281858464088,-0.0550395262469432,-0.0437673431195303,
-0.0312871771278163,-0.0173761699319152,-0.00212616365527593),
 .UNSPECIFIED.);
#1231=B_SPLINE_CURVE_WITH_KNOTS('',3,(#12965,#12966,#12967,#12968,#12969,
#12970),.UNSPECIFIED.,.F.,.F.,(4,2,4),(-0.0942580482856856,-0.0500230495864651,
-0.00152799126305741),.UNSPECIFIED.);
#1232=B_SPLINE_CURVE_WITH_KNOTS('',3,(#12972,#12973,#12974,#12975,#12976,
#12977),.UNSPECIFIED.,.F.,.F.,(4,2,4),(0.31497790761872,0.320913430649623,
0.353605235463099),.UNSPECIFIED.);
#1233=B_SPLINE_CURVE_WITH_KNOTS('',3,(#12978,#12979,#12980,#12981),
 .UNSPECIFIED.,.F.,.F.,(4,4),(-0.0867509478555809,-0.0011253459254421),
 .UNSPECIFIED.);
#1234=B_SPLINE_CURVE_WITH_KNOTS('',3,(#12984,#12985,#12986,#12987),
 .UNSPECIFIED.,.F.,.F.,(4,4),(0.,0.00543966212988572),.UNSPECIFIED.);
#1235=B_SPLINE_CURVE_WITH_KNOTS('',3,(#12989,#12990,#12991,#12992),
 .UNSPECIFIED.,.F.,.F.,(4,4),(0.,0.0146364967117825),.UNSPECIFIED.);
#1236=B_SPLINE_CURVE_WITH_KNOTS('',3,(#12996,#12997,#12998,#12999,#13000,
#13001,#13002,#13003,#13004,#13005,#13006,#13007,#13008,#13009,#13010,#13011,
#13012,#13013,#13014,#13015,#13016,#13017,#13018,#13019,#13020,#13021,#13022,
#13023,#13024,#13025,#13026,#13027,#13028,#13029,#13030,#13031,#13032,#13033,
#13034,#13035,#13036,#13037,#13038,#13039,#13040,#13041,#13042,#13043,#13044,
#13045,#13046,#13047,#13048,#13049,#13050,#13051,#13052,#13053,#13054,#13055,
#13056,#13057,#13058,#13059,#13060,#13061,#13062,#13063,#13064,#13065,#13066,
#13067,#13068,#13069,#13070,#13071,#13072,#13073,#13074,#13075,#13076,#13077,
#13078,#13079,#13080,#13081,#13082,#13083),.UNSPECIFIED.,.F.,.F.,(4,3,3,
3,3,3,3,3,3,3,3,3,3,3,3,3,3,3,3,3,3,3,3,3,3,3,3,3,3,4),(0.,0.0258260740408234,
0.0621538547068688,0.0989229457645657,0.135638978855683,0.14769608638293,
0.154010732384414,0.189902252988839,0.225722717925846,0.260776849486767,
0.288525653206241,0.294827662437031,0.300967317524399,0.335458380531023,
0.369020467026818,0.402151952636654,0.436300775758561,0.44111937264328,
0.474534957939434,0.508516755568951,0.542217627328803,0.567490167559029,
0.575924259490715,0.608982407913722,0.642836293227944,0.654907851897474,
0.664022037486317,0.695845847471868,0.726802774478787,0.744397949170613),
 .UNSPECIFIED.);
#1237=B_SPLINE_CURVE_WITH_KNOTS('',3,(#13086,#13087,#13088,#13089),
 .UNSPECIFIED.,.F.,.F.,(4,4),(0.720569046407016,0.741270768406323),
 .UNSPECIFIED.);
#1238=B_SPLINE_CURVE_WITH_KNOTS('',3,(#13092,#13093,#13094,#13095,#13096,
#13097,#13098,#13099,#13100,#13101,#13102,#13103,#13104,#13105,#13106,#13107,
#13108,#13109,#13110,#13111,#13112,#13113,#13114,#13115,#13116,#13117,#13118,
#13119,#13120,#13121,#13122,#13123,#13124,#13125,#13126,#13127,#13128,#13129,
#13130,#13131,#13132,#13133,#13134,#13135,#13136,#13137,#13138,#13139,#13140,
#13141,#13142,#13143,#13144,#13145,#13146,#13147,#13148,#13149,#13150,#13151,
#13152,#13153,#13154,#13155,#13156,#13157,#13158,#13159,#13160,#13161,#13162,
#13163,#13164,#13165,#13166,#13167,#13168,#13169,#13170,#13171,#13172,#13173,
#13174,#13175,#13176,#13177,#13178,#13179,#13180,#13181,#13182,#13183,#13184,
#13185,#13186,#13187,#13188,#13189,#13190,#13191,#13192,#13193,#13194,#13195,
#13196,#13197,#13198,#13199,#13200,#13201,#13202,#13203,#13204,#13205,#13206,
#13207,#13208,#13209,#13210,#13211,#13212,#13213,#13214,#13215,#13216,#13217,
#13218,#13219,#13220,#13221,#13222,#13223,#13224,#13225,#13226,#13227,#13228,
#13229,#13230,#13231,#13232,#13233,#13234,#13235,#13236,#13237,#13238,#13239,
#13240,#13241,#13242,#13243,#13244,#13245,#13246,#13247,#13248,#13249,#13250,
#13251,#13252,#13253,#13254,#13255,#13256,#13257,#13258,#13259,#13260,#13261,
#13262,#13263,#13264,#13265,#13266,#13267,#13268,#13269,#13270,#13271,#13272,
#13273,#13274,#13275,#13276,#13277,#13278,#13279,#13280,#13281,#13282,#13283,
#13284,#13285,#13286,#13287,#13288,#13289,#13290,#13291,#13292,#13293),
 .UNSPECIFIED.,.F.,.F.,(4,3,3,3,3,3,3,3,3,3,3,3,3,3,3,3,3,3,3,3,3,3,3,3,
3,3,3,3,3,3,3,3,3,3,3,3,3,3,3,3,3,3,3,3,3,3,3,3,3,3,3,3,3,3,3,3,3,3,3,3,
3,3,3,3,3,3,3,4),(-29.2254901136586,-29.1178016057759,-29.0085140011152,
-28.9376744100947,-28.8491012607996,-28.7606424677612,-28.6722742554,-28.5807179195209,
-28.4924512759753,-28.404197885369,-28.3159364031115,-28.2276454839452,
-28.1392544983622,-28.0508039100885,-27.9622239853604,-27.9398235683673,
-27.8512504190762,-27.7627916260421,-27.6744234136853,-27.5828670778046,
-27.4946004342638,-27.4063470436626,-27.3180855614104,-27.2297946422494,
-27.1414036566721,-27.052953068404,-26.9643731436818,-26.9419727266399,
-26.853399577259,-26.7649407841347,-26.6765725716875,-26.5850162358407,
-26.4967495922096,-26.4084962015182,-26.3202347191761,-26.2319437999256,
-26.1435528142598,-26.0551022259036,-25.9665223010947,-25.9441218849125,
-25.8555487357036,-25.7670899427513,-25.6787217304758,-25.5871653945645,
-25.4988987511032,-25.4106453605806,-25.3223838784063,-25.2340929593222,
-25.1457019738199,-25.057251385626,-24.9686714609759,-24.9462710431851,
-24.8576978939488,-24.7692391009706,-24.6808708886705,-24.5893145527689,
-24.5010479092867,-24.4127945187446,-24.3245330365521,-24.2362421174512,
-24.1478511319343,-24.0594005437268,-23.9708206190652,-23.9484202014577,
-23.8598575551356,-23.7713953969511,-23.6830309769814,-23.6507319389946),
 .UNSPECIFIED.);
#1239=B_SPLINE_CURVE_WITH_KNOTS('',3,(#13295,#13296,#13297,#13298,#13299,
#13300,#13301,#13302,#13303,#13304),.UNSPECIFIED.,.F.,.F.,(4,1,1,1,1,1,
1,4),(-35.5086755760922,-34.9247794604591,-33.9269286187317,-32.9290777770043,
-31.9312269352769,-30.9333760935495,-29.9355252518221,-29.2254902689126),
 .UNSPECIFIED.);
#1240=B_SPLINE_CURVE_WITH_KNOTS('',3,(#13306,#13307,#13308,#13309,#13310,
#13311,#13312,#13313,#13314,#13315,#13316,#13317,#13318,#13319,#13320,#13321,
#13322,#13323,#13324,#13325,#13326,#13327,#13328,#13329,#13330,#13331,#13332,
#13333,#13334,#13335,#13336,#13337,#13338,#13339,#13340,#13341,#13342,#13343,
#13344,#13345,#13346,#13347,#13348,#13349,#13350,#13351,#13352,#13353,#13354,
#13355,#13356,#13357,#13358,#13359,#13360,#13361,#13362,#13363,#13364,#13365,
#13366,#13367,#13368,#13369,#13370,#13371,#13372,#13373,#13374,#13375,#13376,
#13377,#13378,#13379,#13380,#13381,#13382,#13383,#13384,#13385,#13386,#13387,
#13388,#13389,#13390,#13391,#13392,#13393,#13394,#13395,#13396,#13397,#13398,
#13399,#13400,#13401,#13402,#13403,#13404,#13405,#13406,#13407,#13408,#13409,
#13410,#13411,#13412,#13413,#13414,#13415,#13416,#13417,#13418,#13419,#13420,
#13421,#13422,#13423,#13424,#13425,#13426,#13427,#13428,#13429,#13430,#13431,
#13432,#13433,#13434,#13435,#13436,#13437,#13438,#13439,#13440,#13441,#13442,
#13443,#13444,#13445,#13446,#13447,#13448,#13449,#13450,#13451,#13452,#13453,
#13454,#13455,#13456,#13457,#13458,#13459,#13460,#13461,#13462,#13463,#13464,
#13465,#13466,#13467,#13468,#13469,#13470,#13471,#13472,#13473,#13474,#13475,
#13476,#13477,#13478,#13479,#13480,#13481,#13482,#13483,#13484,#13485,#13486,
#13487,#13488,#13489,#13490,#13491,#13492,#13493,#13494,#13495,#13496,#13497,
#13498,#13499,#13500,#13501,#13502,#13503,#13504,#13505,#13506,#13507,#13508,
#13509,#13510,#13511,#13512,#13513,#13514,#13515,#13516,#13517,#13518,#13519,
#13520,#13521,#13522,#13523,#13524,#13525,#13526,#13527,#13528,#13529,#13530,
#13531),.UNSPECIFIED.,.F.,.F.,(4,3,3,3,3,3,3,3,3,3,3,3,3,3,3,3,3,3,3,3,
3,3,3,3,3,3,3,3,3,3,3,3,3,3,3,3,3,3,3,3,3,3,3,3,3,3,3,3,3,3,3,3,3,3,3,3,
3,3,3,3,3,3,3,3,3,3,3,3,3,3,3,3,3,3,3,4),(-41.7918608832718,-41.7045602143125,
-41.6173582380344,-41.529174022133,-41.4420878044719,-41.3550194181906,
-41.2679464497759,-41.1789309650378,-41.0917343409792,-41.0018094259014,
-40.9118845108235,-40.823311361517,-40.7348525684672,-40.6464843560947,
-40.5549280202198,-40.466661376663,-40.3784079860458,-40.2901465037774,
-40.2018555846002,-40.1134645990067,-40.0250140107227,-39.9364340859845,
-39.9140336690961,-39.8254605197895,-39.7370017267396,-39.6486335143673,
-39.5570771784925,-39.4688105349357,-39.3805571443185,-39.2922956620502,
-39.2040047428731,-39.1156137572796,-39.027163168995,-38.9385832442569,
-38.9161828273687,-38.8276096780622,-38.7391508850123,-38.6507826726396,
-38.5592263367648,-38.470959693208,-38.3827063025907,-38.2944448203224,
-38.2061539011449,-38.1177629155515,-38.0293123272675,-37.9407324025291,
-37.9183319856413,-37.8297588363347,-37.7413000432849,-37.6529318309125,
-37.5613754950377,-37.4731088514809,-37.3848554608634,-37.2965939785949,
-37.2083030594178,-37.1199120738244,-37.0314614855404,-36.942881560802,
-36.9204811439139,-36.8319079946074,-36.7434492015581,-36.6550809891854,
-36.5635246533106,-36.4752580097538,-36.3870046191366,-36.2987431368686,
-36.2104522176913,-36.122061232098,-36.0336106438137,-35.9450307190755,
-35.9226303021865,-35.8250780890747,-35.727916662375,-35.6310133550191,
-35.5344973374085,-35.5086757767519),.UNSPECIFIED.);
#1241=B_SPLINE_CURVE_WITH_KNOTS('',3,(#13533,#13534,#13535,#13536,#13537,
#13538,#13539,#13540,#13541,#13542,#13543),.UNSPECIFIED.,.F.,.F.,(4,1,1,
1,1,1,1,1,4),(-48.0750461904514,-47.8968404029153,-46.8989895611879,-45.9011387194605,
-44.9032878777331,-43.9054370360057,-42.9075861942783,-41.9097353525509,
-41.7918608832718),.UNSPECIFIED.);
#1242=B_SPLINE_CURVE_WITH_KNOTS('',3,(#13545,#13546,#13547,#13548,#13549,
#13550,#13551,#13552,#13553,#13554,#13555,#13556,#13557,#13558,#13559,#13560,
#13561,#13562,#13563,#13564,#13565,#13566,#13567,#13568,#13569,#13570,#13571,
#13572,#13573,#13574,#13575,#13576,#13577,#13578,#13579,#13580,#13581,#13582,
#13583,#13584,#13585,#13586,#13587,#13588,#13589,#13590,#13591,#13592,#13593,
#13594,#13595,#13596,#13597,#13598,#13599,#13600,#13601,#13602,#13603,#13604,
#13605,#13606,#13607,#13608,#13609,#13610,#13611,#13612,#13613,#13614,#13615,
#13616,#13617,#13618,#13619,#13620,#13621,#13622,#13623,#13624,#13625,#13626,
#13627,#13628,#13629,#13630,#13631,#13632,#13633,#13634,#13635,#13636,#13637,
#13638,#13639,#13640,#13641,#13642,#13643,#13644,#13645,#13646,#13647,#13648,
#13649,#13650,#13651,#13652,#13653,#13654,#13655,#13656,#13657,#13658,#13659,
#13660,#13661,#13662,#13663,#13664,#13665,#13666,#13667,#13668,#13669,#13670,
#13671,#13672,#13673,#13674,#13675,#13676,#13677,#13678,#13679,#13680,#13681,
#13682,#13683,#13684,#13685,#13686,#13687,#13688,#13689,#13690,#13691,#13692,
#13693,#13694,#13695,#13696,#13697,#13698,#13699,#13700,#13701,#13702,#13703,
#13704,#13705,#13706,#13707,#13708,#13709,#13710,#13711,#13712,#13713,#13714,
#13715,#13716,#13717,#13718,#13719,#13720,#13721,#13722,#13723,#13724,#13725,
#13726,#13727,#13728,#13729,#13730,#13731,#13732,#13733,#13734,#13735,#13736,
#13737,#13738,#13739,#13740,#13741,#13742,#13743,#13744,#13745,#13746,#13747,
#13748,#13749,#13750,#13751,#13752,#13753,#13754,#13755,#13756,#13757,#13758,
#13759,#13760,#13761,#13762,#13763,#13764,#13765,#13766,#13767,#13768,#13769,
#13770),.UNSPECIFIED.,.F.,.F.,(4,3,3,3,3,3,3,3,3,3,3,3,3,3,3,3,3,3,3,3,
3,3,3,3,3,3,3,3,3,3,3,3,3,3,3,3,3,3,3,3,3,3,3,3,3,3,3,3,3,3,3,3,3,3,3,3,
3,3,3,3,3,3,3,3,3,3,3,3,3,3,3,3,3,3,3,4),(-54.3582314975006,-54.2647917556389,
-54.1695801800491,-54.0757075390233,-53.9798264961515,-53.8839454532797,
-53.7953723039732,-53.7069135109234,-53.6185452985508,-53.526988962676,
-53.4387223191192,-53.3504689285019,-53.2622074462337,-53.1739165270565,
-53.0855255414631,-52.9970749531788,-52.9084950284406,-52.8860946115523,
-52.7975214622457,-52.709062669196,-52.6206944568234,-52.5291381209486,
-52.4408714773918,-52.3526180867744,-52.2643566045061,-52.176065685329,
-52.0876746997355,-51.9992241114512,-51.9106441867131,-51.8882437698249,
-51.7996706205183,-51.7112118274686,-51.622843615096,-51.5312872792212,
-51.4430206356644,-51.354767245047,-51.2665057627787,-51.1782148436015,
-51.089823858008,-51.0013732697238,-50.9127933449856,-50.8903929280975,
-50.8018197787909,-50.7133609857412,-50.6249927733686,-50.5334364374938,
-50.445169793937,-50.3569164033197,-50.2686549210514,-50.1803640018742,
-50.0919730162807,-50.0035224279965,-49.9149425032583,-49.8925420863701,
-49.8039689370635,-49.7155101440138,-49.6271419316412,-49.5355855957664,
-49.4473189522096,-49.3590655615923,-49.270804079324,-49.1825131601468,
-49.0941221745533,-49.0056715862691,-48.9170916615308,-48.8946912446427,
-48.8074317150173,-48.7158835244466,-48.6288408914097,-48.5418520352153,
-48.4548944238513,-48.3679455587705,-48.2809477662494,-48.1939214043438,
-48.1068026622736,-48.0750461904514),.UNSPECIFIED.);
#1243=B_SPLINE_CURVE_WITH_KNOTS('',3,(#13772,#13773,#13774,#13775,#13776,
#13777,#13778,#13779,#13780,#13781,#13782,#13783,#13784,#13785,#13786,#13787,
#13788,#13789,#13790,#13791,#13792,#13793,#13794,#13795,#13796,#13797,#13798,
#13799,#13800,#13801,#13802,#13803,#13804,#13805,#13806,#13807,#13808,#13809,
#13810,#13811,#13812,#13813,#13814,#13815,#13816,#13817,#13818,#13819,#13820,
#13821,#13822,#13823,#13824,#13825,#13826,#13827,#13828,#13829,#13830,#13831,
#13832,#13833,#13834,#13835,#13836,#13837,#13838,#13839,#13840,#13841,#13842,
#13843,#13844,#13845,#13846,#13847,#13848,#13849,#13850,#13851,#13852,#13853,
#13854,#13855,#13856,#13857,#13858,#13859,#13860,#13861,#13862,#13863,#13864,
#13865,#13866,#13867,#13868,#13869,#13870,#13871,#13872,#13873,#13874,#13875,
#13876,#13877,#13878,#13879,#13880,#13881,#13882,#13883,#13884,#13885,#13886,
#13887,#13888,#13889,#13890,#13891,#13892,#13893,#13894,#13895,#13896,#13897,
#13898,#13899,#13900,#13901,#13902,#13903,#13904,#13905,#13906,#13907,#13908,
#13909,#13910,#13911,#13912,#13913,#13914,#13915,#13916,#13917,#13918,#13919,
#13920,#13921,#13922,#13923,#13924,#13925,#13926,#13927,#13928,#13929,#13930,
#13931,#13932,#13933,#13934,#13935,#13936,#13937,#13938,#13939,#13940,#13941,
#13942,#13943,#13944,#13945,#13946,#13947,#13948,#13949,#13950,#13951,#13952,
#13953,#13954,#13955,#13956,#13957,#13958,#13959,#13960,#13961,#13962,#13963,
#13964,#13965,#13966,#13967,#13968,#13969,#13970,#13971,#13972,#13973,#13974,
#13975,#13976,#13977,#13978,#13979,#13980,#13981,#13982,#13983,#13984,#13985,
#13986,#13987,#13988,#13989,#13990,#13991,#13992,#13993,#13994,#13995,#13996,
#13997),.UNSPECIFIED.,.F.,.F.,(4,3,3,3,3,3,3,3,3,3,3,3,3,3,3,3,3,3,3,3,
3,3,3,3,3,3,3,3,3,3,3,3,3,3,3,3,3,3,3,3,3,3,3,3,3,3,3,3,3,3,3,3,3,3,3,3,
3,3,3,3,3,3,3,3,3,3,3,3,3,3,3,3,3,3,3,4),(-60.6414168048105,-60.554197711858,
-60.4670437575023,-60.3799239860027,-60.2928160031432,-60.2056974286979,
-60.1184916829168,-60.0312413217147,-59.9438501869995,-59.8710505036442,
-59.7824773543376,-59.6940185612878,-59.6056503489153,-59.5140940130405,
-59.4258273694837,-59.3375739788664,-59.2493124965982,-59.161021577421,
-59.0726305918274,-58.9841800035434,-58.8956000788052,-58.8731996619168,
-58.7846265126102,-58.6961677195605,-58.607799507188,-58.5162431713132,
-58.4279765277564,-58.3397231371391,-58.2514616548708,-58.1631707356939,
-58.0747797501003,-57.986329161816,-57.8977492370779,-57.8753488201894,
-57.7867756708829,-57.6983168778333,-57.6099486654606,-57.5183923295858,
-57.430125686029,-57.3418722954117,-57.2536108131436,-57.1653198939667,
-57.0769289083732,-56.9884783200889,-56.8998983953508,-56.877497978462,
-56.7889248291554,-56.7004660361058,-56.6120978237337,-56.5205414878588,
-56.432274844302,-56.3440214536848,-56.2557599714167,-56.1674690522392,
-56.0790780666456,-55.9906274783613,-55.9020475536231,-55.8796471367345,
-55.7910739874278,-55.7026151943779,-55.6142469820052,-55.5226906461304,
-55.4344240025736,-55.3461706119563,-55.2579091296881,-55.1696182105107,
-55.0812272249172,-54.9927766366329,-54.9041967118949,-54.8817962950071,
-54.7896385149841,-54.6976344620866,-54.6058196949302,-54.5141167775383,
-54.4225461234989,-54.358231497631),.UNSPECIFIED.);
#1244=B_SPLINE_CURVE_WITH_KNOTS('',3,(#13999,#14000,#14001,#14002,#14003,
#14004,#14005,#14006,#14007,#14008,#14009),.UNSPECIFIED.,.F.,.F.,(4,1,1,
1,1,1,1,1,4),(-66.9246021119902,-66.856006395736,-65.8581555540086,-64.8603047122812,
-63.8624538705538,-62.8646030288264,-61.866752187099,-60.8689013453716,
-60.6414168048105),.UNSPECIFIED.);
#1245=B_SPLINE_CURVE_WITH_KNOTS('',3,(#14011,#14012,#14013,#14014,#14015,
#14016,#14017,#14018,#14019,#14020,#14021,#14022,#14023,#14024,#14025,#14026,
#14027,#14028,#14029,#14030,#14031,#14032,#14033,#14034,#14035,#14036,#14037,
#14038,#14039,#14040,#14041,#14042,#14043,#14044,#14045,#14046,#14047,#14048,
#14049,#14050,#14051,#14052,#14053,#14054,#14055,#14056,#14057,#14058,#14059,
#14060,#14061,#14062,#14063,#14064,#14065,#14066,#14067,#14068,#14069,#14070,
#14071,#14072,#14073,#14074,#14075,#14076,#14077,#14078,#14079,#14080,#14081,
#14082,#14083,#14084,#14085,#14086,#14087,#14088,#14089,#14090,#14091,#14092,
#14093,#14094,#14095,#14096,#14097,#14098,#14099,#14100,#14101,#14102,#14103,
#14104,#14105,#14106,#14107,#14108,#14109,#14110,#14111,#14112,#14113,#14114,
#14115,#14116,#14117,#14118,#14119,#14120,#14121,#14122,#14123,#14124,#14125,
#14126,#14127,#14128,#14129,#14130,#14131,#14132,#14133,#14134,#14135,#14136,
#14137,#14138,#14139,#14140,#14141,#14142,#14143,#14144,#14145,#14146,#14147,
#14148,#14149,#14150,#14151,#14152,#14153,#14154,#14155,#14156,#14157,#14158,
#14159,#14160,#14161,#14162,#14163,#14164,#14165,#14166,#14167,#14168,#14169,
#14170,#14171,#14172,#14173,#14174,#14175,#14176,#14177,#14178,#14179,#14180,
#14181,#14182,#14183,#14184,#14185,#14186,#14187,#14188,#14189,#14190,#14191,
#14192,#14193,#14194,#14195,#14196,#14197,#14198,#14199,#14200,#14201,#14202,
#14203,#14204,#14205,#14206,#14207,#14208,#14209,#14210,#14211,#14212,#14213,
#14214,#14215,#14216,#14217,#14218,#14219,#14220,#14221,#14222,#14223,#14224,
#14225,#14226,#14227,#14228,#14229,#14230,#14231,#14232,#14233,#14234,#14235,
#14236),.UNSPECIFIED.,.F.,.F.,(4,3,3,3,3,3,3,3,3,3,3,3,3,3,3,3,3,3,3,3,
3,3,3,3,3,3,3,3,3,3,3,3,3,3,3,3,3,3,3,3,3,3,3,3,3,3,3,3,3,3,3,3,3,3,3,3,
3,3,3,3,3,3,3,3,3,3,3,3,3,3,3,3,3,3,3,4),(-73.2077874189366,-73.1077360066987,
-73.0072421038388,-72.9061731673704,-72.8431114461004,-72.7545382967938,
-72.6660795037441,-72.5777112913716,-72.4861549554968,-72.3978883119399,
-72.3096349213225,-72.2213734390542,-72.133082519877,-72.0446915342834,
-71.9562409459991,-71.8676610212609,-71.845260604373,-71.7566874550664,
-71.6682286620166,-71.5798604496439,-71.4883041137691,-71.4000374702123,
-71.311784079595,-71.2235225973267,-71.1352316781495,-71.046840692556,-70.9583901042718,
-70.8698101795335,-70.8474097626456,-70.758836613339,-70.6703778202893,
-70.5820096079168,-70.4904532720419,-70.4021866284851,-70.3139332378678,
-70.2256717555995,-70.1373808364224,-70.0489898508289,-69.9605392625447,
-69.8719593378065,-69.8495589209182,-69.7609857716116,-69.6725269785619,
-69.5841587661893,-69.4926024303144,-69.4043357867576,-69.3160823961403,
-69.227820913872,-69.1395299946948,-69.0511390091013,-68.962688420817,-68.8741084960788,
-68.8517080791908,-68.7631349298842,-68.6746761368344,-68.5863079244618,
-68.494751588587,-68.4064849450302,-68.3182315544129,-68.2299700721446,
-68.1416791529674,-68.0532881673739,-67.9648375790896,-67.8762576543515,
-67.8538572374634,-67.7661482579468,-67.6785529256837,-67.5910465431623,
-67.5036029660177,-67.416191807519,-67.3287908976864,-67.24137807933,-67.1538814321558,
-67.066339207297,-66.9786674844112,-66.9246021119902),.UNSPECIFIED.);
#1246=B_SPLINE_CURVE_WITH_KNOTS('',3,(#14238,#14239,#14240,#14241,#14242,
#14243,#14244,#14245,#14246,#14247,#14248,#14249,#14250,#14251,#14252,#14253,
#14254,#14255,#14256,#14257,#14258,#14259,#14260,#14261,#14262,#14263,#14264,
#14265,#14266,#14267,#14268,#14269,#14270,#14271,#14272,#14273,#14274,#14275,
#14276,#14277,#14278,#14279,#14280,#14281,#14282,#14283,#14284,#14285,#14286,
#14287,#14288,#14289,#14290,#14291,#14292,#14293,#14294,#14295,#14296,#14297,
#14298,#14299,#14300,#14301,#14302,#14303,#14304,#14305,#14306,#14307,#14308,
#14309,#14310,#14311,#14312,#14313,#14314,#14315,#14316,#14317,#14318,#14319,
#14320,#14321,#14322,#14323,#14324,#14325,#14326,#14327,#14328,#14329,#14330,
#14331,#14332,#14333,#14334,#14335,#14336,#14337,#14338,#14339,#14340,#14341,
#14342,#14343,#14344,#14345,#14346,#14347,#14348,#14349,#14350,#14351,#14352,
#14353,#14354,#14355,#14356,#14357,#14358,#14359,#14360,#14361,#14362,#14363,
#14364,#14365,#14366,#14367,#14368,#14369,#14370,#14371,#14372,#14373,#14374,
#14375,#14376,#14377,#14378,#14379,#14380,#14381,#14382,#14383,#14384,#14385,
#14386,#14387,#14388,#14389,#14390,#14391,#14392,#14393,#14394,#14395,#14396,
#14397,#14398,#14399,#14400,#14401,#14402,#14403,#14404,#14405,#14406,#14407,
#14408,#14409,#14410,#14411,#14412,#14413,#14414,#14415,#14416,#14417,#14418,
#14419,#14420,#14421,#14422,#14423,#14424,#14425,#14426,#14427,#14428,#14429,
#14430,#14431,#14432,#14433,#14434,#14435,#14436,#14437,#14438,#14439,#14440,
#14441,#14442,#14443,#14444,#14445,#14446,#14447,#14448,#14449,#14450,#14451,
#14452,#14453,#14454,#14455,#14456,#14457,#14458,#14459,#14460,#14461,#14462,
#14463),.UNSPECIFIED.,.F.,.F.,(4,3,3,3,3,3,3,3,3,3,3,3,3,3,3,3,3,3,3,3,
3,3,3,3,3,3,3,3,3,3,3,3,3,3,3,3,3,3,3,3,3,3,3,3,3,3,3,3,3,3,3,3,3,3,3,3,
3,3,3,3,3,3,3,3,3,3,3,3,3,3,3,3,3,3,3,4),(-79.4909727263493,-79.4027030535825,
-79.3144454917003,-79.2261787933953,-79.137881709884,-79.0494784849831,
-78.9610151902704,-78.8724102190023,-78.8302164964648,-78.7416433471582,
-78.6531845541085,-78.564816341736,-78.4732600058611,-78.3849933623043,
-78.296739971687,-78.2084784894188,-78.1201875702418,-78.0317965846482,
-77.9433459963641,-77.8547660716259,-77.8323656547374,-77.7437925054308,
-77.655333712381,-77.5669655000085,-77.4754091641337,-77.3871425205769,
-77.2988891299597,-77.2106276476916,-77.1223367285145,-77.033945742921,
-76.9454951546369,-76.8569152298987,-76.83451481301,-76.7459416637034,-76.6574828706536,
-76.5691146582808,-76.477558322406,-76.3892916788491,-76.3010382882317,
-76.2127768059632,-76.1244858867861,-76.0360949011925,-75.9476443129081,
-75.85906438817,-75.8366639712826,-75.7480908219759,-75.659632028926,-75.5712638165536,
-75.4797074806788,-75.3914408371219,-75.3031874465046,-75.2149259642361,
-75.1266350450588,-75.0382440594654,-74.9497934711811,-74.8612135464427,
-74.8388131295552,-74.7502399802486,-74.6617811871993,-74.5734129748265,
-74.4818566389517,-74.3935899953948,-74.3053366047776,-74.2170751225096,
-74.128784203332,-74.0403932177385,-73.9519426294543,-73.8633627047161,
-73.8409622878278,-73.7518618126712,-73.6628783053694,-73.5739909580721,
-73.4824400733465,-73.3936855521496,-73.3007364856597,-73.2077874191697),
 .UNSPECIFIED.);
#1247=B_SPLINE_CURVE_WITH_KNOTS('',3,(#14465,#14466,#14467,#14468,#14469,
#14470,#14471,#14472,#14473,#14474),.UNSPECIFIED.,.F.,.F.,(4,1,1,1,1,1,
1,4),(-85.7741526916333,-84.8173215468292,-83.8194707051018,-82.8216198633744,
-81.823769021647,-80.8259181799196,-79.8280673381922,-79.4909799947471),
 .UNSPECIFIED.);
#1248=B_SPLINE_CURVE_WITH_KNOTS('',3,(#14476,#14477,#14478,#14479,#14480,
#14481,#14482,#14483,#14484,#14485,#14486,#14487,#14488,#14489,#14490,#14491,
#14492,#14493,#14494,#14495,#14496,#14497,#14498,#14499,#14500,#14501,#14502,
#14503,#14504,#14505,#14506,#14507,#14508,#14509,#14510,#14511,#14512,#14513,
#14514,#14515,#14516,#14517,#14518,#14519,#14520,#14521,#14522,#14523,#14524,
#14525,#14526,#14527,#14528,#14529,#14530,#14531,#14532,#14533,#14534,#14535,
#14536,#14537,#14538,#14539,#14540,#14541,#14542,#14543,#14544,#14545,#14546,
#14547,#14548,#14549,#14550,#14551,#14552,#14553,#14554,#14555,#14556,#14557,
#14558,#14559,#14560,#14561,#14562,#14563,#14564,#14565,#14566,#14567,#14568,
#14569,#14570,#14571,#14572,#14573,#14574,#14575,#14576,#14577,#14578,#14579,
#14580,#14581,#14582,#14583,#14584,#14585,#14586,#14587,#14588,#14589,#14590,
#14591,#14592,#14593,#14594,#14595,#14596,#14597,#14598,#14599,#14600,#14601,
#14602,#14603,#14604,#14605,#14606,#14607,#14608,#14609,#14610,#14611,#14612,
#14613,#14614,#14615,#14616,#14617,#14618,#14619,#14620,#14621,#14622,#14623,
#14624,#14625,#14626,#14627,#14628,#14629,#14630,#14631,#14632,#14633,#14634,
#14635,#14636,#14637,#14638,#14639,#14640,#14641,#14642,#14643,#14644,#14645,
#14646,#14647,#14648,#14649,#14650,#14651,#14652,#14653,#14654,#14655,#14656,
#14657,#14658,#14659,#14660,#14661,#14662,#14663,#14664,#14665,#14666,#14667,
#14668,#14669,#14670,#14671,#14672,#14673,#14674,#14675,#14676,#14677,#14678,
#14679,#14680,#14681,#14682,#14683,#14684,#14685,#14686,#14687,#14688,#14689,
#14690,#14691,#14692,#14693,#14694,#14695,#14696,#14697,#14698,#14699,#14700,
#14701,#14702,#14703,#14704),.UNSPECIFIED.,.F.,.F.,(4,3,3,3,3,3,3,3,3,3,
3,3,3,3,3,3,3,3,3,3,3,3,3,3,3,3,3,3,3,3,3,3,3,3,3,3,3,3,3,3,3,3,3,3,3,3,
3,3,3,3,3,3,3,3,3,3,3,3,3,3,3,3,3,3,3,3,3,3,3,3,3,3,3,3,3,3,4),(-92.0573432033913,
-91.9449585863266,-91.830194852235,-91.8022774389211,-91.7137042896145,
-91.6252454965648,-91.5368772841921,-91.4453209483173,-91.3570543047604,
-91.2688009141431,-91.1805394318749,-91.0922485126977,-91.0038575271042,
-90.91540693882,-90.8268270140818,-90.8044265971936,-90.715853447887,-90.6273946548373,
-90.5390264424647,-90.4474701065899,-90.3592034630331,-90.2709500724158,
-90.1826885901474,-90.0943976709703,-90.0060066853768,-89.9175560970926,
-89.8289761723544,-89.8065757554662,-89.7180026061596,-89.6295438131099,
-89.5411756007373,-89.4496192648625,-89.3613526213056,-89.2730992306883,
-89.18483774842,-89.0965468292428,-89.0081558436493,-88.919705255365,-88.8311253306268,
-88.8087249137388,-88.7201517644322,-88.6316929713825,-88.5433247590099,
-88.4517684231351,-88.3635017795783,-88.275248388961,-88.1869869066927,
-88.0986959875155,-88.010305001922,-87.9218544136378,-87.8332744888996,
-87.8108740720114,-87.7223009227048,-87.6338421296551,-87.5454739172824,
-87.4539175814076,-87.3656509378508,-87.2773975472335,-87.1891360649651,
-87.100845145788,-87.0124541601946,-86.9240035719104,-86.8354236471722,
-86.813023230284,-86.7244500809774,-86.6359912879277,-86.5476230755552,
-86.4560667396804,-86.3678000961236,-86.2795467055063,-86.191285223238,
-86.1029943040609,-86.0146033184674,-85.9261527301832,-85.837572805445,
-85.8151723885566,-85.7741580335289),.UNSPECIFIED.);
#1249=B_SPLINE_CURVE_WITH_KNOTS('',3,(#14706,#14707,#14708,#14709,#14710,
#14711,#14712,#14713,#14714,#14715),.UNSPECIFIED.,.F.,.F.,(4,1,1,1,1,1,
1,4),(-98.3405286478881,-97.7893824892855,-96.791531647558,-95.7936808058307,
-94.7958299641032,-93.7979791223758,-92.8001282806485,-92.0573433407085),
 .UNSPECIFIED.);
#1250=B_SPLINE_CURVE_WITH_KNOTS('',3,(#14717,#14718,#14719,#14720,#14721,
#14722,#14723,#14724,#14725,#14726),.UNSPECIFIED.,.F.,.F.,(4,1,1,1,1,1,
1,4),(-104.623706641862,-103.77648753965,-102.778636697922,-101.780785856195,
-100.782935014468,-99.7850841727403,-98.7872333310129,-98.3405286478881),
 .UNSPECIFIED.);
#1251=B_SPLINE_CURVE_WITH_KNOTS('',3,(#14728,#14729,#14730,#14731,#14732,
#14733,#14734,#14735,#14736,#14737,#14738,#14739,#14740,#14741,#14742,#14743,
#14744,#14745,#14746,#14747,#14748,#14749,#14750,#14751,#14752,#14753,#14754,
#14755,#14756,#14757,#14758,#14759,#14760,#14761,#14762,#14763,#14764,#14765,
#14766,#14767,#14768,#14769,#14770,#14771,#14772,#14773,#14774,#14775,#14776,
#14777,#14778,#14779,#14780,#14781,#14782,#14783,#14784,#14785,#14786,#14787,
#14788,#14789,#14790,#14791,#14792,#14793,#14794,#14795,#14796,#14797,#14798,
#14799,#14800,#14801,#14802,#14803,#14804,#14805,#14806,#14807,#14808,#14809,
#14810,#14811,#14812,#14813,#14814,#14815,#14816,#14817,#14818,#14819,#14820,
#14821,#14822,#14823,#14824,#14825,#14826,#14827,#14828,#14829,#14830,#14831,
#14832,#14833,#14834,#14835,#14836,#14837,#14838,#14839,#14840,#14841,#14842,
#14843,#14844,#14845,#14846,#14847,#14848,#14849,#14850,#14851,#14852,#14853,
#14854,#14855,#14856,#14857,#14858,#14859,#14860,#14861,#14862,#14863,#14864,
#14865,#14866,#14867,#14868,#14869,#14870,#14871,#14872,#14873,#14874,#14875,
#14876,#14877,#14878,#14879,#14880,#14881,#14882,#14883,#14884,#14885,#14886,
#14887,#14888,#14889,#14890,#14891,#14892,#14893,#14894,#14895,#14896,#14897,
#14898,#14899,#14900,#14901,#14902,#14903,#14904,#14905,#14906,#14907,#14908,
#14909,#14910,#14911,#14912,#14913,#14914,#14915,#14916,#14917,#14918,#14919,
#14920,#14921,#14922,#14923,#14924,#14925,#14926,#14927,#14928,#14929,#14930,
#14931,#14932,#14933,#14934,#14935,#14936,#14937,#14938,#14939,#14940,#14941,
#14942,#14943,#14944,#14945,#14946,#14947,#14948,#14949,#14950),
 .UNSPECIFIED.,.F.,.F.,(4,3,3,3,3,3,3,3,3,3,3,3,3,3,3,3,3,3,3,3,3,3,3,3,
3,3,3,3,3,3,3,3,3,3,3,3,3,3,3,3,3,3,3,3,3,3,3,3,3,3,3,3,3,3,3,3,3,3,3,3,
3,3,3,3,3,3,3,3,3,3,3,3,3,3,4),(-110.906899262247,-110.761443431742,-110.672870261492,
-110.584411447275,-110.496043213538,-110.404486885598,-110.316220220321,
-110.22796680789,-110.139705303736,-110.051414362625,-109.963023355137,
-109.874572744955,-109.785992798481,-109.763592590014,-109.675019440711,
-109.586560647612,-109.498192435137,-109.406636099281,-109.318369455489,
-109.230116064587,-109.141854581985,-109.053563662425,-108.965172676378,
-108.876722087598,-108.788142162306,-108.765741748287,-108.677168604673,
-108.588709817407,-108.500341610901,-108.408785272858,-108.320518635341,
-108.232265250816,-108.144003774687,-108.05571286169,-107.967321882306,
-107.878871300257,-107.790291381742,-107.767890906559,-107.679317754033,
-107.590858957727,-107.502490742065,-107.410934407411,-107.322667760504,
-107.234414366519,-107.14615288087,-107.057861958303,-106.969470969322,
-106.881020377648,-106.792440449541,-106.770040064832,-106.681466915798,
-106.593008123017,-106.504639910909,-106.413083574933,-106.324816931629,
-106.236563541259,-106.148302059232,-106.060011140292,-105.971620154925,
-105.883169566862,-105.794589642336,-105.772189223105,-105.68361607452,
-105.595157282203,-105.506789070576,-105.415232734426,-105.326966091637,
-105.238712701796,-105.15045122031,-105.062160301921,-104.97376931712,-104.885318729632,
-104.79673880569,-104.774338381377,-104.623713955068),.UNSPECIFIED.);
#1252=B_SPLINE_CURVE_WITH_KNOTS('',3,(#14952,#14953,#14954,#14955,#14956,
#14957,#14958,#14959,#14960,#14961),.UNSPECIFIED.,.F.,.F.,(4,1,1,1,1,1,
1,4),(-117.19008011828,-116.748548482106,-115.750697640379,-114.752846798651,
-113.754995956924,-112.757145115197,-111.759294273469,-110.906906884946),
 .UNSPECIFIED.);
#1253=B_SPLINE_CURVE_WITH_KNOTS('',3,(#14963,#14964,#14965,#14966,#14967,
#14968,#14969,#14970,#14971,#14972,#14973,#14974,#14975,#14976,#14977,#14978,
#14979,#14980,#14981,#14982,#14983,#14984,#14985,#14986,#14987,#14988,#14989,
#14990,#14991,#14992,#14993,#14994,#14995,#14996,#14997,#14998,#14999,#15000,
#15001,#15002,#15003,#15004,#15005,#15006,#15007,#15008,#15009,#15010,#15011,
#15012,#15013,#15014,#15015,#15016,#15017,#15018,#15019,#15020,#15021,#15022,
#15023,#15024,#15025,#15026,#15027,#15028,#15029,#15030,#15031,#15032,#15033,
#15034,#15035,#15036,#15037,#15038,#15039,#15040,#15041,#15042,#15043,#15044,
#15045,#15046,#15047,#15048,#15049,#15050,#15051,#15052,#15053,#15054,#15055,
#15056,#15057,#15058,#15059,#15060,#15061,#15062,#15063,#15064,#15065,#15066,
#15067,#15068,#15069,#15070,#15071,#15072,#15073,#15074,#15075,#15076,#15077,
#15078,#15079,#15080,#15081,#15082,#15083,#15084,#15085,#15086,#15087,#15088,
#15089,#15090,#15091,#15092,#15093,#15094,#15095,#15096,#15097,#15098,#15099,
#15100,#15101,#15102,#15103,#15104,#15105,#15106,#15107,#15108,#15109,#15110,
#15111,#15112,#15113,#15114,#15115,#15116,#15117,#15118,#15119,#15120,#15121,
#15122,#15123,#15124,#15125,#15126,#15127,#15128,#15129,#15130,#15131,#15132,
#15133,#15134,#15135,#15136,#15137,#15138,#15139,#15140,#15141,#15142,#15143,
#15144,#15145,#15146,#15147,#15148,#15149,#15150,#15151,#15152,#15153,#15154,
#15155,#15156,#15157,#15158,#15159,#15160,#15161,#15162,#15163,#15164,#15165,
#15166,#15167,#15168,#15169,#15170,#15171,#15172,#15173,#15174,#15175,#15176,
#15177,#15178,#15179,#15180,#15181,#15182,#15183,#15184,#15185,#15186,#15187,
#15188),.UNSPECIFIED.,.F.,.F.,(4,3,3,3,3,3,3,3,3,3,3,3,3,3,3,3,3,3,3,3,
3,3,3,3,3,3,3,3,3,3,3,3,3,3,3,3,3,3,3,3,3,3,3,3,3,3,3,3,3,3,3,3,3,3,3,3,
3,3,3,3,3,3,3,3,3,3,3,3,3,3,3,3,3,3,3,4),(-123.473269876606,-123.385963817173,
-123.298706638601,-123.211472892286,-123.124240298723,-123.036986583253,
-122.949638453688,-122.862236484049,-122.774701382474,-122.735653532471,
-122.64705600505,-122.558572741542,-122.470179996843,-122.378632833581,
-122.290341662701,-122.202063789463,-122.113777896155,-122.025462664474,
-121.937047636497,-121.848573134328,-121.759969668638,-121.737802690743,
-121.649211601926,-121.560734519507,-121.472347691821,-121.38079821147,
-121.292512254859,-121.204239325495,-121.115958098892,-121.027647249759,
-120.93923615818,-120.850765336606,-120.762165146963,-120.739951849016,
-120.651395452075,-120.562953632999,-120.474602594572,-120.383039896162,
-120.294790817753,-120.206555107228,-120.118311401479,-120.030038336789,
-119.941665231825,-119.853232561338,-119.764670471248,-119.742101007288,
-119.653523259052,-119.565059836333,-119.476686969352,-119.385132368878,
-119.296861038376,-119.208602956949,-119.120336785073,-119.032041182565,
-118.943645546695,-118.855190321758,-118.766605816084,-118.744250165561,
-118.655675059032,-118.567214265706,-118.478844012632,-118.387288426532,
-118.299019653933,-118.210764105141,-118.122500437758,-118.0342073087,-117.945814087448,
-117.857361245723,-117.768779058712,-117.746399323834,-117.655351667581,
-117.564442627165,-117.47085311273,-117.380199332793,-117.28514195111,-117.190084569427),
 .UNSPECIFIED.);
#1254=B_SPLINE_CURVE_WITH_KNOTS('',3,(#15190,#15191,#15192,#15193,#15194,
#15195,#15196,#15197),.UNSPECIFIED.,.F.,.F.,(4,1,1,1,1,4),(-127.724907741108,
-126.72705689938,-125.729206057653,-124.731355215925,-123.733504374198,
-123.473272729035),.UNSPECIFIED.);
#1255=B_SPLINE_CURVE_WITH_KNOTS('',3,(#15201,#15202,#15203,#15204,#15205,
#15206,#15207,#15208,#15209,#15210,#15211,#15212,#15213,#15214,#15215,#15216,
#15217,#15218,#15219,#15220,#15221,#15222,#15223,#15224,#15225,#15226,#15227,
#15228,#15229,#15230,#15231,#15232,#15233,#15234,#15235,#15236,#15237,#15238,
#15239,#15240,#15241,#15242,#15243,#15244,#15245,#15246,#15247,#15248,#15249,
#15250,#15251,#15252,#15253,#15254,#15255,#15256,#15257,#15258,#15259,#15260,
#15261,#15262,#15263,#15264,#15265,#15266,#15267,#15268,#15269,#15270,#15271,
#15272,#15273,#15274,#15275,#15276,#15277,#15278,#15279,#15280,#15281,#15282,
#15283,#15284,#15285,#15286,#15287,#15288,#15289,#15290,#15291,#15292,#15293,
#15294,#15295,#15296,#15297,#15298,#15299,#15300,#15301,#15302,#15303,#15304,
#15305,#15306,#15307,#15308,#15309,#15310,#15311,#15312,#15313,#15314,#15315,
#15316,#15317,#15318,#15319,#15320,#15321,#15322,#15323,#15324,#15325,#15326,
#15327,#15328,#15329,#15330,#15331,#15332,#15333,#15334,#15335,#15336,#15337,
#15338,#15339,#15340,#15341,#15342,#15343,#15344,#15345,#15346,#15347,#15348,
#15349,#15350,#15351,#15352,#15353,#15354,#15355,#15356,#15357,#15358,#15359,
#15360,#15361,#15362,#15363,#15364,#15365,#15366,#15367,#15368,#15369,#15370,
#15371,#15372,#15373,#15374,#15375,#15376,#15377,#15378,#15379,#15380,#15381,
#15382,#15383,#15384,#15385,#15386,#15387),.UNSPECIFIED.,.F.,.F.,(4,3,3,
3,3,3,3,3,3,3,3,3,3,3,3,3,3,3,3,3,3,3,3,3,3,3,3,3,3,3,3,3,3,3,3,3,3,3,3,
3,3,3,3,3,3,3,3,3,3,3,3,3,3,3,3,3,3,3,3,3,3,3,4),(120.490566152121,120.603837052801,
120.71967464691,120.739951849016,120.828545137016,120.917023992194,121.005412168038,
121.096960983376,121.185247223457,121.273520042512,121.361800765146,121.450110716473,
121.538520332177,121.626989338908,121.715587232755,121.737802690743,121.826399174075,
121.91488156938,122.003273621172,122.094821110084,122.183112028445,122.271389812282,
122.359675779401,122.44799124832,122.536406754079,122.624881874923,122.71348616021,
122.735653532471,122.82410435621,122.912440558979,123.000686058367,123.092288347846,
123.180432724514,123.268564214759,123.356704288735,123.444874417773,123.5331461304,
123.62147818081,123.70994155568,123.733504374198,123.822247266296,123.910875376148,
123.999412284792,124.090905151184,124.179337895411,124.2677561418,124.356181059584,
124.444633817484,124.533183474876,124.62179107482,124.710524399572,124.731355215925,
124.819152681151,124.906838203155,124.994436379332,125.08197397875,125.169480475744,
125.256977959367,125.344488506912,125.432084824851,125.519727567832,125.607501981674,
125.66337244262),.UNSPECIFIED.);
#1256=B_SPLINE_CURVE_WITH_KNOTS('',3,(#15389,#15390,#15391,#15392,#15393,
#15394,#15395,#15396,#15397,#15398),.UNSPECIFIED.,.F.,.F.,(4,1,1,1,1,1,
1,4),(114.207380740144,114.752846798651,115.750697640379,116.748548482106,
117.746399323834,118.744250165561,119.742101007288,120.490566047323),
 .UNSPECIFIED.);
#1257=B_SPLINE_CURVE_WITH_KNOTS('',3,(#15400,#15401,#15402,#15403,#15404,
#15405,#15406,#15407,#15408,#15409,#15410,#15411,#15412,#15413,#15414,#15415,
#15416,#15417,#15418,#15419,#15420,#15421,#15422,#15423,#15424,#15425,#15426,
#15427,#15428,#15429,#15430,#15431,#15432,#15433,#15434,#15435,#15436,#15437,
#15438,#15439,#15440,#15441,#15442,#15443,#15444,#15445,#15446,#15447,#15448,
#15449,#15450,#15451,#15452,#15453,#15454,#15455,#15456,#15457,#15458,#15459,
#15460,#15461,#15462,#15463,#15464,#15465,#15466,#15467,#15468,#15469,#15470,
#15471,#15472,#15473,#15474,#15475,#15476,#15477,#15478,#15479,#15480,#15481,
#15482,#15483,#15484,#15485,#15486,#15487,#15488,#15489,#15490,#15491,#15492,
#15493,#15494,#15495,#15496,#15497,#15498,#15499,#15500,#15501,#15502,#15503,
#15504,#15505,#15506,#15507,#15508,#15509,#15510,#15511,#15512,#15513,#15514,
#15515,#15516,#15517,#15518,#15519,#15520,#15521,#15522,#15523,#15524,#15525,
#15526,#15527,#15528,#15529,#15530,#15531,#15532,#15533,#15534,#15535,#15536,
#15537,#15538,#15539,#15540,#15541,#15542,#15543,#15544,#15545,#15546,#15547,
#15548,#15549,#15550,#15551,#15552,#15553,#15554,#15555,#15556,#15557,#15558,
#15559,#15560,#15561,#15562,#15563,#15564,#15565,#15566,#15567,#15568,#15569,
#15570,#15571,#15572,#15573,#15574,#15575,#15576,#15577,#15578,#15579,#15580,
#15581,#15582,#15583,#15584,#15585,#15586,#15587,#15588,#15589,#15590,#15591,
#15592,#15593,#15594,#15595,#15596,#15597,#15598,#15599,#15600,#15601,#15602,
#15603,#15604,#15605,#15606,#15607,#15608,#15609,#15610,#15611,#15612,#15613,
#15614,#15615,#15616,#15617,#15618,#15619,#15620,#15621,#15622,#15623,#15624,
#15625),.UNSPECIFIED.,.F.,.F.,(4,3,3,3,3,3,3,3,3,3,3,3,3,3,3,3,3,3,3,3,
3,3,3,3,3,3,3,3,3,3,3,3,3,3,3,3,3,3,3,3,3,3,3,3,3,3,3,3,3,3,3,3,3,3,3,3,
3,3,3,3,3,3,3,3,3,3,3,3,3,3,3,3,3,3,3,4),(107.92419543314,108.011346351858,
108.098408182763,108.185408306089,108.272376673895,108.359335784728,108.446308125387,
108.53336836748,108.620475808099,108.70771888384,108.765741748287,108.854314898151,
108.942773691706,109.031141904533,109.122698240218,109.2109648841,109.299218274993,
109.38747975749,109.475770676847,109.564161662549,109.6526122509,109.741192175643,
109.763592590014,109.852165760785,109.940624575388,110.028992809377,110.120549137172,
110.208815802365,110.29706921459,110.385330718413,110.473621659069,110.562012665923,
110.650463275365,110.73904322095,110.761443431742,110.850016534348,110.938475280703,
111.026843446439,111.118399799818,111.206666397174,111.294919741829,111.383181178421,
111.471472052256,111.559862993227,111.648313537255,111.736893418609,111.759294273469,
111.847867440913,111.936326251761,112.024694481579,112.116250810781,112.204517470803,
112.292770877498,112.381032375441,112.469323309875,112.557714310034,112.646164912499,
112.734744850751,112.757145115197,112.845718398669,112.934177326567,113.022545674305,
113.114101959633,113.202368738992,113.290622265342,113.378883883128,113.467174937462,
113.555566056999,113.644016778682,113.732596834996,113.754995956924,113.850301728731,
113.945297041335,114.04010251559,114.134620297776,114.207380494539),
 .UNSPECIFIED.);
#1258=B_SPLINE_CURVE_WITH_KNOTS('',3,(#15627,#15628,#15629,#15630,#15631,
#15632,#15633,#15634,#15635,#15636,#15637,#15638,#15639,#15640,#15641,#15642,
#15643,#15644,#15645,#15646,#15647,#15648,#15649,#15650,#15651,#15652,#15653,
#15654,#15655,#15656,#15657,#15658,#15659,#15660,#15661,#15662,#15663,#15664,
#15665,#15666,#15667,#15668,#15669,#15670,#15671,#15672,#15673,#15674,#15675,
#15676,#15677,#15678,#15679,#15680,#15681,#15682,#15683,#15684,#15685,#15686,
#15687,#15688,#15689,#15690,#15691,#15692,#15693,#15694,#15695,#15696,#15697,
#15698,#15699,#15700,#15701,#15702,#15703,#15704,#15705,#15706,#15707,#15708,
#15709,#15710,#15711,#15712,#15713,#15714,#15715,#15716,#15717,#15718,#15719,
#15720,#15721,#15722,#15723,#15724,#15725,#15726,#15727,#15728,#15729,#15730,
#15731,#15732,#15733,#15734,#15735,#15736,#15737,#15738,#15739,#15740,#15741,
#15742,#15743,#15744,#15745,#15746,#15747,#15748,#15749,#15750,#15751,#15752,
#15753,#15754,#15755,#15756,#15757,#15758,#15759,#15760,#15761,#15762,#15763,
#15764,#15765,#15766,#15767,#15768,#15769,#15770,#15771,#15772,#15773,#15774,
#15775,#15776,#15777,#15778,#15779,#15780,#15781,#15782,#15783,#15784,#15785,
#15786,#15787,#15788,#15789,#15790,#15791,#15792,#15793,#15794,#15795,#15796,
#15797,#15798,#15799,#15800,#15801,#15802,#15803,#15804,#15805,#15806,#15807,
#15808,#15809,#15810,#15811,#15812,#15813,#15814,#15815,#15816,#15817,#15818,
#15819,#15820,#15821,#15822,#15823,#15824,#15825,#15826,#15827,#15828,#15829,
#15830,#15831,#15832,#15833,#15834,#15835,#15836,#15837,#15838,#15839,#15840,
#15841,#15842,#15843,#15844,#15845,#15846,#15847,#15848,#15849,#15850,#15851,
#15852),.UNSPECIFIED.,.F.,.F.,(4,3,3,3,3,3,3,3,3,3,3,3,3,3,3,3,3,3,3,3,
3,3,3,3,3,3,3,3,3,3,3,3,3,3,3,3,3,3,3,3,3,3,3,3,3,3,3,3,3,3,3,3,3,3,3,3,
3,3,3,3,3,3,3,3,3,3,3,3,3,3,3,3,3,3,3,4),(101.641010125785,101.780785856195,
101.869359005405,101.957817798359,102.046186010637,102.137742346547,102.22600899001,
102.314262380534,102.40252386271,102.490814781796,102.5792057673,102.667656355496,
102.756236280147,102.778636697922,102.867209847159,102.955668640139,103.04403685244,
103.135593188341,103.223859831825,103.312113222368,103.400374704562,103.488665623664,
103.577056609182,103.66550719739,103.754087122053,103.77648753965,103.865060689457,
103.953519483008,104.041887695882,104.133444031569,104.221710675627,104.309964066744,
104.39822554951,104.486516469182,104.574907455265,104.663358044036,104.751937969252,
104.774338381377,104.862911529898,104.951370322164,105.039738533755,105.131294869924,
105.219561512709,105.30781490256,105.396076384068,105.484367302492,105.572758287345,
105.661208874896,105.749788798917,105.772189223105,105.860762372204,105.949221165039,
106.037589377189,106.129145713144,106.217412356462,106.305665746834,106.393927228852,
106.482218147774,106.570609133106,106.659059721124,106.747639645593,106.770040064832,
106.858613217461,106.947072013844,107.035440229556,107.126996564182,107.215263211076,
107.303516605024,107.391778090612,107.480069013096,107.568460001958,107.656910593494,
107.745490521433,107.767890906559,107.913755880126,107.924195432964),
 .UNSPECIFIED.);
#1259=B_SPLINE_CURVE_WITH_KNOTS('',3,(#15854,#15855,#15856,#15857,#15858,
#15859,#15860,#15861,#15862,#15863),.UNSPECIFIED.,.F.,.F.,(4,1,1,1,1,1,
1,4),(95.3578296359417,95.7936808058306,96.791531647558,97.7893824892855,
98.7872333310129,99.7850841727403,100.782935014468,101.641002196766),
 .UNSPECIFIED.);
#1260=B_SPLINE_CURVE_WITH_KNOTS('',3,(#15865,#15866,#15867,#15868,#15869,
#15870,#15871,#15872,#15873,#15874,#15875,#15876,#15877,#15878,#15879,#15880,
#15881,#15882,#15883,#15884,#15885,#15886,#15887,#15888,#15889,#15890,#15891,
#15892,#15893,#15894,#15895,#15896,#15897,#15898,#15899,#15900,#15901,#15902,
#15903,#15904,#15905,#15906,#15907,#15908,#15909,#15910,#15911,#15912,#15913,
#15914,#15915,#15916,#15917,#15918,#15919,#15920,#15921,#15922,#15923,#15924,
#15925,#15926,#15927,#15928,#15929,#15930,#15931,#15932,#15933,#15934,#15935,
#15936,#15937,#15938,#15939,#15940,#15941,#15942,#15943,#15944,#15945,#15946,
#15947,#15948,#15949,#15950,#15951,#15952,#15953,#15954,#15955,#15956,#15957,
#15958,#15959,#15960,#15961,#15962,#15963,#15964,#15965,#15966,#15967,#15968,
#15969,#15970,#15971,#15972,#15973,#15974,#15975,#15976,#15977,#15978,#15979,
#15980,#15981,#15982,#15983,#15984,#15985,#15986,#15987,#15988,#15989,#15990,
#15991,#15992,#15993,#15994,#15995,#15996,#15997,#15998,#15999,#16000,#16001,
#16002,#16003,#16004,#16005,#16006,#16007,#16008,#16009,#16010,#16011,#16012,
#16013,#16014,#16015,#16016,#16017,#16018,#16019,#16020,#16021,#16022,#16023,
#16024,#16025,#16026,#16027,#16028,#16029,#16030,#16031,#16032,#16033,#16034,
#16035,#16036,#16037,#16038,#16039,#16040,#16041,#16042,#16043,#16044,#16045,
#16046,#16047,#16048,#16049,#16050,#16051,#16052,#16053,#16054,#16055,#16056,
#16057,#16058,#16059,#16060,#16061,#16062,#16063,#16064,#16065,#16066,#16067,
#16068,#16069,#16070,#16071,#16072,#16073,#16074,#16075,#16076,#16077,#16078,
#16079,#16080,#16081,#16082,#16083,#16084,#16085,#16086,#16087,#16088,#16089,
#16090,#16091,#16092,#16093),.UNSPECIFIED.,.F.,.F.,(4,3,3,3,3,3,3,3,3,3,
3,3,3,3,3,3,3,3,3,3,3,3,3,3,3,3,3,3,3,3,3,3,3,3,3,3,3,3,3,3,3,3,3,3,3,3,
3,3,3,3,3,3,3,3,3,3,3,3,3,3,3,3,3,3,3,3,3,3,3,3,3,3,3,3,3,3,4),(89.0746395114255,
89.1661315419306,89.2535335418103,89.3409155597643,89.4282997621435,89.515708312922,
89.6032130314677,89.690774292348,89.778465706738,89.8065757554662,89.8951489047728,
89.9836076978226,90.0719759101952,90.16353224607,90.2517988896268,90.3400522802442,
90.4283137625124,90.5166046816894,90.6049956672829,90.6934462555673,90.7820261803054,
90.8044265971937,90.8929997465003,90.98145853955,91.0698267519225,91.1613830877973,
91.2496497313541,91.3379031219715,91.4261646042399,91.5144555234169,91.6028465090104,
91.6912970972943,91.7798770220325,91.8022774389211,91.8908505882279,91.979309381278,
92.0676775936506,92.1592339295253,92.2475005730823,92.3357539636997,92.4240154459682,
92.5123063651454,92.6006973507391,92.6891479390237,92.777727863762,92.8001282806484,
92.8887014299548,92.9771602230042,93.0655284353769,93.1570847712517,93.2453514148085,
93.3336048054257,93.4218662876938,93.5101572068713,93.5985481924647,93.6869987807487,
93.7755787054866,93.7979791223758,93.8865522716819,93.9750110647312,94.0633792771031,
94.1549356129782,94.2432022565346,94.3314556471514,94.4197171294191,94.5080080485956,
94.5963990341886,94.6848496224724,94.7734295472099,94.7958299641032,94.8867065999364,
94.977446835222,95.0725413310677,95.1630320672469,95.2534488825782,95.3437980500512,
95.3578248186051),.UNSPECIFIED.);
#1261=B_SPLINE_CURVE_WITH_KNOTS('',3,(#16095,#16096,#16097,#16098,#16099,
#16100,#16101,#16102,#16103,#16104,#16105,#16106,#16107,#16108,#16109,#16110,
#16111,#16112,#16113,#16114,#16115,#16116,#16117,#16118,#16119,#16120,#16121,
#16122,#16123,#16124,#16125,#16126,#16127,#16128,#16129,#16130,#16131,#16132,
#16133,#16134,#16135,#16136,#16137,#16138,#16139,#16140,#16141,#16142,#16143,
#16144,#16145,#16146,#16147,#16148,#16149,#16150,#16151,#16152,#16153,#16154,
#16155,#16156,#16157,#16158,#16159,#16160,#16161,#16162,#16163,#16164,#16165,
#16166,#16167,#16168,#16169,#16170,#16171,#16172,#16173,#16174,#16175,#16176,
#16177,#16178,#16179,#16180,#16181,#16182,#16183,#16184,#16185,#16186,#16187,
#16188,#16189,#16190,#16191,#16192,#16193,#16194,#16195,#16196,#16197,#16198,
#16199,#16200,#16201,#16202,#16203,#16204,#16205,#16206,#16207,#16208,#16209,
#16210,#16211,#16212,#16213,#16214,#16215,#16216,#16217,#16218,#16219,#16220,
#16221,#16222,#16223,#16224,#16225,#16226,#16227,#16228,#16229,#16230,#16231,
#16232,#16233,#16234,#16235,#16236,#16237,#16238,#16239,#16240,#16241,#16242,
#16243,#16244,#16245,#16246,#16247,#16248,#16249,#16250,#16251,#16252,#16253,
#16254,#16255,#16256,#16257,#16258,#16259,#16260,#16261,#16262,#16263,#16264,
#16265,#16266,#16267,#16268,#16269,#16270,#16271,#16272,#16273,#16274,#16275,
#16276,#16277,#16278,#16279,#16280,#16281,#16282,#16283,#16284,#16285,#16286,
#16287,#16288,#16289,#16290,#16291,#16292,#16293,#16294,#16295,#16296,#16297,
#16298,#16299,#16300,#16301,#16302,#16303,#16304,#16305,#16306,#16307,#16308,
#16309,#16310,#16311,#16312,#16313,#16314,#16315,#16316,#16317,#16318,#16319,
#16320,#16321,#16322,#16323),.UNSPECIFIED.,.F.,.F.,(4,3,3,3,3,3,3,3,3,3,
3,3,3,3,3,3,3,3,3,3,3,3,3,3,3,3,3,3,3,3,3,3,3,3,3,3,3,3,3,3,3,3,3,3,3,3,
3,3,3,3,3,3,3,3,3,3,3,3,3,3,3,3,3,3,3,3,3,3,3,3,3,3,3,3,3,3,4),(82.7914542042459,
82.8216198633744,82.910193012681,82.9986518057307,83.0870200181033,83.1785763539781,
83.2668429975349,83.3550963881522,83.4433578704206,83.5316487895978,83.6200397751913,
83.7084903634755,83.7970702882138,83.8194707051018,83.9080438544084,83.9965026474582,
84.0848708598308,84.1764271957056,84.2646938392624,84.3529472298798,84.4412087121482,
84.5294996313254,84.6178906169189,84.7063412052032,84.7949211299414,84.8173215468292,
84.9058946961358,84.9943534891855,85.082721701558,85.1742780374329,85.2625446809897,
85.3507980716069,85.4390595538753,85.5273504730524,85.6157414586459,85.7041920469301,
85.7927719716683,85.8151723885566,85.9037455378632,85.9922043309129,86.0805725432855,
86.1721288791603,86.2603955227172,86.3486489133345,86.4369103956028,86.52520131478,
86.6135923003735,86.7020428886577,86.7906228133959,86.813023230284,86.9015963795906,
86.9900551726403,87.0784233850128,87.1699797208877,87.2582463644445,87.3464997550618,
87.4347612373301,87.5230521565073,87.6114431421008,87.699893730385,87.7884736551232,
87.8108740720114,87.8994472213179,87.9879060143677,88.0762742267402,88.167830562615,
88.2560972061718,88.344350596789,88.4326120790573,88.5209029982345,88.609293983828,
88.697744572112,88.7863244968503,88.8087249137388,88.9216441128932,89.0325337049013,
89.0746395112361),.UNSPECIFIED.);
#1262=B_SPLINE_CURVE_WITH_KNOTS('',3,(#16325,#16326,#16327,#16328,#16329,
#16330,#16331,#16332,#16333,#16334),.UNSPECIFIED.,.F.,.F.,(4,1,1,1,1,1,
1,4),(76.5082758295062,76.83451481301,77.8323656547374,78.8302164964648,
79.8280673381922,80.8259181799196,81.823769021647,82.7914500653136),
 .UNSPECIFIED.);
#1263=B_SPLINE_CURVE_WITH_KNOTS('',3,(#16336,#16337,#16338,#16339,#16340,
#16341,#16342,#16343,#16344,#16345,#16346,#16347,#16348,#16349,#16350,#16351,
#16352,#16353,#16354,#16355,#16356,#16357,#16358,#16359,#16360,#16361,#16362,
#16363,#16364,#16365,#16366,#16367,#16368,#16369,#16370,#16371,#16372,#16373,
#16374,#16375,#16376,#16377,#16378,#16379,#16380,#16381,#16382,#16383,#16384,
#16385,#16386,#16387,#16388,#16389,#16390,#16391,#16392,#16393,#16394,#16395,
#16396,#16397,#16398,#16399,#16400,#16401,#16402,#16403,#16404,#16405,#16406,
#16407,#16408,#16409,#16410,#16411,#16412,#16413,#16414,#16415,#16416,#16417,
#16418,#16419,#16420,#16421,#16422,#16423,#16424,#16425,#16426,#16427,#16428,
#16429,#16430,#16431,#16432,#16433,#16434,#16435,#16436,#16437,#16438,#16439,
#16440,#16441,#16442,#16443,#16444,#16445,#16446,#16447,#16448,#16449,#16450,
#16451,#16452,#16453,#16454,#16455,#16456,#16457,#16458,#16459,#16460,#16461,
#16462,#16463,#16464,#16465,#16466,#16467,#16468,#16469,#16470,#16471,#16472,
#16473,#16474,#16475,#16476,#16477,#16478,#16479,#16480,#16481,#16482,#16483,
#16484,#16485,#16486,#16487,#16488,#16489,#16490,#16491,#16492,#16493,#16494,
#16495,#16496,#16497,#16498,#16499,#16500,#16501,#16502,#16503,#16504,#16505,
#16506,#16507,#16508,#16509,#16510,#16511,#16512,#16513,#16514,#16515,#16516,
#16517,#16518,#16519,#16520,#16521,#16522,#16523,#16524,#16525,#16526,#16527,
#16528,#16529,#16530,#16531,#16532,#16533,#16534,#16535,#16536,#16537,#16538,
#16539,#16540,#16541,#16542,#16543,#16544,#16545,#16546,#16547,#16548,#16549,
#16550,#16551,#16552,#16553,#16554,#16555,#16556,#16557,#16558,#16559,#16560,
#16561),.UNSPECIFIED.,.F.,.F.,(4,3,3,3,3,3,3,3,3,3,3,3,3,3,3,3,3,3,3,3,
3,3,3,3,3,3,3,3,3,3,3,3,3,3,3,3,3,3,3,3,3,3,3,3,3,3,3,3,3,3,3,3,3,3,3,3,
3,3,3,3,3,3,3,3,3,3,3,3,3,3,3,3,3,3,3,4),(70.2250835898867,70.3140257139893,
70.4029773741115,70.4919588141693,70.5810544107303,70.6702073895619,70.7595248544879,
70.8474097626456,70.9359829119522,71.0244417050018,71.1128099173743,71.2043662532491,
71.2926328968059,71.3808862874233,71.4691477696917,71.557438688869,71.6458296744625,
71.7342802627467,71.8228601874848,71.845260604373,71.9338337536796,72.0222925467293,
72.1106607591019,72.2022170949768,72.2904837385335,72.3787371291508,72.466998611419,
72.5552895305961,72.6436805161896,72.7321311044739,72.8207110292122,72.8431114461004,
72.931684595407,73.0201433884567,73.1085116008294,73.2000679367042,73.288334580261,
73.3765879708783,73.4648494531465,73.5531403723238,73.6415313579173,73.7299819462015,
73.8185618709397,73.8409622878278,73.9295354371344,74.0179942301841,74.1063624425564,
74.1979187784313,74.2861854219882,74.3744388126055,74.462700294874,74.5509912140511,
74.6393821996446,74.7278327879289,74.816412712667,74.8388131295552,74.9273862788618,
75.0158450719113,75.1042132842839,75.1957696201587,75.2840362637154,75.3722896543324,
75.4605511366011,75.5488420557785,75.637233041372,75.7256836296562,75.8142635543943,
75.8366639712826,75.9250774885632,76.0133803059621,76.1015940720835,76.1897403602782,
76.2778480053841,76.3659320489739,76.4540370202494,76.5082688970663),
 .UNSPECIFIED.);
#1264=B_SPLINE_CURVE_WITH_KNOTS('',3,(#16563,#16564,#16565,#16566,#16567,
#16568,#16569,#16570,#16571,#16572),.UNSPECIFIED.,.F.,.F.,(4,1,1,1,1,1,
1,4),(63.9418982827071,64.8603047122812,65.8581555540086,66.856006395736,
67.8538572374634,68.8517080791908,69.8495589209182,70.2250761086419),
 .UNSPECIFIED.);
#1265=B_SPLINE_CURVE_WITH_KNOTS('',3,(#16574,#16575,#16576,#16577,#16578,
#16579,#16580,#16581,#16582,#16583,#16584),.UNSPECIFIED.,.F.,.F.,(4,1,1,
1,1,1,1,1,4),(57.6587129755275,57.8753488201894,58.8731996619168,59.8710505036442,
60.8689013453716,61.866752187099,62.8646030288264,63.8624538705538,63.9418982827071),
 .UNSPECIFIED.);
#1266=B_SPLINE_CURVE_WITH_KNOTS('',3,(#16586,#16587,#16588,#16589,#16590,
#16591,#16592,#16593,#16594,#16595,#16596,#16597,#16598,#16599,#16600,#16601,
#16602,#16603,#16604,#16605,#16606,#16607,#16608,#16609,#16610,#16611,#16612,
#16613,#16614,#16615,#16616,#16617,#16618,#16619,#16620,#16621,#16622,#16623,
#16624,#16625,#16626,#16627,#16628,#16629,#16630,#16631,#16632,#16633,#16634,
#16635,#16636,#16637,#16638,#16639,#16640,#16641,#16642,#16643,#16644,#16645,
#16646,#16647,#16648,#16649,#16650,#16651,#16652,#16653,#16654,#16655,#16656,
#16657,#16658,#16659,#16660,#16661,#16662,#16663,#16664,#16665,#16666,#16667,
#16668,#16669,#16670,#16671,#16672,#16673,#16674,#16675,#16676,#16677,#16678,
#16679,#16680,#16681,#16682,#16683,#16684,#16685,#16686,#16687,#16688,#16689,
#16690,#16691,#16692,#16693,#16694,#16695,#16696,#16697,#16698,#16699,#16700,
#16701,#16702,#16703,#16704,#16705,#16706,#16707,#16708,#16709,#16710,#16711,
#16712,#16713,#16714,#16715,#16716,#16717,#16718,#16719,#16720,#16721,#16722,
#16723,#16724,#16725,#16726,#16727,#16728,#16729,#16730,#16731,#16732,#16733,
#16734,#16735,#16736,#16737,#16738,#16739,#16740,#16741,#16742,#16743,#16744,
#16745,#16746,#16747,#16748,#16749,#16750,#16751,#16752,#16753,#16754,#16755,
#16756,#16757,#16758,#16759,#16760,#16761,#16762,#16763,#16764,#16765,#16766,
#16767,#16768,#16769,#16770,#16771,#16772,#16773,#16774,#16775,#16776,#16777,
#16778,#16779,#16780,#16781,#16782,#16783,#16784,#16785,#16786,#16787,#16788,
#16789,#16790,#16791,#16792,#16793,#16794,#16795,#16796,#16797,#16798,#16799,
#16800,#16801,#16802,#16803,#16804,#16805,#16806,#16807,#16808,#16809,#16810,
#16811),.UNSPECIFIED.,.F.,.F.,(4,3,3,3,3,3,3,3,3,3,3,3,3,3,3,3,3,3,3,3,
3,3,3,3,3,3,3,3,3,3,3,3,3,3,3,3,3,3,3,3,3,3,3,3,3,3,3,3,3,3,3,3,3,3,3,3,
3,3,3,3,3,3,3,3,3,3,3,3,3,3,3,3,3,3,3,4),(51.3755276683479,51.4674551182634,
51.5594915131789,51.6517320877936,51.7440828937285,51.8366378040778,51.8882437698249,
51.9768169191315,52.0652757121811,52.1536439245537,52.2452002604286,52.3334669039854,
52.4217202946027,52.509981776871,52.5982726960484,52.6866636816419,52.775114269926,
52.8636941946643,52.8860946115523,52.9746677608589,53.0631265539085,53.1514947662813,
53.2430511021561,53.3313177457129,53.4195711363302,53.5078326185985,53.596123537776,
53.6845145233695,53.7729651116536,53.8615450363917,53.8839454532797,53.9725186025863,
54.0609773956361,54.1493456080086,54.2409019438834,54.3291685874402,54.4174219780575,
54.5056834603262,54.5939743795036,54.6823653650971,54.7708159533812,54.8593958781193,
54.8817962950071,54.9703694443136,55.0588282373635,55.1471964497362,55.238752785611,
55.3270194291679,55.4152728197852,55.5035343020536,55.5918252212311,55.6802162068246,
55.7686667951087,55.857246719847,55.8796471367346,55.9682202860412,56.0566790790908,
56.1450472914633,56.2366036273381,56.3248702708951,56.4131236615125,56.5013851437809,
56.589676062958,56.6780670485515,56.7665176368355,56.8550975615738,56.877497978462,
56.9648624461654,57.0520884991057,57.1392356291962,57.2263263599901,57.3133831580112,
57.4004603167863,57.4875438192577,57.5747123789985,57.6587129755275),
 .UNSPECIFIED.);
#1267=B_SPLINE_CURVE_WITH_KNOTS('',3,(#16813,#16814,#16815,#16816,#16817,
#16818,#16819,#16820,#16821,#16822),.UNSPECIFIED.,.F.,.F.,(4,1,1,1,1,1,
1,4),(45.0923466255027,45.9011387194605,46.8989895611879,47.8968404029153,
48.8946912446427,49.8925420863701,50.8903929280975,51.3755266026442),
 .UNSPECIFIED.);
#1268=B_SPLINE_CURVE_WITH_KNOTS('',3,(#16824,#16825,#16826,#16827,#16828,
#16829,#16830,#16831,#16832,#16833,#16834,#16835,#16836,#16837,#16838,#16839,
#16840,#16841,#16842,#16843,#16844,#16845,#16846,#16847,#16848,#16849,#16850,
#16851,#16852,#16853,#16854,#16855,#16856,#16857,#16858,#16859,#16860,#16861,
#16862,#16863,#16864,#16865,#16866,#16867,#16868,#16869,#16870,#16871,#16872,
#16873,#16874,#16875,#16876,#16877,#16878,#16879,#16880,#16881,#16882,#16883,
#16884,#16885,#16886,#16887,#16888,#16889,#16890,#16891,#16892,#16893,#16894,
#16895,#16896,#16897,#16898,#16899,#16900,#16901,#16902,#16903,#16904,#16905,
#16906,#16907,#16908,#16909,#16910,#16911,#16912,#16913,#16914,#16915,#16916,
#16917,#16918,#16919,#16920,#16921,#16922,#16923,#16924,#16925,#16926,#16927,
#16928,#16929,#16930,#16931,#16932,#16933,#16934,#16935,#16936,#16937,#16938,
#16939,#16940,#16941,#16942,#16943,#16944,#16945,#16946,#16947,#16948,#16949,
#16950,#16951,#16952,#16953,#16954,#16955,#16956,#16957,#16958,#16959,#16960,
#16961,#16962,#16963,#16964,#16965,#16966,#16967,#16968,#16969,#16970,#16971,
#16972,#16973,#16974,#16975,#16976,#16977,#16978,#16979,#16980,#16981,#16982,
#16983,#16984,#16985,#16986,#16987,#16988,#16989,#16990,#16991,#16992,#16993,
#16994,#16995,#16996,#16997,#16998,#16999,#17000,#17001,#17002,#17003,#17004,
#17005,#17006,#17007,#17008,#17009,#17010,#17011,#17012,#17013,#17014,#17015,
#17016,#17017,#17018,#17019,#17020,#17021,#17022,#17023,#17024,#17025,#17026,
#17027,#17028,#17029,#17030,#17031,#17032,#17033,#17034,#17035,#17036,#17037,
#17038,#17039,#17040,#17041,#17042,#17043,#17044,#17045,#17046,#17047,#17048,
#17049),.UNSPECIFIED.,.F.,.F.,(4,3,3,3,3,3,3,3,3,3,3,3,3,3,3,3,3,3,3,3,
3,3,3,3,3,3,3,3,3,3,3,3,3,3,3,3,3,3,3,3,3,3,3,3,3,3,3,3,3,3,3,3,3,3,3,3,
3,3,3,3,3,3,3,3,3,3,3,3,3,3,3,3,3,3,3,4),(38.8091570539888,38.9161828273687,
39.0047559766754,39.0932147697253,39.1815829820979,39.2731393179727,39.3614059615296,
39.4496593521471,39.5379208344156,39.6262117535929,39.7146027391865,39.8030533274707,
39.8916332522091,39.9140336690961,40.0026068184027,40.0910656114524,40.179433823825,
40.2709901596998,40.3592568032566,40.4475101938739,40.5357716761421,40.6240625953193,
40.7124535809127,40.8009041691969,40.8894840939351,40.9118845108235,41.00045766013,
41.0889164531798,41.1772846655523,41.2688410014271,41.3571076449839,41.4453610356012,
41.5336225178695,41.6219134370467,41.7103044226401,41.7987550109243,41.8873349356625,
41.9097353525509,41.9983085018575,42.0867672949073,42.1751355072798,42.2666918431546,
42.3549584867115,42.4432118773288,42.5314733595971,42.6197642787743,42.7081552643678,
42.7966058526521,42.8851857773903,42.9075861942783,42.9961593435849,43.0846181366347,
43.1729863490072,43.264542684882,43.3528093284388,43.4410627190561,43.5293242013244,
43.6176151205017,43.7060061060952,43.7944566943794,43.8830366191176,43.9054370360057,
43.9940101853123,44.082468978362,44.1708371907345,44.2623935266093,44.3506601701662,
44.4389135607834,44.5271750430518,44.6154659622291,44.7038569478225,44.7923075361068,
44.880887460845,44.9032878777331,45.0337718756031,45.0923423611683),
 .UNSPECIFIED.);
#1269=B_SPLINE_CURVE_WITH_KNOTS('',3,(#17051,#17052,#17053,#17054,#17055,
#17056,#17057,#17058,#17059,#17060,#17061,#17062,#17063,#17064,#17065,#17066,
#17067,#17068,#17069,#17070,#17071,#17072,#17073,#17074,#17075,#17076,#17077,
#17078,#17079,#17080,#17081,#17082,#17083,#17084,#17085,#17086,#17087,#17088,
#17089,#17090,#17091,#17092,#17093,#17094,#17095,#17096,#17097,#17098,#17099,
#17100,#17101,#17102,#17103,#17104,#17105,#17106,#17107,#17108,#17109,#17110,
#17111,#17112,#17113,#17114,#17115,#17116,#17117,#17118,#17119,#17120,#17121,
#17122,#17123,#17124,#17125,#17126,#17127,#17128,#17129,#17130,#17131,#17132,
#17133,#17134,#17135,#17136,#17137,#17138,#17139,#17140,#17141,#17142,#17143,
#17144,#17145,#17146,#17147,#17148,#17149,#17150,#17151,#17152,#17153,#17154,
#17155,#17156,#17157,#17158,#17159,#17160,#17161,#17162,#17163,#17164,#17165,
#17166,#17167,#17168,#17169,#17170,#17171,#17172,#17173,#17174,#17175,#17176,
#17177,#17178,#17179,#17180,#17181,#17182,#17183,#17184,#17185,#17186,#17187,
#17188,#17189,#17190,#17191,#17192,#17193,#17194,#17195,#17196,#17197,#17198,
#17199,#17200,#17201,#17202,#17203,#17204,#17205,#17206,#17207,#17208,#17209,
#17210,#17211,#17212,#17213,#17214,#17215,#17216,#17217,#17218,#17219,#17220,
#17221,#17222,#17223,#17224,#17225,#17226,#17227,#17228,#17229,#17230,#17231,
#17232,#17233,#17234,#17235,#17236,#17237,#17238,#17239,#17240,#17241,#17242,
#17243,#17244,#17245,#17246,#17247,#17248,#17249,#17250,#17251,#17252,#17253,
#17254,#17255,#17256,#17257,#17258,#17259,#17260,#17261,#17262,#17263,#17264,
#17265,#17266,#17267,#17268,#17269,#17270,#17271,#17272,#17273,#17274,#17275,
#17276),.UNSPECIFIED.,.F.,.F.,(4,3,3,3,3,3,3,3,3,3,3,3,3,3,3,3,3,3,3,3,
3,3,3,3,3,3,3,3,3,3,3,3,3,3,3,3,3,3,3,3,3,3,3,3,3,3,3,3,3,3,3,3,3,3,3,3,
3,3,3,3,3,3,3,3,3,3,3,3,3,3,3,3,3,3,3,4),(32.525971963069,32.6267484165528,
32.7244048484166,32.8267413127105,32.9290777770043,33.0176509263104,33.1061097193596,
33.1944779317316,33.2860342676066,33.3743009111629,33.4625543017797,33.5508157840475,
33.6391067032241,33.7274976888171,33.8159482771008,33.9045282018386,33.9269286187317,
34.0155017680382,34.1039605610878,34.1923287734603,34.2838851093351,34.3721517528918,
34.460405143509,34.5486666257773,34.6369575449543,34.7253485305477,34.8137991188318,
34.9023790435699,34.9247794604591,35.0133526097659,35.1018114028158,35.1901796151886,
35.2817359510633,35.3700025946204,35.4582559852379,35.5465174675064,35.6348083866838,
35.7231993722774,35.8116499605619,35.9002298853003,35.9226303021865,36.011203451493,
36.0996622445427,36.1880304569152,36.27958679279,36.3678534363467,36.456106826964,
36.5443683092322,36.6326592284093,36.7210502140027,36.8095008022868,36.8980807270249,
36.9204811439139,37.0090542932205,37.0975130862702,37.1858812986428,37.2774376345176,
37.3657042780745,37.4539576686918,37.5422191509601,37.6305100701371,37.7189010557306,
37.8073516440148,37.8959315687529,37.9183319856413,38.0057567402233,38.0930680815749,
38.1825792030983,38.269738045414,38.3568657274586,38.4439846320749,38.5352777374967,
38.6224901904464,38.7097513439574,38.79712291786,38.809157053762),
 .UNSPECIFIED.);
#1270=B_SPLINE_CURVE_WITH_KNOTS('',3,(#17278,#17279,#17280,#17281,#17282,
#17283,#17284,#17285,#17286,#17287),.UNSPECIFIED.,.F.,.F.,(4,1,1,1,1,1,
1,4),(26.2427864396296,26.9419727266399,27.9398235683673,28.9376744100947,
29.9355252518221,30.9333760935495,31.9312269352769,32.5259717468092),
 .UNSPECIFIED.);
#1271=B_SPLINE_CURVE_WITH_KNOTS('',3,(#17288,#17289,#17290,#17291,#17292,
#17293,#17294,#17295,#17296,#17297,#17298,#17299,#17300,#17301,#17302,#17303,
#17304,#17305,#17306,#17307,#17308,#17309,#17310,#17311,#17312,#17313,#17314,
#17315,#17316,#17317,#17318,#17319,#17320,#17321,#17322,#17323,#17324,#17325,
#17326,#17327,#17328,#17329,#17330,#17331,#17332,#17333,#17334,#17335,#17336,
#17337,#17338,#17339,#17340,#17341,#17342,#17343,#17344,#17345,#17346,#17347,
#17348,#17349,#17350,#17351,#17352,#17353,#17354,#17355,#17356,#17357,#17358,
#17359,#17360,#17361,#17362,#17363,#17364,#17365,#17366,#17367,#17368,#17369,
#17370,#17371,#17372,#17373,#17374,#17375,#17376,#17377,#17378,#17379,#17380,
#17381,#17382,#17383,#17384,#17385,#17386,#17387,#17388,#17389,#17390,#17391,
#17392,#17393,#17394,#17395,#17396,#17397,#17398,#17399,#17400,#17401,#17402,
#17403,#17404,#17405,#17406,#17407,#17408,#17409,#17410,#17411,#17412,#17413,
#17414,#17415,#17416,#17417,#17418,#17419,#17420,#17421,#17422,#17423,#17424,
#17425,#17426,#17427,#17428,#17429,#17430,#17431,#17432,#17433,#17434,#17435,
#17436,#17437,#17438,#17439,#17440,#17441,#17442,#17443,#17444,#17445,#17446,
#17447,#17448,#17449,#17450,#17451,#17452,#17453,#17454,#17455,#17456,#17457,
#17458,#17459,#17460,#17461,#17462,#17463,#17464,#17465,#17466,#17467,#17468,
#17469,#17470,#17471,#17472,#17473,#17474,#17475,#17476,#17477,#17478,#17479,
#17480,#17481,#17482,#17483,#17484,#17485,#17486),.UNSPECIFIED.,.F.,.F.,
(4,3,3,3,3,3,3,3,3,3,3,3,3,3,3,3,3,3,3,3,3,3,3,3,3,3,3,3,3,3,3,3,3,3,3,
3,3,3,3,3,3,3,3,3,3,3,3,3,3,3,3,3,3,3,3,3,3,3,3,3,3,3,3,3,3,3,4),(20.7587652524469,
20.8471770515305,20.9357172601531,20.9548676762754,21.0434408253141,21.1318996180998,
21.2202678302125,21.3118241661863,21.4000908094954,21.4883441998699,21.5766056819008,
21.664896600846,21.7532875862169,21.8417381742837,21.930318098814,21.9527185180029,
22.0412916665946,22.1297504589173,22.2181186705516,22.3096750066989,22.3979416494941,
22.4861950393424,22.5744565208353,22.6627474392314,22.751138424039,22.8395890115339,
22.9281689354835,22.9505693597303,23.0391425095139,23.1276013030463,23.2159695159069,
23.3075258516008,23.3957924956554,23.4840458867733,23.5723073695444,23.6605982892259,
23.748989275324,23.8374398641133,23.9260197893538,23.9484202014577,24.0369933506891,
24.1254521436636,24.213820355961,24.305376691864,24.3936433353464,24.4818967258899,
24.5701582080845,24.6584491271886,24.7468401127105,24.8352907009236,24.9238706255922,
24.9462710431851,25.0348441924046,25.1233029853661,25.2116711976484,25.3032275335564,
25.3914941770201,25.4797475675431,25.5680090497163,25.6562999687983,25.7446909542951,
25.8331415424822,25.921721467123,25.9441218849125,26.0521117090049,26.1587324119638,
26.2427862611992),.UNSPECIFIED.);
#1272=B_SPLINE_CURVE_WITH_KNOTS('',3,(#17488,#17489,#17490,#17491,#17492,
#17493,#17494,#17495,#17496,#17497,#17498,#17499,#17500,#17501,#17502,#17503,
#17504,#17505,#17506,#17507,#17508,#17509,#17510,#17511,#17512,#17513,#17514,
#17515,#17516,#17517,#17518,#17519,#17520,#17521,#17522,#17523,#17524,#17525,
#17526,#17527,#17528,#17529,#17530,#17531,#17532,#17533,#17534,#17535,#17536,
#17537,#17538,#17539,#17540,#17541,#17542,#17543,#17544,#17545,#17546,#17547,
#17548,#17549,#17550,#17551,#17552,#17553,#17554,#17555,#17556,#17557,#17558,
#17559,#17560,#17561,#17562,#17563,#17564,#17565,#17566,#17567,#17568,#17569,
#17570,#17571,#17572,#17573,#17574,#17575,#17576,#17577,#17578,#17579,#17580,
#17581,#17582,#17583,#17584,#17585,#17586,#17587,#17588,#17589,#17590,#17591,
#17592,#17593,#17594,#17595,#17596,#17597,#17598,#17599,#17600,#17601,#17602,
#17603,#17604,#17605,#17606,#17607,#17608,#17609,#17610,#17611,#17612,#17613,
#17614,#17615,#17616,#17617,#17618,#17619,#17620,#17621,#17622,#17623,#17624,
#17625,#17626,#17627,#17628,#17629,#17630,#17631,#17632,#17633,#17634,#17635,
#17636,#17637,#17638,#17639,#17640,#17641,#17642,#17643,#17644,#17645,#17646,
#17647),.UNSPECIFIED.,.F.,.F.,(4,3,3,3,3,3,3,3,3,3,3,3,3,3,3,3,3,3,3,3,
3,3,3,3,3,3,3,3,3,3,3,3,3,3,3,3,3,3,3,3,3,3,3,3,3,3,3,3,3,3,3,3,3,4),(-22.0660092005583,
-21.9775604397691,-21.9527185180029,-21.8641453689077,-21.7756865760771,
-21.6873183639311,-21.5957620279741,-21.5074953846606,-21.4192419942923,
-21.3309805122783,-21.2426895933606,-21.1542986080331,-21.0658480200188,
-20.9772680955541,-20.9548676762754,-20.8662945236151,-20.7778357272005,
-20.689467511456,-20.5979111768425,-20.5096445299166,-20.421391135937,-20.3331296503169,
-20.2448387278021,-20.1564477389083,-20.0679971473415,-19.979417219372,
-19.957016834548,-19.8684436914371,-19.7799849045778,-19.6916166983834,
-19.6000603601881,-19.5117937227411,-19.4235403381984,-19.3352788619628,
-19.246987948771,-19.1585969690613,-19.0701463866092,-18.9815664675831,
-18.9591659928206,-18.8705928429654,-18.7821340494192,-18.6937658366019,
-18.6022095009133,-18.5139428570424,-18.4256894661595,-18.3374279836741,
-18.2491370643286,-18.160746078639,-18.0722954903006,-17.9837155655689,
-17.9613151510932,-17.8727403843232,-17.7842934699967,-17.7185431288346),
 .UNSPECIFIED.);
#1273=B_SPLINE_CURVE_WITH_KNOTS('',3,(#17648,#17649,#17650,#17651,#17652,
#17653,#17654,#17655,#17656,#17657,#17658,#17659,#17660,#17661,#17662,#17663,
#17664,#17665,#17666,#17667,#17668,#17669,#17670,#17671,#17672,#17673,#17674,
#17675,#17676,#17677,#17678,#17679,#17680,#17681,#17682,#17683,#17684,#17685,
#17686,#17687,#17688,#17689,#17690,#17691,#17692,#17693,#17694,#17695,#17696,
#17697,#17698,#17699,#17700,#17701,#17702,#17703,#17704,#17705,#17706,#17707,
#17708,#17709,#17710,#17711,#17712,#17713,#17714,#17715,#17716,#17717,#17718,
#17719,#17720,#17721,#17722,#17723,#17724,#17725,#17726,#17727,#17728,#17729,
#17730,#17731,#17732,#17733,#17734,#17735,#17736,#17737,#17738,#17739,#17740,
#17741,#17742,#17743,#17744,#17745,#17746,#17747,#17748,#17749,#17750,#17751,
#17752,#17753,#17754,#17755,#17756,#17757,#17758,#17759,#17760,#17761,#17762,
#17763,#17764,#17765,#17766,#17767,#17768,#17769,#17770,#17771,#17772,#17773,
#17774,#17775,#17776,#17777,#17778,#17779,#17780,#17781,#17782,#17783,#17784,
#17785,#17786,#17787,#17788,#17789,#17790,#17791,#17792,#17793,#17794,#17795,
#17796,#17797,#17798,#17799,#17800,#17801,#17802,#17803,#17804),
 .UNSPECIFIED.,.F.,.F.,(4,3,3,3,3,3,3,3,3,3,3,3,3,3,3,3,3,3,3,3,3,3,3,3,
3,3,3,3,3,3,3,3,3,3,3,3,3,3,3,3,3,3,3,3,3,3,3,3,3,3,3,3,4),(14.7355974371875,
14.8240238515058,14.9125887089936,14.967762625911,15.0563357887042,15.1447945957911,
15.2331628227319,15.3247191533452,15.4129858127104,15.5012392195697,15.5895007184981,
15.6777916547382,15.7661826579098,15.8546332640942,15.9432132070692,15.9656134676384,
16.0541865737118,16.1426453228713,16.231013490753,16.3225698430796,16.4108364409255,
16.4990897854578,16.5873512213152,16.6756420938033,16.7640330325289,16.8524835737835,
16.9410634516159,16.9634643093658,17.0520374794408,17.1404962934807,17.2288645270386,
17.3204208550455,17.4086875201402,17.496940932389,17.5852024363594,17.6734933772864,
17.7618843845908,17.8503349945898,17.9389149408814,17.9613151510932,18.0498883004087,
18.1383470935207,18.2267153060082,18.3182716418598,18.4065382856639,18.4947916765772,
18.5830531591902,18.6713440787606,18.7597350648179,18.8481856536076,18.936765578909,
18.9591659928206,18.9739239990975),.UNSPECIFIED.);
#1274=B_SPLINE_CURVE_WITH_KNOTS('',3,(#17806,#17807,#17808,#17809,#17810,
#17811,#17812,#17813),.UNSPECIFIED.,.F.,.F.,(4,1,1,1,1,4),(-15.5984662374724,
-14.967762625911,-13.9699117841836,-12.9720609424562,-11.9742101007288,
-11.4361522655988),.UNSPECIFIED.);
#1275=B_SPLINE_CURVE_WITH_KNOTS('',3,(#17814,#17815,#17816,#17817,#17818,
#17819,#17820,#17821),.UNSPECIFIED.,.F.,.F.,(4,1,1,1,1,4),(8.45339075667584,
8.98065757554662,9.97850841727402,10.9763592590014,11.9742101007288,12.615721686902),
 .UNSPECIFIED.);
#1276=B_SPLINE_CURVE_WITH_KNOTS('',3,(#17823,#17824,#17825,#17826,#17827,
#17828,#17829,#17830),.UNSPECIFIED.,.F.,.F.,(4,1,1,1,1,4),(-9.31667937974296,
-8.98065757554662,-7.98280673381922,-6.98495589209182,-5.98710505036441,
-5.15395682855483),.UNSPECIFIED.);
#1277=B_SPLINE_CURVE_WITH_KNOTS('',3,(#17831,#17832,#17833,#17834,#17835,
#17836,#17837,#17838,#17839,#17840,#17841,#17842,#17843,#17844,#17845,#17846,
#17847,#17848,#17849,#17850,#17851,#17852,#17853,#17854,#17855,#17856,#17857,
#17858,#17859,#17860,#17861,#17862,#17863,#17864,#17865,#17866,#17867,#17868,
#17869,#17870,#17871,#17872,#17873,#17874,#17875,#17876,#17877,#17878,#17879,
#17880,#17881,#17882,#17883,#17884,#17885,#17886,#17887,#17888,#17889,#17890,
#17891,#17892,#17893,#17894,#17895,#17896,#17897,#17898,#17899,#17900,#17901,
#17902,#17903,#17904,#17905,#17906,#17907,#17908,#17909,#17910,#17911,#17912,
#17913,#17914,#17915,#17916,#17917,#17918,#17919,#17920,#17921,#17922,#17923,
#17924,#17925,#17926,#17927,#17928,#17929,#17930,#17931,#17932,#17933,#17934,
#17935,#17936,#17937,#17938,#17939,#17940,#17941,#17942,#17943,#17944,#17945,
#17946,#17947,#17948,#17949,#17950,#17951,#17952,#17953,#17954,#17955,#17956,
#17957,#17958,#17959,#17960,#17961,#17962,#17963,#17964,#17965,#17966,#17967,
#17968,#17969,#17970,#17971,#17972,#17973,#17974,#17975,#17976,#17977,#17978,
#17979,#17980,#17981),.UNSPECIFIED.,.F.,.F.,(4,3,3,3,3,3,3,3,3,3,3,3,3,
3,3,3,3,3,3,3,3,3,3,3,3,3,3,3,3,3,3,3,3,3,3,3,3,3,3,3,3,3,3,3,3,3,3,3,3,
3,4),(2.17031737188971,2.25881290186963,2.3506553547837,2.43904646041468,
2.52742311294194,2.61580651482276,2.70421786808851,2.79272702145135,2.881294244772,
2.96998899437975,2.99355252518221,3.08227858874621,3.17089309169939,3.2594196018157,
3.35091757245244,3.4393479542858,3.52776681491773,3.61619532292152,3.70465464856639,
3.79321523827935,3.88183633344943,3.9705867777702,3.99140336690961,4.07986039758296,
4.1682016225605,4.25645096449381,4.34805137001171,4.43619662711166,4.52432790356672,
4.61246666977451,4.70063439648283,4.78890209727742,4.87722919356262,4.96568627168405,
4.98925420863701,5.07785161744967,5.16633476132244,5.25472738550838,5.34627459361539,
5.4345656425618,5.52284339355104,5.61112916442565,5.69944427361828,5.78785917964294,
5.87633356002678,5.96493690510802,5.98710505036441,6.0756768503468,6.16414887291111,
6.25252666002196,6.33364065268233),.UNSPECIFIED.);
#1278=B_SPLINE_CURVE_WITH_KNOTS('',3,(#18506,#18507,#18508,#18509,#18510,
#18511,#18512,#18513,#18514,#18515,#18516,#18517,#18518,#18519,#18520,#18521,
#18522,#18523,#18524,#18525,#18526,#18527,#18528,#18529,#18530,#18531,#18532,
#18533,#18534,#18535,#18536,#18537,#18538,#18539,#18540,#18541,#18542,#18543,
#18544,#18545,#18546,#18547,#18548,#18549,#18550,#18551,#18552,#18553,#18554,
#18555,#18556,#18557,#18558,#18559,#18560,#18561,#18562,#18563,#18564,#18565,
#18566,#18567,#18568,#18569,#18570,#18571,#18572,#18573,#18574,#18575,#18576,
#18577,#18578,#18579,#18580,#18581,#18582,#18583,#18584,#18585,#18586,#18587,
#18588,#18589,#18590,#18591,#18592,#18593,#18594,#18595,#18596,#18597,#18598,
#18599,#18600,#18601,#18602,#18603,#18604,#18605,#18606,#18607,#18608,#18609,
#18610,#18611,#18612,#18613,#18614,#18615,#18616,#18617,#18618,#18619,#18620,
#18621,#18622,#18623,#18624,#18625,#18626,#18627,#18628,#18629,#18630,#18631,
#18632,#18633,#18634,#18635,#18636,#18637,#18638,#18639,#18640,#18641,#18642,
#18643,#18644,#18645,#18646,#18647,#18648,#18649,#18650,#18651,#18652,#18653,
#18654,#18655,#18656,#18657,#18658,#18659,#18660,#18661,#18662,#18663,#18664,
#18665,#18666,#18667,#18668,#18669,#18670,#18671,#18672,#18673,#18674,#18675,
#18676,#18677,#18678,#18679,#18680,#18681,#18682,#18683,#18684,#18685,#18686,
#18687,#18688,#18689,#18690,#18691,#18692,#18693,#18694,#18695,#18696,#18697,
#18698,#18699,#18700,#18701,#18702,#18703,#18704,#18705,#18706,#18707,#18708,
#18709,#18710,#18711,#18712,#18713,#18714,#18715,#18716,#18717,#18718,#18719,
#18720,#18721,#18722,#18723),.UNSPECIFIED.,.F.,.F.,(4,2,2,2,2,2,2,2,2,2,
2,2,2,2,2,2,2,2,2,2,2,2,2,2,2,2,2,2,2,2,2,2,2,2,2,2,2,2,2,2,2,2,2,2,2,2,
2,2,2,2,2,2,2,2,2,2,2,2,2,2,2,2,2,2,2,2,2,2,2,2,2,2,2,2,2,2,2,2,2,2,2,2,
2,2,2,2,2,2,2,2,2,2,2,2,2,2,2,2,2,2,2,2,2,2,2,2,2,2,4),(2.03132451219564,
2.04771864970936,2.054188022303,2.05814698897628,2.06242056802813,2.06823430844965,
2.0817897698534,2.10064397805793,2.20370857919037,2.21377989580146,2.2175320623633,
2.21976390896051,2.22218884705627,2.22568143858123,2.23475090456857,2.24835366133737,
2.29485606209288,2.35966392834093,2.37095468450181,2.37708768999893,2.38137662830883,
2.38577408674184,2.39223546346006,2.41005207867283,2.43732461440137,2.47913470812155,
2.52862412889425,2.53674984560304,2.5398555957629,2.54208109135899,2.54451148219816,
2.54803239165717,2.55729118947681,2.57127885605092,2.66996057549393,2.69116499558442,
2.69828760099901,2.70282479670568,2.70707904550392,2.7127763701719,2.72565665508832,
2.74329096533933,2.82738094384854,2.85559067256685,2.86037638324324,2.8633657240369,
2.86571845065722,2.86850779348139,2.87368300521173,2.90475334948206,2.96883722346092,
3.01038229618799,3.01827447807536,3.0234318638587,3.02762204312451,3.03245205411302,
3.04091676178286,3.08275717061232,3.13996540164022,3.17740586865857,3.18242954396431,
3.18545724954237,3.18781739862515,3.1905431584796,3.19542278361477,3.21981157227677,
3.26857495939193,3.33197371593967,3.34020907084036,3.34547079137238,3.34966884535167,
3.35442483817035,3.36254901686561,3.39818868269499,3.44478912959587,3.49560784772432,
3.50370000263359,3.50680089198984,3.50902485831906,3.51145585347853,3.51498141809216,
3.52427414349188,3.53833208109676,3.63881185324464,3.65849253024262,3.66541756413956,
3.66991152965345,3.6741845443711,3.67967676578006,3.69226103363765,3.70951482656912,
3.75794415447515,3.81824270779646,3.82611542164801,3.82918325833868,3.83139835011756,
3.83383707614073,3.83740312448355,3.846974911804,3.90962690510115,3.94173461786071,
3.97769715987629,3.98606014211005,3.99091632105627,3.99510351997158,3.99911650182043,
4.00412635044493,4.01174920751113,4.06083740610103),.UNSPECIFIED.);
#1279=B_SPLINE_CURVE_WITH_KNOTS('',3,(#18725,#18726,#18727,#18728),
 .UNSPECIFIED.,.F.,.F.,(4,4),(0.,0.0148042672212818),.UNSPECIFIED.);
#1280=B_SPLINE_CURVE_WITH_KNOTS('',3,(#18729,#18730,#18731,#18732,#18733,
#18734,#18735,#18736,#18737,#18738,#18739,#18740,#18741,#18742,#18743,#18744,
#18745,#18746,#18747,#18748,#18749,#18750,#18751,#18752,#18753,#18754,#18755,
#18756,#18757,#18758,#18759,#18760,#18761,#18762,#18763,#18764,#18765,#18766,
#18767,#18768,#18769,#18770,#18771,#18772,#18773,#18774,#18775,#18776,#18777,
#18778,#18779,#18780,#18781,#18782,#18783,#18784,#18785,#18786,#18787,#18788,
#18789,#18790,#18791,#18792,#18793,#18794,#18795,#18796,#18797,#18798,#18799,
#18800,#18801,#18802,#18803,#18804,#18805,#18806,#18807,#18808,#18809,#18810,
#18811,#18812,#18813,#18814,#18815,#18816,#18817,#18818,#18819),
 .UNSPECIFIED.,.F.,.F.,(4,3,3,3,3,3,3,3,3,3,3,3,3,3,3,3,3,3,3,3,3,3,3,3,
3,3,3,3,3,3,4),(0.,0.0213307452137482,0.0521561464407917,0.0839669760524937,
0.115759968726801,0.125948380810053,0.130779959365576,0.163494710583772,
0.196733919866297,0.230225396295248,0.259366443292864,0.264034736052148,
0.29841870568857,0.33269054668832,0.364788977591868,0.388319089517784,0.395090312303456,
0.401763820706065,0.435663949756398,0.470194310390573,0.505432883798703,
0.534520684831987,0.540918384207332,0.546655482151201,0.582601778959208,
0.618814597237711,0.635163545672189,0.641284826970611,0.678126477849349,
0.714525403155029,0.741270768406514),.UNSPECIFIED.);
#1281=B_SPLINE_CURVE_WITH_KNOTS('',3,(#19344,#19345,#19346,#19347,#19348,
#19349,#19350,#19351,#19352,#19353,#19354,#19355,#19356,#19357,#19358,#19359,
#19360,#19361,#19362,#19363,#19364,#19365,#19366,#19367,#19368,#19369,#19370,
#19371,#19372,#19373,#19374,#19375,#19376,#19377,#19378,#19379,#19380,#19381,
#19382,#19383,#19384,#19385,#19386,#19387,#19388,#19389,#19390,#19391,#19392,
#19393,#19394,#19395,#19396,#19397,#19398,#19399,#19400,#19401,#19402,#19403,
#19404,#19405,#19406,#19407,#19408,#19409,#19410,#19411,#19412,#19413,#19414,
#19415,#19416,#19417,#19418,#19419,#19420,#19421,#19422,#19423,#19424,#19425,
#19426,#19427,#19428,#19429,#19430,#19431,#19432,#19433,#19434,#19435,#19436,
#19437,#19438,#19439,#19440,#19441,#19442,#19443,#19444,#19445,#19446,#19447,
#19448,#19449,#19450,#19451,#19452,#19453,#19454,#19455,#19456,#19457,#19458,
#19459,#19460,#19461,#19462,#19463,#19464,#19465,#19466,#19467,#19468,#19469,
#19470,#19471,#19472,#19473,#19474,#19475,#19476,#19477,#19478,#19479,#19480,
#19481,#19482,#19483,#19484,#19485,#19486,#19487,#19488,#19489,#19490,#19491,
#19492,#19493,#19494,#19495,#19496,#19497),.UNSPECIFIED.,.F.,.F.,(4,2,2,
2,2,2,2,2,2,2,2,2,2,2,2,2,2,2,2,2,2,2,2,2,2,2,2,2,2,2,2,2,2,2,2,2,2,2,2,
2,2,2,2,2,2,2,2,2,2,2,2,2,2,2,2,2,2,2,2,2,2,2,2,2,2,2,2,2,2,2,2,2,2,2,2,
2,4),(2.29812698965297,2.33178680710208,2.343698682039,2.34771175618191,
2.34999527417306,2.35238664207991,2.35568912049544,2.36356174417911,2.3748249844316,
2.40834603517596,2.49226078206667,2.50344108419059,2.50882799377206,2.51304041355705,
2.51772388540368,2.52551066317873,2.55623450036125,2.62236224341244,2.66323886779315,
2.66831369188992,2.67135690112496,2.67371951851705,2.67643689399347,2.68127497132266,
2.70487603980923,2.7678565060481,2.81805201859086,2.82623901100133,2.83148711299157,
2.83568535443051,2.84045343806509,2.8486280427595,2.88505451296413,2.9338179921185,
2.959078252197,2.98619587606192,2.99093747377553,2.9939139741472,2.99626654178504,
2.99906750127949,3.00429517840024,3.03683769124635,3.10535480575199,3.14147168447426,
3.14984779067923,3.15470844716903,3.15889763575437,3.16401895218815,3.17386136502113,
3.18634501935978,3.21531750118195,3.28203716994859,3.30859430794303,3.31331295715945,
3.31628247771575,3.31863458179563,3.32144100135327,3.32669476223459,3.36004089016106,
3.42920761730249,3.46398461360625,3.47227227587684,3.47711271054028,3.48088407589505,
3.48584648937806,3.49492658587954,3.55653966581214,3.62216199348397,3.63341098950873,
3.63733435388478,3.63959987208859,3.64200085564126,3.6453620190887,3.65359162423786,
3.66553623385595,3.70250391739545,3.75982114661551),.UNSPECIFIED.);
#1282=B_SPLINE_CURVE_WITH_KNOTS('',3,(#20022,#20023,#20024,#20025,#20026,
#20027,#20028,#20029,#20030,#20031,#20032,#20033,#20034,#20035,#20036,#20037,
#20038,#20039,#20040,#20041,#20042,#20043,#20044,#20045,#20046,#20047,#20048,
#20049,#20050,#20051,#20052,#20053,#20054,#20055,#20056,#20057,#20058,#20059,
#20060,#20061,#20062,#20063,#20064,#20065,#20066,#20067,#20068,#20069,#20070,
#20071,#20072,#20073,#20074,#20075,#20076,#20077,#20078,#20079,#20080,#20081,
#20082,#20083,#20084,#20085,#20086,#20087,#20088,#20089,#20090,#20091,#20092,
#20093,#20094,#20095,#20096,#20097,#20098,#20099,#20100,#20101,#20102,#20103,
#20104,#20105,#20106,#20107,#20108,#20109,#20110,#20111,#20112,#20113,#20114,
#20115,#20116,#20117,#20118,#20119,#20120,#20121,#20122,#20123,#20124,#20125,
#20126,#20127,#20128,#20129,#20130,#20131,#20132,#20133,#20134,#20135,#20136,
#20137,#20138,#20139,#20140,#20141,#20142,#20143,#20144,#20145,#20146,#20147,
#20148,#20149,#20150,#20151,#20152,#20153,#20154,#20155,#20156,#20157,#20158,
#20159,#20160,#20161,#20162,#20163,#20164,#20165,#20166,#20167,#20168,#20169,
#20170,#20171,#20172,#20173,#20174,#20175,#20176,#20177,#20178,#20179,#20180,
#20181,#20182,#20183,#20184,#20185,#20186,#20187,#20188,#20189,#20190,#20191,
#20192,#20193,#20194,#20195,#20196,#20197,#20198,#20199,#20200,#20201,#20202,
#20203,#20204,#20205,#20206,#20207,#20208,#20209,#20210,#20211,#20212,#20213),
 .UNSPECIFIED.,.F.,.F.,(4,2,2,2,2,2,2,2,2,2,2,2,2,2,2,2,2,2,2,2,2,2,2,2,
2,2,2,2,2,2,2,2,2,2,2,2,2,2,2,2,2,2,2,2,2,2,2,2,2,2,2,2,2,2,2,2,2,2,2,2,
2,2,2,2,2,2,2,2,2,2,2,2,2,2,2,2,2,2,2,2,2,2,2,2,2,2,2,2,2,2,2,2,2,2,2,4),
(0.302215230993473,0.329128974360592,0.357185769673646,0.369402245040697,
0.378989406177068,0.384033554243151,0.384070159127476,0.384109313688677,
0.384151204849934,0.384196034379097,0.384244020179286,0.384295397705355,
0.384350421504573,0.384409366917275,0.38447253189265,0.384540238998633,
0.384612837573121,0.384690706047362,0.38477425445222,0.38486392706983,0.384960205242976,
0.385037539250905,0.385146049371129,0.385298292617762,0.38570222586489,
0.389955650760635,0.395543788853112,0.408146525352725,0.469715663524433,
0.531966096927452,0.541753248185602,0.545351210882397,0.54779720883181,
0.550007524781269,0.553054116064316,0.560795258722229,0.623382942899022,
0.692052308270695,0.701577049809445,0.706632611330204,0.710779313113456,
0.71567933677062,0.724230157428683,0.763480756018339,0.829501312458737,
0.861061657216598,0.866254908924068,0.869048392518178,0.871401214228517,
0.874386379678638,0.879157445918688,0.906988701133725,0.931748156993207,
0.97165600671502,1.00107308561578,1.01368393066366,1.02360457088653,1.0287417232672,
1.03293155613221,1.0377791516955,1.04609847437421,1.08134226978856,1.08754697792447,
1.15217797306174,1.18337278354229,1.18855307273335,1.19134383270273,1.19369694614796,
1.19668576131112,1.20146875606336,1.22958768252735,1.31383767257273,1.34048421317768,
1.34792998110663,1.35253816827687,1.35676831414208,1.36220736758336,1.37398064730734,
1.45268733617976,1.48931711425151,1.50119642118929,1.50939260987216,1.51274819502265,
1.51514813521365,1.51741522950933,1.52134645457812,1.53265220593135,1.59824802683231,
1.639724373617,1.66340376052312,1.67056196732202,1.67510762657115,1.67935991591873,
1.68494150859781,1.69750740525998,1.73011464129713),.UNSPECIFIED.);
#1283=B_SPLINE_CURVE_WITH_KNOTS('',3,(#20738,#20739,#20740,#20741,#20742,
#20743,#20744,#20745,#20746,#20747,#20748,#20749,#20750,#20751,#20752,#20753,
#20754,#20755,#20756,#20757,#20758,#20759,#20760,#20761,#20762,#20763,#20764,
#20765,#20766,#20767,#20768,#20769,#20770,#20771,#20772,#20773,#20774,#20775,
#20776,#20777,#20778,#20779,#20780,#20781,#20782,#20783,#20784,#20785,#20786,
#20787,#20788,#20789,#20790,#20791,#20792,#20793,#20794,#20795,#20796,#20797,
#20798,#20799,#20800,#20801,#20802,#20803,#20804,#20805,#20806,#20807,#20808,
#20809,#20810,#20811,#20812,#20813,#20814,#20815,#20816,#20817,#20818,#20819,
#20820,#20821,#20822,#20823,#20824,#20825,#20826,#20827,#20828,#20829,#20830,
#20831,#20832,#20833,#20834,#20835,#20836,#20837,#20838,#20839,#20840,#20841,
#20842,#20843,#20844,#20845,#20846,#20847,#20848,#20849,#20850,#20851,#20852,
#20853,#20854,#20855,#20856,#20857,#20858,#20859,#20860,#20861,#20862,#20863,
#20864,#20865,#20866,#20867,#20868,#20869,#20870,#20871,#20872,#20873,#20874,
#20875,#20876,#20877,#20878,#20879),.UNSPECIFIED.,.F.,.F.,(4,2,2,2,2,2,
2,2,2,2,2,2,2,2,2,2,2,2,2,2,2,2,2,2,2,2,2,2,2,2,2,2,2,2,2,2,2,2,2,2,2,2,
2,2,2,2,2,2,2,2,2,2,2,2,2,2,2,2,2,2,2,2,2,2,2,2,2,2,2,2,4),(2.33187697907722,
2.34000409178357,2.38271068663288,2.45303195363635,2.4732949170467,2.47808089597807,
2.48081495411595,2.48315271451519,2.48620928169482,2.4927041936187,2.54881461406063,
2.62166647798696,2.63268654209339,2.63814233847343,2.64211218048268,2.6463809720684,
2.65215891201936,2.66549643523321,2.68395147161456,2.73857417766915,2.74988897894658,
2.79414139013763,2.79972351460422,2.80263449545506,2.80498264728649,2.8078354289298,
2.8133218128894,2.85661449696997,2.92558724271068,2.95159091325247,2.95925084758828,
2.96390227143753,2.96811417032225,2.97353992920464,2.98494856249953,3.0297196538535,
3.08424430961922,3.11673561973802,3.12166499252487,3.1246957183138,3.12704994809193,
3.12980514136111,3.13482312746102,3.16204370662117,3.25733726872406,3.27586210312986,
3.28262899631771,3.28664460702511,3.29088640159593,3.29649699748084,3.30888401877498,
3.3256454764821,3.37173253357554,3.43546188845268,3.44314074139632,3.44617931693045,
3.44838928742662,3.45084813917423,3.45447784087544,3.46443143634096,3.52924641917268,
3.59293790347914,3.60116373260668,3.60642876603047,3.61063580943842,3.61540899080695,
3.62358055265985,3.65978812734178,3.7078645478554,3.75667841923273,3.75929980855926),
 .UNSPECIFIED.);
#1284=B_SPLINE_CURVE_WITH_KNOTS('',3,(#20881,#20882,#20883,#20884,#20885,
#20886,#20887,#20888,#20889,#20890,#20891,#20892,#20893,#20894,#20895,#20896,
#20897,#20898,#20899,#20900,#20901,#20902,#20903,#20904,#20905,#20906,#20907,
#20908,#20909,#20910,#20911,#20912,#20913,#20914,#20915,#20916,#20917,#20918,
#20919,#20920,#20921,#20922,#20923,#20924,#20925,#20926,#20927,#20928,#20929,
#20930,#20931,#20932,#20933,#20934,#20935,#20936,#20937,#20938,#20939,#20940,
#20941,#20942,#20943,#20944,#20945,#20946,#20947,#20948,#20949,#20950,#20951,
#20952,#20953,#20954,#20955,#20956,#20957,#20958,#20959,#20960,#20961,#20962,
#20963,#20964,#20965,#20966,#20967,#20968,#20969,#20970,#20971,#20972,#20973,
#20974,#20975,#20976,#20977,#20978,#20979,#20980,#20981,#20982,#20983,#20984,
#20985,#20986,#20987,#20988,#20989,#20990,#20991,#20992,#20993,#20994,#20995,
#20996,#20997,#20998,#20999,#21000,#21001,#21002,#21003,#21004,#21005,#21006,
#21007,#21008,#21009,#21010,#21011,#21012,#21013,#21014,#21015,#21016,#21017,
#21018,#21019,#21020,#21021,#21022,#21023,#21024,#21025,#21026,#21027,#21028,
#21029,#21030,#21031,#21032,#21033,#21034,#21035,#21036,#21037,#21038,#21039,
#21040,#21041,#21042,#21043,#21044,#21045,#21046,#21047,#21048,#21049,#21050,
#21051,#21052,#21053,#21054,#21055,#21056,#21057,#21058,#21059,#21060,#21061,
#21062,#21063,#21064,#21065,#21066,#21067,#21068,#21069,#21070,#21071,#21072,
#21073,#21074,#21075,#21076,#21077,#21078,#21079,#21080,#21081,#21082,#21083,
#21084,#21085,#21086),.UNSPECIFIED.,.F.,.F.,(4,2,2,2,2,2,2,2,2,2,2,2,2,
2,2,2,2,2,2,2,2,2,2,2,2,2,2,2,2,2,2,2,2,2,2,2,2,2,2,2,2,2,2,2,2,2,2,2,2,
2,2,2,2,2,2,2,2,2,2,2,2,2,2,2,2,2,2,2,2,2,2,2,2,2,2,2,2,2,2,2,2,2,2,2,2,
2,2,2,2,2,2,2,2,2,2,2,2,2,2,2,2,2,4),(2.03100183139203,2.0311472448286,
2.0622708037727,2.1307986436883,2.15265245736636,2.15754705736789,2.16030608582901,
2.16266263124956,2.16569484294027,2.17206554650664,2.18061445438363,2.20241417761017,
2.27029695476723,2.30728161376276,2.31571320665052,2.32058659138894,2.32477522958079,
2.32988143952482,2.33964953485503,2.40420335186027,2.47074499864376,2.47827448833059,
2.48128558801495,2.48348706779254,2.48594361662004,2.48959206774801,2.4997379536851,
2.56782034138872,2.62855310475401,2.63682059551014,2.64209294234794,2.64629318834684,
2.65104495693733,2.65914525368751,2.69437508074936,2.7729750427622,2.7971826404337,
2.80177646559555,2.80470824980164,2.80705889596875,2.80989786529937,2.81530591202188,
2.85434264552798,2.87971731437408,2.94566451311948,2.95801528969989,2.96314115027234,
2.96741918288954,2.97183251333061,2.97836829542996,2.99673365855859,3.02518936748285,
3.08614823250679,3.11885393924503,3.12379461090875,3.12683074091925,3.12918757736804,
3.13194371636431,3.13696141444024,3.16413342245865,3.25880189067027,3.27776297334542,
3.2845907817082,3.28861788340449,3.29285389393087,3.29842669702448,3.31060588700989,
3.36167721604079,3.41666941594778,3.44179447666789,3.44643354893427,3.449378812166,
3.45172954565832,3.4545557543779,3.45990431575374,3.49653725141768,3.58560785748541,
3.60121535936558,3.60753736150401,3.61146953061622,3.61576432738407,3.62169840492567,
3.63597792093371,3.70314519568518,3.75950691993871,3.76752008821574,3.77061012087802,
3.77283141818765,3.77521681384309,3.77850114381141,3.78236976497366,3.78931156482314,
3.80535352678214,3.8519522794886,3.91259087507341,3.92515931254135,3.93074093028329,
3.93499279186394,3.93953756523577,3.94669347964855,3.97035732895371,4.01178858053361,
4.06070745563291),.UNSPECIFIED.);
#1285=B_SPLINE_CURVE_WITH_KNOTS('',3,(#21088,#21089,#21090,#21091,#21092,
#21093,#21094,#21095,#21096,#21097,#21098,#21099,#21100,#21101,#21102,#21103,
#21104,#21105,#21106,#21107,#21108,#21109,#21110,#21111,#21112,#21113,#21114,
#21115,#21116,#21117,#21118,#21119,#21120,#21121,#21122,#21123,#21124,#21125,
#21126,#21127,#21128,#21129,#21130,#21131,#21132,#21133,#21134,#21135,#21136,
#21137,#21138,#21139,#21140,#21141,#21142,#21143,#21144,#21145,#21146,#21147,
#21148,#21149,#21150,#21151,#21152,#21153,#21154,#21155,#21156,#21157,#21158,
#21159,#21160,#21161,#21162,#21163,#21164,#21165,#21166,#21167,#21168,#21169,
#21170,#21171,#21172,#21173,#21174,#21175,#21176,#21177,#21178,#21179,#21180,
#21181,#21182,#21183,#21184,#21185,#21186,#21187,#21188,#21189,#21190,#21191,
#21192,#21193,#21194,#21195,#21196,#21197,#21198,#21199,#21200,#21201,#21202,
#21203,#21204,#21205,#21206,#21207,#21208,#21209,#21210,#21211,#21212,#21213,
#21214,#21215,#21216,#21217,#21218,#21219,#21220,#21221,#21222,#21223,#21224,
#21225,#21226,#21227,#21228,#21229,#21230,#21231,#21232,#21233,#21234,#21235,
#21236,#21237,#21238,#21239,#21240,#21241,#21242,#21243,#21244,#21245,#21246,
#21247,#21248,#21249,#21250,#21251,#21252,#21253,#21254,#21255,#21256,#21257),
 .UNSPECIFIED.,.F.,.F.,(4,2,2,2,2,2,2,2,2,2,2,2,2,2,2,2,2,2,2,2,2,2,2,2,
2,2,2,2,2,2,2,2,2,2,2,2,2,2,2,2,2,2,2,2,2,2,2,2,2,2,2,2,2,2,2,2,2,2,2,2,
2,2,2,2,2,2,2,2,2,2,2,2,2,2,2,2,2,2,2,2,2,2,2,2,4),(2.33214412619499,2.34314390748205,
2.34815976670484,2.35118603662359,2.35354714568822,2.35627647635811,2.36116839331613,
2.38575313385532,2.4344059690819,2.49775933657462,2.5059987165985,2.5112631569145,
2.51546348242276,2.52022216312754,2.52835123624104,2.56401913740978,2.61067247325097,
2.66146448119969,2.66956051740221,2.67266301938936,2.67488817530125,2.67732052144944,
2.68084815180698,2.69014696781106,2.70421481321656,2.80483048721128,2.82444188424143,
2.83136009644012,2.8358542296935,2.8401307355468,2.84595562003803,2.85957060127714,
2.87853203977876,2.97998146077599,2.99115573880753,2.9950692164851,2.99733307911335,
2.99973585156921,3.0031052138381,3.01138290597708,3.02341961134417,3.06086763776495,
3.13838682435815,3.14910298331414,3.15448450492669,3.15843564724393,3.16271800332851,
3.16857468337451,3.18237669982729,3.20168124026125,3.25854126081562,3.28358938223161,
3.31100908242314,3.31576364870506,3.3187442189316,3.3210972553409,3.32389553658596,
3.32910974010845,3.36124235303482,3.42893272730556,3.4661794014146,3.47462562401882,
3.47950250916065,3.48369122997518,3.48879388304669,3.49854374588661,3.56253348743775,
3.62976256051955,3.63723535957617,3.6402368847183,3.64243606917896,3.64489574106813,
3.64855867656192,3.65880894340948,3.67487898764247,3.74027143458282,3.78777384684983,
3.79588402007578,3.80110894017101,3.8053054379871,3.80924984992859,3.81598532022518,
3.83818153678218,3.87584990582865,3.88120708400659),.UNSPECIFIED.);
#1286=B_SPLINE_CURVE_WITH_KNOTS('',3,(#21259,#21260,#21261,#21262,#21263,
#21264,#21265,#21266,#21267,#21268,#21269,#21270,#21271,#21272,#21273,#21274,
#21275,#21276,#21277,#21278,#21279,#21280,#21281,#21282,#21283,#21284,#21285,
#21286,#21287,#21288,#21289,#21290,#21291,#21292,#21293,#21294,#21295,#21296,
#21297,#21298,#21299,#21300,#21301,#21302,#21303,#21304,#21305,#21306,#21307,
#21308,#21309,#21310,#21311,#21312,#21313,#21314,#21315,#21316,#21317,#21318,
#21319,#21320,#21321,#21322,#21323,#21324,#21325,#21326,#21327,#21328,#21329,
#21330,#21331,#21332,#21333,#21334,#21335,#21336,#21337,#21338,#21339,#21340,
#21341,#21342,#21343,#21344,#21345,#21346,#21347,#21348,#21349,#21350,#21351,
#21352,#21353,#21354,#21355,#21356,#21357,#21358,#21359,#21360,#21361,#21362,
#21363,#21364,#21365,#21366,#21367,#21368,#21369,#21370,#21371,#21372,#21373,
#21374,#21375,#21376,#21377,#21378,#21379,#21380,#21381,#21382,#21383,#21384,
#21385,#21386,#21387,#21388,#21389,#21390,#21391,#21392,#21393,#21394,#21395,
#21396,#21397,#21398,#21399,#21400,#21401,#21402,#21403,#21404,#21405,#21406,
#21407,#21408,#21409,#21410),.UNSPECIFIED.,.F.,.F.,(4,2,2,2,2,2,2,2,2,2,
2,2,2,2,2,2,2,2,2,2,2,2,2,2,2,2,2,2,2,2,2,2,2,2,2,2,2,2,2,2,2,2,2,2,2,2,
2,2,2,2,2,2,2,2,2,2,2,2,2,2,2,2,2,2,2,2,2,2,2,2,2,2,2,2,2,4),(0.301764389565749,
0.336997421742996,0.402082561451209,0.412049110741382,0.415672773957841,
0.418124329011747,0.420330373038981,0.423359284103103,0.430993232595732,
0.495970310647265,0.541381653988435,0.558002432545585,0.570309617785616,
0.575906333243603,0.580146535002168,0.584167219828148,0.590958727159664,
0.609654629986511,0.612060019638961,0.711477517129167,0.725494253380263,
0.734768867433389,0.738292895505578,0.74072454168496,0.742950473644679,
0.746055936666919,0.754173521210122,0.806227076830489,0.860614627825897,
0.879029039364973,0.892343234318116,0.898117562918137,0.902386070272692,
0.906898503025551,0.913899501389437,0.93413983033226,1.03396779548654,1.04800204454639,
1.05728549503769,1.06081107926912,1.06324322932423,1.06546917102268,1.06857405240924,
1.076685567579,1.12662310049518,1.1739252833292,1.20983528000517,1.21798015619441,
1.22274258104761,1.22694288265329,1.23220288395753,1.24042661088312,1.30176537997898,
1.36934405933428,1.37946192939676,1.3831071305885,1.38556349497273,1.38776634224661,
1.39078128546721,1.39833043639893,1.46471256066369,1.52993648428243,1.53944564985019,
1.54449911708538,1.54864722191747,1.55355257507023,1.56212209826921,1.60169513190205,
1.66746908985183,1.6989644829291,1.70415692239507,1.70695086905996,1.70930465801907,
1.71229179931322,1.71706738939369,1.7301847824281),.UNSPECIFIED.);
#1287=B_SPLINE_CURVE_WITH_KNOTS('',3,(#21412,#21413,#21414,#21415,#21416,
#21417,#21418,#21419,#21420,#21421,#21422,#21423,#21424,#21425,#21426,#21427,
#21428,#21429,#21430,#21431,#21432,#21433,#21434,#21435,#21436,#21437,#21438,
#21439,#21440,#21441,#21442,#21443,#21444,#21445,#21446,#21447,#21448,#21449,
#21450,#21451,#21452,#21453,#21454,#21455,#21456,#21457,#21458,#21459,#21460,
#21461,#21462,#21463,#21464,#21465,#21466,#21467,#21468,#21469,#21470,#21471,
#21472,#21473,#21474,#21475,#21476,#21477,#21478,#21479,#21480,#21481,#21482,
#21483,#21484,#21485,#21486,#21487,#21488,#21489,#21490,#21491,#21492,#21493,
#21494,#21495,#21496,#21497,#21498,#21499,#21500,#21501,#21502,#21503,#21504,
#21505,#21506,#21507,#21508,#21509,#21510,#21511,#21512,#21513,#21514,#21515,
#21516,#21517,#21518,#21519,#21520,#21521,#21522,#21523,#21524,#21525,#21526,
#21527,#21528,#21529,#21530,#21531,#21532,#21533,#21534,#21535,#21536,#21537,
#21538,#21539,#21540,#21541,#21542,#21543,#21544,#21545,#21546,#21547,#21548,
#21549,#21550,#21551,#21552,#21553,#21554,#21555,#21556,#21557,#21558,#21559,
#21560,#21561,#21562,#21563,#21564,#21565),.UNSPECIFIED.,.F.,.F.,(4,2,2,
2,2,2,2,2,2,2,2,2,2,2,2,2,2,2,2,2,2,2,2,2,2,2,2,2,2,2,2,2,2,2,2,2,2,2,2,
2,2,2,2,2,2,2,2,2,2,2,2,2,2,2,2,2,2,2,2,2,2,2,2,2,2,2,2,2,2,2,2,2,2,2,2,
2,4),(2.02429205743456,2.05982563655793,2.06831357651967,2.0732008319214,
2.07739042046877,2.08248414896639,2.09218608974965,2.15473965184139,2.22371438725919,
2.23113277901731,2.23403844746681,2.23643191535898,2.23898220662163,2.24306189954909,
2.25679125124458,2.28118682621688,2.36250058773232,2.38468531338238,2.39192507882908,
2.39648859072482,2.40073421316354,2.40636995271312,2.41889671966936,2.43590192211972,
2.48311572678428,2.54531869209189,2.55308440903767,2.55613485598263,2.55834598806923,
2.56079041955842,2.5643820272343,2.57412690853977,2.63573887958691,2.69810893458408,
2.71066961404753,2.71624977324714,2.72050129125558,2.72504643215298,2.73220446309448,
2.75588971687803,2.7973788235357,2.86304967048591,2.8742322698189,2.87814595134809,
2.88040924477266,2.88281112641316,2.8861783425374,2.89444589921121,2.90646402436641,
2.94382066934414,3.02144595405536,3.03214895875594,3.03752665854793,3.04147629715229,
3.04575827329045,3.05161669654854,3.06543366834844,3.08476732237958,3.14180416032355,
3.16715890002166,3.19403536748223,3.19876638997552,3.20173958629876,3.20409174214718,
3.20689483258659,3.21213375952348,3.24503719982133,3.31698945877872,3.34967688859921,
3.35782181140696,3.36262927634612,3.36682191085842,3.37190739490323,3.38169003524407,
3.3942227840258,3.42336842327489,3.45200167847295),.UNSPECIFIED.);
#1288=B_SPLINE_CURVE_WITH_KNOTS('',3,(#22090,#22091,#22092,#22093,#22094,
#22095,#22096,#22097,#22098,#22099,#22100,#22101,#22102,#22103,#22104,#22105,
#22106,#22107,#22108,#22109,#22110,#22111,#22112,#22113,#22114,#22115,#22116,
#22117,#22118,#22119,#22120,#22121,#22122,#22123,#22124,#22125,#22126,#22127,
#22128,#22129,#22130,#22131,#22132,#22133,#22134,#22135,#22136,#22137,#22138,
#22139,#22140,#22141,#22142,#22143,#22144,#22145,#22146,#22147,#22148,#22149,
#22150,#22151,#22152,#22153,#22154,#22155,#22156,#22157,#22158,#22159,#22160,
#22161,#22162,#22163,#22164,#22165,#22166,#22167,#22168,#22169,#22170,#22171,
#22172,#22173,#22174,#22175,#22176,#22177,#22178,#22179,#22180,#22181,#22182,
#22183),.UNSPECIFIED.,.F.,.F.,(4,3,3,3,3,3,3,3,3,3,3,3,3,3,3,3,3,3,3,3,
3,3,3,3,3,3,3,3,3,3,3,4),(0.,0.0258260740408245,0.0620914164741229,0.0993864137683754,
0.136681411062628,0.147696100525531,0.154010737947389,0.189902258745158,
0.22572273166162,0.260776893843891,0.288525741895271,0.294828798261742,
0.299623899892133,0.334131254550439,0.368141603593604,0.402151952636769,
0.423542327420144,0.431068176013837,0.436300783095514,0.441119373588802,
0.474798699922684,0.508767094152298,0.542465821270648,0.56749016733248,
0.575255905600941,0.608325399901122,0.640746061995403,0.657708562027131,
0.662778546763718,0.694621529164936,0.72559455743344,0.744397949170769),
 .UNSPECIFIED.);
#1289=B_SPLINE_CURVE_WITH_KNOTS('',3,(#23756,#23757,#23758,#23759,#23760,
#23761,#23762,#23763,#23764,#23765,#23766,#23767,#23768,#23769,#23770,#23771,
#23772,#23773,#23774,#23775,#23776,#23777,#23778,#23779,#23780,#23781,#23782,
#23783,#23784,#23785,#23786,#23787,#23788,#23789,#23790,#23791,#23792,#23793,
#23794,#23795,#23796,#23797,#23798,#23799,#23800,#23801,#23802,#23803,#23804,
#23805,#23806,#23807,#23808,#23809,#23810,#23811,#23812,#23813,#23814,#23815,
#23816,#23817,#23818,#23819,#23820,#23821,#23822,#23823,#23824,#23825,#23826,
#23827,#23828,#23829,#23830,#23831,#23832,#23833,#23834,#23835,#23836,#23837,
#23838,#23839,#23840,#23841,#23842,#23843,#23844,#23845,#23846,#23847,#23848,
#23849,#23850,#23851,#23852,#23853,#23854,#23855,#23856,#23857,#23858,#23859,
#23860,#23861,#23862,#23863,#23864,#23865,#23866,#23867,#23868,#23869,#23870,
#23871,#23872,#23873,#23874,#23875,#23876,#23877,#23878,#23879,#23880,#23881,
#23882,#23883,#23884,#23885,#23886,#23887,#23888,#23889,#23890,#23891,#23892,
#23893,#23894,#23895,#23896,#23897,#23898,#23899,#23900,#23901),
 .UNSPECIFIED.,.F.,.F.,(4,2,2,2,2,2,2,2,2,2,2,2,2,2,2,2,2,2,2,2,2,2,2,2,
2,2,2,2,2,2,2,2,2,2,2,2,2,2,2,2,2,2,2,2,2,2,2,2,2,2,2,2,2,2,2,2,2,2,2,2,
2,2,2,2,2,2,2,2,2,2,2,2,4),(0.00561840038966108,0.0829874935783554,0.113427462423338,
0.126395668356017,0.136577031974214,0.1418189926542,0.146080884437416,0.150998255954348,
0.159408985883126,0.195113324983282,0.259907465387342,0.281920212796875,
0.294766066261603,0.29881970124982,0.301371020753402,0.303763134602496,
0.307169565336292,0.315270901268713,0.364708929927512,0.411921772563163,
0.447764628065761,0.45592937153838,0.460710921840607,0.464932961417181,
0.4702269313106,0.478517238233412,0.540306725514118,0.58453028550462,0.605265236649418,
0.617560623264396,0.621484960969627,0.624002963893898,0.62640450493714,
0.629374199664684,0.636710300272061,0.705249954748309,0.748473115816585,
0.772740034761623,0.779926576082181,0.784457139716752,0.788672088869992,
0.794170698250464,0.806399405848167,0.879829039931145,0.920414664077409,
0.933011134198793,0.941564284506154,0.944960511711001,0.947356833621923,
0.94960519711638,0.953439151550553,0.9640459149341,1.03032509859657,1.07205030445187,
1.09583966565259,1.10302064013644,1.10757890181242,1.11184185903787,1.11743609652098,
1.13002667538366,1.19096936970976,1.25326166676231,1.26305870208845,1.26666723466649,
1.2691224866918,1.2713376802449,1.27439436336967,1.28217677566595,1.34418144738385,
1.39148325654162,1.40850471952644,1.42103960946813,1.42238233932181),
 .UNSPECIFIED.);
#1290=B_SPLINE_CURVE_WITH_KNOTS('',3,(#23903,#23904,#23905,#23906),
 .UNSPECIFIED.,.F.,.F.,(4,4),(0.,0.0501024666884938),.UNSPECIFIED.);
#1291=B_SPLINE_CURVE_WITH_KNOTS('',3,(#23907,#23908,#23909,#23910,#23911,
#23912,#23913,#23914,#23915,#23916,#23917,#23918,#23919,#23920,#23921,#23922,
#23923,#23924,#23925,#23926,#23927,#23928,#23929,#23930,#23931,#23932,#23933,
#23934,#23935,#23936,#23937,#23938,#23939,#23940,#23941,#23942,#23943),
 .UNSPECIFIED.,.F.,.F.,(4,3,3,3,3,3,3,3,3,3,3,3,4),(-3.03270570277863,-2.99355252518221,
-2.90575452476498,-2.81806846465193,-2.73046974794672,-2.64293160597546,
-2.55542456519864,-2.46792653698669,-2.3804154444671,-2.29281858352263,
-2.20517529783961,-2.11740034625084,-2.06153490655644),.UNSPECIFIED.);
#1292=B_SPLINE_CURVE_WITH_KNOTS('',3,(#23945,#23946,#23947,#23948,#23949,
#23950,#23951,#23952,#23953,#23954,#23955,#23956,#23957,#23958,#23959,#23960,
#23961,#23962,#23963,#23964,#23965,#23966,#23967,#23968,#23969,#23970,#23971,
#23972,#23973,#23974,#23975,#23976,#23977,#23978,#23979,#23980,#23981,#23982,
#23983,#23984,#23985,#23986,#23987,#23988,#23989,#23990,#23991,#23992,#23993,
#23994,#23995,#23996,#23997,#23998,#23999,#24000,#24001,#24002,#24003,#24004,
#24005,#24006,#24007,#24008,#24009,#24010,#24011,#24012,#24013,#24014,#24015,
#24016,#24017,#24018,#24019,#24020,#24021,#24022,#24023,#24024,#24025,#24026,
#24027,#24028,#24029,#24030,#24031,#24032,#24033,#24034,#24035,#24036,#24037,
#24038,#24039,#24040,#24041,#24042,#24043,#24044,#24045,#24046,#24047,#24048,
#24049,#24050),.UNSPECIFIED.,.F.,.F.,(4,3,3,3,3,3,3,3,3,3,3,3,3,3,3,3,3,
3,3,3,3,3,3,3,3,3,3,3,3,3,3,3,3,3,3,4),(11.6152142277546,11.710478589548,
11.8056881718592,11.9008650919448,11.9960581933183,12.0912656561396,12.186507565826,
12.2818040356968,12.3772412794828,12.4727567243883,12.5684397131032,12.613065069482,
12.7052250926877,12.7972467196939,12.8891587437926,12.9809895468936,13.0727771628103,
13.1645473844809,13.2563259834302,13.3481995729483,13.4401212358669,13.5322010952523,
13.6109159112094,13.7041429367066,13.79724435493,13.8902475827988,13.9831825993322,
14.0760822056078,14.1689710331669,14.2618736980142,14.3548731676223,14.4479236129884,
14.541125320041,14.6087667529368,14.7020045732548,14.7774109291987),
 .UNSPECIFIED.);
#1293=B_SPLINE_CURVE_WITH_KNOTS('',3,(#25106,#25107,#25108,#25109,#25110),
 .UNSPECIFIED.,.F.,.F.,(4,1,4),(13.8752082355906,14.7665104986906,15.0541924217381),
 .UNSPECIFIED.);
#1294=B_SPLINE_CURVE_WITH_KNOTS('',3,(#25113,#25114,#25115,#25116),
 .UNSPECIFIED.,.F.,.F.,(4,4),(14.3991256467175,15.0523450926205),
 .UNSPECIFIED.);
#1295=B_SPLINE_CURVE_WITH_KNOTS('',3,(#25122,#25123,#25124,#25125,#25126,
#25127,#25128,#25129,#25130,#25131),.UNSPECIFIED.,.F.,.F.,(4,1,1,1,1,1,
1,4),(15.707963267949,15.7361680573154,16.7058256159401,17.6754831745648,
18.6451407331896,19.6147982918143,20.584455850439,21.3359364871903),
 .UNSPECIFIED.);
#1296=B_SPLINE_CURVE_WITH_KNOTS('',3,(#25132,#25133,#25134,#25135),
 .UNSPECIFIED.,.F.,.F.,(4,4),(15.0541924217381,15.707963267949),
 .UNSPECIFIED.);
#1297=B_SPLINE_CURVE_WITH_KNOTS('',3,(#25137,#25138,#25139,#25140,#25141),
 .UNSPECIFIED.,.F.,.F.,(4,1,4),(15.0523450926205,15.3687832053423,15.7079559920353),
 .UNSPECIFIED.);
#1298=B_SPLINE_CURVE_WITH_KNOTS('',3,(#25142,#25143,#25144,#25145,#25146,
#25147,#25148,#25149,#25150,#25151,#25152,#25153,#25154,#25155,#25156,#25157,
#25158,#25159,#25160,#25161,#25162,#25163,#25164,#25165,#25166,#25167,#25168,
#25169,#25170,#25171,#25172,#25173,#25174,#25175,#25176,#25177,#25178,#25179,
#25180,#25181,#25182,#25183,#25184,#25185,#25186,#25187,#25188,#25189,#25190,
#25191,#25192,#25193,#25194,#25195,#25196,#25197,#25198,#25199,#25200,#25201,
#25202,#25203,#25204,#25205,#25206,#25207,#25208,#25209,#25210,#25211,#25212,
#25213,#25214,#25215,#25216,#25217,#25218,#25219,#25220,#25221,#25222,#25223,
#25224,#25225,#25226,#25227,#25228,#25229,#25230,#25231,#25232,#25233,#25234,
#25235,#25236,#25237,#25238,#25239,#25240,#25241,#25242,#25243,#25244,#25245,
#25246,#25247,#25248,#25249,#25250,#25251,#25252,#25253,#25254,#25255,#25256,
#25257,#25258,#25259,#25260,#25261,#25262,#25263,#25264,#25265,#25266,#25267,
#25268,#25269,#25270,#25271,#25272,#25273,#25274,#25275,#25276,#25277,#25278,
#25279,#25280,#25281,#25282,#25283,#25284,#25285,#25286,#25287,#25288,#25289,
#25290,#25291,#25292,#25293,#25294,#25295,#25296,#25297,#25298,#25299,#25300,
#25301,#25302,#25303,#25304,#25305,#25306,#25307,#25308,#25309,#25310,#25311,
#25312,#25313,#25314,#25315,#25316,#25317,#25318,#25319,#25320,#25321,#25322,
#25323,#25324,#25325,#25326,#25327,#25328,#25329,#25330,#25331,#25332,#25333,
#25334,#25335,#25336,#25337),.UNSPECIFIED.,.F.,.F.,(4,3,3,3,3,3,3,3,3,3,
3,3,3,3,3,3,3,3,3,3,3,3,3,3,3,3,3,3,3,3,3,3,3,3,3,3,3,3,3,3,3,3,3,3,3,3,
3,3,3,3,3,3,3,3,3,3,3,3,3,3,3,3,3,3,3,4),(15.707963267949,15.7953191781018,
15.882666103131,15.9700247548158,16.0574158483864,16.1449087968635,16.2324629526336,
16.3201451818259,16.338440763967,16.4265915804881,16.5146360954676,16.6025968319756,
16.6907845183026,16.7786538304492,16.8665116399313,16.9543781872225,17.0428082210648,
17.1307958621293,17.2194470923605,17.3080983225917,17.39627025819,17.4843382017312,
17.5723246356153,17.6605035413154,17.7484039692419,17.8362948905087,17.9241965166447,
18.0125863577876,18.1006136302211,18.1891847557188,18.2777558812165,18.3657091708626,
18.4535548185024,18.5413156253886,18.6295778521952,18.7172460090986,18.804902588628,
18.8925680768335,18.9812794175854,19.0690682889294,19.1582408643853,19.2474134398412,
19.335483835568,19.4234480064783,19.5113285891001,19.5995463902709,19.6873365944086,
19.7751158504035,19.8629045010682,19.9514461254176,20.0393582345022,20.128214616484,
20.2170709984659,20.3051302458619,20.3930833744788,20.480953035497,20.5691749756962,
20.656954632174,20.7447235025596,20.832501943196,20.9210585966697,21.0089610261075,
21.0978447915991,21.1867285570907,21.2735006371787,21.3371564183306),
 .UNSPECIFIED.);
#1299=B_SPLINE_CURVE_WITH_KNOTS('',3,(#25343,#25344,#25345,#25346,#25347,
#25348,#25349,#25350,#25351,#25352,#25353,#25354,#25355,#25356,#25357,#25358,
#25359,#25360,#25361,#25362,#25363,#25364,#25365,#25366,#25367,#25368,#25369,
#25370,#25371,#25372,#25373,#25374,#25375,#25376,#25377,#25378,#25379,#25380,
#25381,#25382,#25383,#25384,#25385,#25386,#25387,#25388,#25389,#25390,#25391,
#25392,#25393,#25394,#25395,#25396,#25397,#25398,#25399,#25400,#25401,#25402,
#25403,#25404,#25405,#25406,#25407,#25408,#25409,#25410,#25411,#25412,#25413,
#25414,#25415,#25416,#25417,#25418,#25419,#25420,#25421,#25422,#25423,#25424,
#25425,#25426,#25427,#25428,#25429,#25430,#25431,#25432,#25433,#25434,#25435,
#25436,#25437,#25438,#25439,#25440,#25441,#25442,#25443,#25444,#25445,#25446,
#25447,#25448,#25449,#25450,#25451,#25452,#25453,#25454,#25455,#25456,#25457,
#25458,#25459,#25460,#25461,#25462,#25463,#25464,#25465,#25466,#25467,#25468,
#25469,#25470,#25471,#25472,#25473,#25474,#25475,#25476,#25477,#25478,#25479,
#25480,#25481,#25482,#25483,#25484,#25485,#25486,#25487,#25488,#25489,#25490,
#25491,#25492,#25493,#25494,#25495,#25496,#25497,#25498,#25499,#25500,#25501,
#25502,#25503,#25504,#25505,#25506,#25507,#25508,#25509,#25510,#25511,#25512,
#25513,#25514,#25515,#25516,#25517,#25518,#25519,#25520,#25521,#25522,#25523,
#25524,#25525,#25526,#25527,#25528,#25529,#25530,#25531,#25532,#25533,#25534,
#25535),.UNSPECIFIED.,.F.,.F.,(4,3,3,3,3,3,3,3,3,3,3,3,3,3,3,3,3,3,3,3,
3,3,3,3,3,3,3,3,3,3,3,3,3,3,3,3,3,3,3,3,3,3,3,3,3,3,3,3,3,3,3,3,3,3,3,3,
3,3,3,3,3,3,3,3,4),(21.9911485751286,22.0812818533853,22.1714775654381,
22.2618222124728,22.3522429655899,22.4428404146287,22.5237709676885,22.6118195054854,
22.6997616830464,22.7876201674516,22.8758462123093,22.9636142132378,23.0513712689732,
23.1391377493465,23.2277104435881,23.3156006621682,23.4045145942407,23.4934285263132,
23.5814764104089,23.6694179282831,23.7572757479402,23.8455020400649,23.9332693683819,
24.0210257498194,24.1087915550198,24.1973651874993,24.285254734994,24.3741704099659,
24.4630860849379,24.5511339011155,24.6390753469046,24.7269330904281,24.8151594095699,
24.902926652306,24.9906829447511,25.0784486576395,25.1670224041203,25.2549118519318,
25.3438277477472,25.4327436435627,25.5207914393718,25.608732868773,25.6965905998733,
25.7848169251625,25.8725841652395,25.9603404587052,26.0481061762938,26.1366799327672,
26.2245693942772,26.3134852982323,26.4024012021874,26.4904491024023,26.5783906332456,
26.6662484627345,26.7544747499942,26.8422420804156,26.9299984610454,27.0177642625259,
27.1063378870974,27.1942274237512,27.2831430922816,27.3720587608121,27.459280535532,
27.5463867365523,27.6203176265813),.UNSPECIFIED.);
#1300=B_SPLINE_CURVE_WITH_KNOTS('',3,(#25536,#25537,#25538,#25539,#25540),
 .UNSPECIFIED.,.F.,.F.,(4,1,4),(21.3359364871903,21.5541134090638,21.9911454985159),
 .UNSPECIFIED.);
#1301=B_SPLINE_CURVE_WITH_KNOTS('',3,(#25542,#25543,#25544,#25545,#25546,
#25547,#25548,#25549,#25550,#25551,#25552,#25553,#25554,#25555,#25556,#25557,
#25558,#25559,#25560,#25561,#25562,#25563,#25564,#25565,#25566),
 .UNSPECIFIED.,.F.,.F.,(4,3,3,3,3,3,3,3,4),(21.3371564183306,21.4237674913069,
21.5103226356218,21.59684350434,21.6833517173297,21.7699037254338,21.8564793827075,
21.9431463484601,21.9911485750058),.UNSPECIFIED.);
#1302=B_SPLINE_CURVE_WITH_KNOTS('',3,(#25567,#25568,#25569,#25570,#25571,
#25572,#25573,#25574,#25575,#25576,#25577,#25578,#25579,#25580,#25581,#25582,
#25583,#25584,#25585,#25586,#25587,#25588,#25589,#25590,#25591,#25592,#25593,
#25594,#25595,#25596,#25597,#25598,#25599,#25600,#25601,#25602,#25603,#25604,
#25605,#25606,#25607,#25608,#25609,#25610,#25611,#25612,#25613,#25614,#25615,
#25616,#25617,#25618,#25619,#25620,#25621,#25622,#25623,#25624,#25625,#25626,
#25627,#25628,#25629,#25630,#25631,#25632,#25633,#25634,#25635,#25636,#25637,
#25638,#25639,#25640,#25641,#25642,#25643,#25644,#25645,#25646,#25647,#25648,
#25649,#25650,#25651,#25652,#25653,#25654,#25655,#25656,#25657,#25658,#25659,
#25660,#25661,#25662,#25663,#25664,#25665,#25666,#25667,#25668,#25669,#25670,
#25671,#25672,#25673,#25674,#25675,#25676,#25677,#25678,#25679,#25680,#25681,
#25682,#25683,#25684,#25685,#25686,#25687,#25688,#25689,#25690,#25691,#25692,
#25693,#25694,#25695,#25696,#25697,#25698,#25699,#25700,#25701,#25702,#25703,
#25704,#25705,#25706,#25707,#25708,#25709,#25710,#25711,#25712,#25713,#25714,
#25715,#25716,#25717,#25718,#25719,#25720,#25721,#25722,#25723,#25724,#25725,
#25726,#25727,#25728,#25729,#25730,#25731,#25732,#25733,#25734,#25735,#25736,
#25737,#25738,#25739,#25740,#25741,#25742,#25743,#25744,#25745,#25746,#25747,
#25748,#25749,#25750,#25751,#25752,#25753,#25754,#25755,#25756,#25757,#25758,
#25759),.UNSPECIFIED.,.F.,.F.,(4,3,3,3,3,3,3,3,3,3,3,3,3,3,3,3,3,3,3,3,
3,3,3,3,3,3,3,3,3,3,3,3,3,3,3,3,3,3,3,3,3,3,3,3,3,3,3,3,3,3,3,3,3,3,3,3,
3,3,3,3,3,3,3,3,4),(21.9911485751286,22.1228194350913,22.1563861157154,
22.2444380999692,22.3323837550216,22.4202457430996,22.5084704845047,22.59624202941,
22.6840026375976,22.7717726746395,22.8603404245647,22.948234177373,23.0371389258566,
23.1260436743401,23.214092344832,23.3020346710917,23.3898933199334,23.4781193090624,
23.5658875121345,23.6536447839157,23.7414114940515,23.8299839287799,23.9178744090476,
24.0067878210062,24.0957012329649,24.1837476390331,24.2716876540278,24.3595439480956,
24.4477708035323,24.5355365607886,24.623291356946,24.7110555644892,24.7996313712643,
24.887519305156,24.9764390483728,25.0653587915896,25.1534073144324,25.241349476856,
25.3292079459619,25.4174339964934,25.5052019818284,25.5929590218885,25.6807254865233,
25.7692982024461,25.8571884052756,25.946102377745,26.0350163502143,26.1230642365196,
26.2110057565983,26.2988635784517,26.3870898697501,26.4748572002282,26.5626135838093,
26.650379391133,26.7389530205595,26.826842570107,26.9157582394731,27.0046739088391,
27.0927089175608,27.1806439750418,27.2684996153284,27.3562982655407,27.4440610465582,
27.531833492624,27.6195744277319),.UNSPECIFIED.);
#1303=B_SPLINE_CURVE_WITH_KNOTS('',3,(#25765,#25766,#25767,#25768,#25769,
#25770,#25771,#25772,#25773,#25774),.UNSPECIFIED.,.F.,.F.,(4,1,1,1,1,1,
1,4),(28.2743338823081,28.3417163194369,29.3113738780616,30.2810314366863,
31.2506889953111,32.2203465539358,33.1900041125605,33.9023219446702),
 .UNSPECIFIED.);
#1304=B_SPLINE_CURVE_WITH_KNOTS('',3,(#25775,#25776,#25777,#25778,#25779,
#25780,#25781,#25782,#25783,#25784,#25785,#25786,#25787,#25788,#25789,#25790,
#25791,#25792,#25793,#25794,#25795,#25796,#25797,#25798,#25799),
 .UNSPECIFIED.,.F.,.F.,(4,3,3,3,3,3,3,3,4),(27.6203176265813,27.7073051292124,
27.794260804199,27.8812059046581,27.9681616709394,28.055194626814,28.1422707001016,
28.2294648389027,28.2743338823081),.UNSPECIFIED.);
#1305=B_SPLINE_CURVE_WITH_KNOTS('',3,(#25801,#25802,#25803,#25804,#25805,
#25806,#25807,#25808,#25809,#25810,#25811,#25812,#25813,#25814,#25815,#25816,
#25817,#25818,#25819,#25820,#25821,#25822),.UNSPECIFIED.,.F.,.F.,(4,3,3,
3,3,3,3,4),(27.6195744277319,27.7082636876649,27.7961529417002,27.885242204582,
27.9743314674638,28.0790230082866,28.1827301957677,28.2743337273969),
 .UNSPECIFIED.);
#1306=B_SPLINE_CURVE_WITH_KNOTS('',3,(#25823,#25824,#25825,#25826,#25827,
#25828,#25829,#25830,#25831,#25832),.UNSPECIFIED.,.F.,.F.,(4,1,1,1,1,1,
1,4),(28.2743338823081,28.9439890260885,29.9136465847132,30.883304143338,
31.8529617019627,32.8226192605874,33.7922768192122,33.9036448620551),
 .UNSPECIFIED.);
#1307=B_SPLINE_CURVE_WITH_KNOTS('',3,(#25838,#25839,#25840,#25841,#25842,
#25843,#25844,#25845,#25846,#25847,#25848,#25849,#25850),.UNSPECIFIED.,
 .F.,.F.,(4,3,3,3,4),(7.592022928411,7.72998057268366,7.75726046899785,
7.85218978178926,7.94711909458068),.UNSPECIFIED.);
#1308=B_SPLINE_CURVE_WITH_KNOTS('',3,(#25852,#25853,#25854,#25855,#25856,
#25857,#25858,#25859,#25860,#25861,#25862,#25863,#25864,#25865,#25866,#25867,
#25868,#25869,#25870,#25871,#25872,#25873,#25874,#25875,#25876,#25877,#25878,
#25879,#25880,#25881,#25882,#25883,#25884,#25885,#25886,#25887,#25888,#25889,
#25890,#25891,#25892,#25893,#25894,#25895,#25896,#25897,#25898,#25899,#25900,
#25901,#25902,#25903,#25904,#25905,#25906,#25907,#25908,#25909,#25910,#25911,
#25912,#25913,#25914,#25915,#25916,#25917,#25918,#25919,#25920,#25921,#25922,
#25923,#25924,#25925,#25926,#25927,#25928,#25929,#25930,#25931,#25932,#25933,
#25934,#25935,#25936,#25937,#25938,#25939,#25940,#25941,#25942,#25943,#25944,
#25945,#25946,#25947,#25948,#25949,#25950,#25951,#25952,#25953,#25954,#25955,
#25956,#25957,#25958,#25959,#25960,#25961,#25962,#25963,#25964,#25965,#25966,
#25967,#25968,#25969,#25970,#25971,#25972,#25973,#25974,#25975,#25976,#25977,
#25978,#25979,#25980,#25981,#25982,#25983,#25984,#25985,#25986,#25987,#25988,
#25989,#25990,#25991,#25992,#25993,#25994,#25995,#25996,#25997,#25998,#25999,
#26000,#26001,#26002,#26003,#26004,#26005,#26006,#26007,#26008,#26009,#26010,
#26011,#26012,#26013,#26014,#26015,#26016,#26017,#26018,#26019,#26020,#26021,
#26022,#26023,#26024,#26025,#26026,#26027,#26028,#26029,#26030,#26031,#26032,
#26033,#26034,#26035,#26036,#26037,#26038,#26039,#26040,#26041),
 .UNSPECIFIED.,.F.,.F.,(4,3,3,3,3,3,3,3,3,3,3,3,3,3,3,3,3,3,3,3,3,3,3,3,
3,3,3,3,3,3,3,3,3,3,3,3,3,3,3,3,3,3,3,3,3,3,3,3,3,3,3,3,3,3,3,3,3,3,3,3,
3,3,3,4),(2.0176935435318,2.10900613700961,2.20020948780471,2.29132757712989,
2.38239979845583,2.47345065763357,2.56450463665772,2.65563952109678,2.7468159737042,
2.83813121660439,2.90897267587419,3.00135448708213,3.09362272558863,3.18580324790417,
3.27792608126715,3.3700199280202,3.46210804549375,3.55421368001692,3.6464128429923,
3.73866410476864,3.8310522924152,3.87863023449892,3.97078296023955,4.06281811462994,
4.15476192079865,4.24664363672281,4.33849375932083,4.43033586316209,4.52219351001169,
4.61414316369226,4.70614373799067,4.79828172793459,4.84828779312365,4.94056321631626,
5.03272261966758,5.12479203689778,5.21680086059312,5.308778956382,5.40074973362021,
5.49273658940472,5.58481549634695,5.67694551413242,5.76921203980279,5.81794535174838,
5.91020909431947,6.00235693384428,6.09441492089814,6.18641256521841,6.27837964339645,
6.37033958024058,6.46231578844065,6.55438440757534,6.64650432910375,6.73876115358093,
6.78760291037311,6.8785392358345,6.96933903752258,7.06006166276081,7.1507320536416,
7.24137509809403,7.33205488312372,7.42275060426606,7.51354992827336,7.5920229281199),
 .UNSPECIFIED.);
#1309=B_SPLINE_CURVE_WITH_KNOTS('',3,(#26044,#26045,#26046,#26047,#26048,
#26049,#26050,#26051,#26052,#26053,#26054,#26055,#26056,#26057,#26058,#26059,
#26060,#26061,#26062,#26063,#26064,#26065,#26066,#26067,#26068,#26069,#26070,
#26071,#26072,#26073,#26074,#26075,#26076,#26077,#26078,#26079,#26080,#26081,
#26082,#26083,#26084,#26085,#26086,#26087,#26088,#26089,#26090,#26091,#26092,
#26093,#26094,#26095,#26096,#26097,#26098,#26099,#26100,#26101,#26102,#26103,
#26104,#26105,#26106,#26107,#26108,#26109,#26110,#26111,#26112,#26113,#26114,
#26115,#26116,#26117,#26118,#26119,#26120,#26121,#26122,#26123,#26124,#26125,
#26126,#26127,#26128,#26129,#26130,#26131),.UNSPECIFIED.,.F.,.F.,(4,2,2,
2,2,2,2,2,2,2,2,2,2,2,2,2,2,2,2,2,2,2,2,2,2,2,2,2,2,2,2,2,2,2,2,2,2,2,2,
2,2,2,2,4),(0.000213322277777609,0.0081712364937981,0.0180651814832395,
0.0898839906907267,0.131793832432466,0.155491307257063,0.181103288449151,
0.27540615577459,0.312356721458623,0.326548888301831,0.33877329588411,0.36164707735747,
0.421445917416244,0.453614416798198,0.48020288102199,0.50005478394176,0.523917830127524,
0.60111797580595,0.630853315953084,0.651562322220697,0.663443723530535,
0.678063909123624,0.717907332690356,0.771430698552995,0.807243642528013,
0.829055144438564,0.852189025253953,0.904418311791255,0.964484903374977,
0.982393494675465,0.994646271915792,1.01304652705384,1.08900583967967,1.13006385373997,
1.15222227131495,1.17427647889075,1.21412238852217,1.27425770059287,1.29572128492808,
1.31261454987213,1.32461516809104,1.34294772153475,1.41903836990406,1.42895520339045),
 .UNSPECIFIED.);
#1310=B_SPLINE_CURVE_WITH_KNOTS('',3,(#26137,#26138,#26139,#26140,#26141,
#26142,#26143,#26144,#26145,#26146,#26147,#26148,#26149),.UNSPECIFIED.,
 .F.,.F.,(4,3,3,3,4),(13.8752082355906,13.9667885610938,14.0583377787896,
14.1499114854528,14.2294808573324),.UNSPECIFIED.);
#1311=B_SPLINE_CURVE_WITH_KNOTS('',3,(#26150,#26151,#26152,#26153,#26154,
#26155,#26156,#26157,#26158,#26159,#26160,#26161,#26162,#26163,#26164,#26165,
#26166,#26167,#26168,#26169,#26170,#26171,#26172,#26173,#26174,#26175,#26176,
#26177,#26178,#26179,#26180,#26181,#26182,#26183,#26184,#26185,#26186,#26187,
#26188,#26189,#26190,#26191,#26192,#26193,#26194,#26195,#26196,#26197,#26198,
#26199,#26200,#26201,#26202,#26203,#26204,#26205,#26206,#26207,#26208,#26209,
#26210,#26211,#26212,#26213,#26214,#26215,#26216,#26217,#26218,#26219,#26220,
#26221,#26222,#26223,#26224,#26225,#26226,#26227,#26228,#26229,#26230,#26231,
#26232,#26233,#26234,#26235,#26236,#26237,#26238,#26239,#26240,#26241,#26242,
#26243,#26244,#26245,#26246,#26247,#26248,#26249,#26250,#26251,#26252,#26253,
#26254,#26255,#26256,#26257,#26258,#26259,#26260,#26261,#26262,#26263,#26264,
#26265,#26266,#26267,#26268,#26269,#26270,#26271,#26272,#26273,#26274,#26275,
#26276,#26277,#26278,#26279,#26280,#26281,#26282,#26283,#26284,#26285,#26286,
#26287,#26288,#26289,#26290,#26291,#26292,#26293,#26294,#26295,#26296,#26297,
#26298,#26299,#26300,#26301,#26302,#26303,#26304,#26305,#26306,#26307,#26308,
#26309,#26310,#26311,#26312,#26313,#26314,#26315,#26316,#26317,#26318,#26319,
#26320,#26321,#26322,#26323,#26324,#26325,#26326,#26327,#26328,#26329,#26330,
#26331,#26332,#26333,#26334,#26335,#26336,#26337,#26338,#26339,#26340,#26341,
#26342,#26343,#26344,#26345,#26346,#26347,#26348,#26349,#26350,#26351),
 .UNSPECIFIED.,.F.,.F.,(4,3,3,3,3,3,3,3,3,3,3,3,3,3,3,3,3,3,3,3,3,3,3,3,
3,3,3,3,3,3,3,3,3,3,3,3,3,3,3,3,3,3,3,3,3,3,3,3,3,3,3,3,3,3,3,3,3,3,3,3,
3,3,3,3,3,3,3,4),(7.94711909458068,8.03916449689059,8.13115131314578,8.22310877742044,
8.31506032401175,8.40702937604215,8.49909140929719,8.59120587840926,8.68345569404661,
8.72691802762258,8.8191706882828,8.9113071987979,9.00335362771794,9.09533942116433,
9.18729447283689,9.2792422229474,9.37120609946293,9.46326223939332,9.55536958219376,
9.6476137888841,9.69657558624731,9.78882587436606,9.8809599610036,9.97300391854113,
10.0649871802198,10.1569396639359,10.2488848131877,10.3408460592029,10.4328995391064,
10.5250042017507,10.6172457216456,10.666233144872,10.7584856508334,10.8506219888867,
10.9426682279119,11.0346538061488,11.1266086269975,11.2185561309138,11.3105197460972,
11.402575603076,11.4946826502856,11.5869265442726,11.6358907034968,11.7281425425284,
11.8202782073,11.9123237677263,12.0043086623816,12.0962627969125,12.1882096126845,
12.2801725388051,12.3722277094847,12.4643340711003,12.5565772870035,12.6055482621215,
12.6978000285144,12.7899356161397,12.8819810950496,12.9739659020025,13.0659199450359,
13.1578666656258,13.2498294929868,13.3418845600313,13.4339908151117,13.5262339209227,
13.5752058207462,13.6848959854304,13.7935319587344,13.8752082353429),
 .UNSPECIFIED.);
#1312=B_SPLINE_CURVE_WITH_KNOTS('',3,(#26352,#26353,#26354,#26355,#26356,
#26357,#26358,#26359,#26360,#26361,#26362,#26363,#26364,#26365,#26366,#26367,
#26368,#26369,#26370,#26371,#26372,#26373,#26374,#26375,#26376,#26377,#26378,
#26379,#26380,#26381,#26382,#26383,#26384,#26385,#26386,#26387,#26388,#26389,
#26390,#26391,#26392,#26393,#26394,#26395,#26396,#26397,#26398,#26399,#26400,
#26401,#26402,#26403,#26404,#26405,#26406,#26407,#26408,#26409,#26410,#26411,
#26412,#26413,#26414,#26415,#26416,#26417,#26418,#26419,#26420,#26421,#26422,
#26423,#26424,#26425,#26426,#26427,#26428,#26429,#26430,#26431,#26432,#26433,
#26434,#26435,#26436,#26437,#26438,#26439,#26440,#26441,#26442,#26443,#26444,
#26445,#26446,#26447,#26448,#26449,#26450,#26451,#26452,#26453,#26454,#26455,
#26456,#26457,#26458,#26459,#26460,#26461,#26462,#26463,#26464,#26465,#26466,
#26467,#26468,#26469,#26470,#26471,#26472,#26473,#26474,#26475,#26476,#26477,
#26478,#26479),.UNSPECIFIED.,.F.,.F.,(4,2,2,2,2,2,2,2,2,2,2,2,2,2,2,2,2,
2,2,2,2,2,2,2,2,2,2,2,2,2,2,2,2,2,2,2,2,2,2,2,2,2,2,2,2,2,2,2,2,2,2,2,2,
2,2,2,2,2,2,2,2,2,2,4),(1.42895520339045,1.46007496358097,1.48208211995382,
1.50383525497819,1.54229239714939,1.61367123091507,1.63723341041766,1.64972479841955,
1.66413554710266,1.70913175895384,1.75932713685332,1.7938919452629,1.81535639125292,
1.83827099184157,1.92496622075754,1.96180891024268,1.97578576406935,1.98865268163704,
2.01479493650323,2.09654907503768,2.12672628323235,2.14771017773909,2.17188820208918,
2.24835130633677,2.27743430706929,2.29799339774998,2.3101772215098,2.32575431093369,
2.40561867459191,2.448146251685,2.4703723153293,2.49216294186807,2.53023103464384,
2.60191563565894,2.62554538117764,2.63808055811796,2.65254485963469,2.69164913274144,
2.75066083212034,2.78343334713444,2.80467240406175,2.82794644366014,2.90446187422405,
2.93517090993916,2.95642742460775,2.96869014449942,2.98398316625685,3.04122032585058,
3.08279506652258,3.11408919989558,3.13517077037761,3.15889354399749,3.23899869863535,
3.26679837079315,3.28678320333307,3.29891650195166,3.31451643957388,3.3588094988828,
3.40732399911904,3.44127988580007,3.4626370436004,3.4855939743301,3.53754491533665,
3.56373237072242),.UNSPECIFIED.);
#1313=B_SPLINE_CURVE_WITH_KNOTS('',3,(#26485,#26486,#26487,#26488,#26489,
#26490,#26491,#26492,#26493,#26494,#26495,#26496,#26497),.UNSPECIFIED.,
 .F.,.F.,(4,3,3,3,4),(20.1583935427702,20.2835108838085,20.3628087311194,
20.4550618538465,20.5134609524394),.UNSPECIFIED.);
#1314=B_SPLINE_CURVE_WITH_KNOTS('',3,(#26498,#26499,#26500,#26501,#26502,
#26503,#26504,#26505,#26506,#26507,#26508,#26509,#26510,#26511,#26512,#26513,
#26514,#26515,#26516,#26517,#26518,#26519,#26520,#26521,#26522,#26523,#26524,
#26525,#26526,#26527,#26528,#26529,#26530,#26531,#26532,#26533,#26534,#26535,
#26536,#26537,#26538,#26539,#26540,#26541,#26542,#26543,#26544,#26545,#26546,
#26547,#26548,#26549,#26550,#26551,#26552,#26553,#26554,#26555,#26556,#26557,
#26558,#26559,#26560,#26561,#26562,#26563,#26564,#26565,#26566,#26567,#26568,
#26569,#26570,#26571,#26572,#26573,#26574,#26575,#26576,#26577,#26578,#26579,
#26580,#26581,#26582,#26583,#26584,#26585,#26586,#26587,#26588,#26589,#26590,
#26591,#26592,#26593,#26594,#26595,#26596,#26597,#26598,#26599,#26600,#26601,
#26602,#26603,#26604,#26605,#26606,#26607,#26608,#26609,#26610,#26611,#26612,
#26613,#26614,#26615,#26616,#26617,#26618,#26619,#26620,#26621,#26622,#26623,
#26624,#26625,#26626,#26627,#26628,#26629,#26630,#26631,#26632,#26633,#26634,
#26635,#26636,#26637,#26638,#26639,#26640,#26641,#26642,#26643,#26644,#26645,
#26646,#26647,#26648,#26649,#26650,#26651,#26652,#26653,#26654,#26655,#26656,
#26657,#26658,#26659,#26660,#26661,#26662,#26663,#26664,#26665,#26666,#26667,
#26668,#26669,#26670,#26671,#26672,#26673,#26674,#26675,#26676,#26677,#26678,
#26679,#26680,#26681,#26682,#26683,#26684,#26685,#26686,#26687,#26688,#26689,
#26690,#26691,#26692,#26693,#26694,#26695,#26696,#26697,#26698,#26699,#26700,
#26701,#26702),.UNSPECIFIED.,.F.,.F.,(4,3,3,3,3,3,3,3,3,3,3,3,3,3,3,3,3,
3,3,3,3,3,3,3,3,3,3,3,3,3,3,3,3,3,3,3,3,3,3,3,3,3,3,3,3,3,3,3,3,3,3,3,3,
3,3,3,3,3,3,3,3,3,3,3,3,3,3,3,4),(14.2294808573324,14.3211458580209,14.4128655316526,
14.5047229612972,14.544863379371,14.6371152350521,14.7292509130644,14.8212964833362,
14.9132813827541,15.0052355188961,15.0971823331305,15.1891452545648,15.2812004158074,
15.3733067652785,15.4655499649325,15.5145209379957,15.6067734688626,15.6989098267224,
15.790956080476,15.882941665837,15.9748964890955,16.0668439907115,16.1588075988842,
16.2508634417462,16.3429704707886,16.4352143404685,16.4841784966204,16.5764286618195,
16.6685626507028,16.7606065355495,16.8525897620659,16.9445422338854,17.0364873944877,
17.1284486751,17.2205022246723,17.3126069769739,17.4048486168314,17.4538360552452,
17.5460888997187,17.6382255564142,17.7302720940337,17.8222579400587,17.9142130095176,
18.0061607426501,18.0981245674236,18.1901806031659,18.282287811887,18.3745318391812,
18.4234936138699,18.515749813376,18.6078898654283,18.6999398333559,18.7919291466729,
18.8838877045188,18.9758389424325,19.0678062836941,19.1598658322997,19.2519765562282,
19.3442240693714,19.3931511724946,19.4888064687512,19.579682221144,19.6704808514327,
19.761227231578,19.8519461796405,19.9426928355591,20.0334557138223,20.1242985696788,
20.1583935425473),.UNSPECIFIED.);
#1315=B_SPLINE_CURVE_WITH_KNOTS('',3,(#26703,#26704,#26705,#26706,#26707,
#26708,#26709,#26710,#26711,#26712,#26713,#26714,#26715,#26716,#26717,#26718,
#26719,#26720,#26721,#26722,#26723,#26724,#26725,#26726,#26727,#26728,#26729,
#26730,#26731,#26732,#26733,#26734,#26735,#26736,#26737,#26738,#26739,#26740,
#26741,#26742,#26743,#26744,#26745,#26746,#26747,#26748,#26749,#26750,#26751,
#26752,#26753,#26754,#26755,#26756,#26757,#26758,#26759,#26760,#26761,#26762,
#26763,#26764,#26765,#26766,#26767,#26768,#26769,#26770,#26771,#26772,#26773,
#26774,#26775,#26776,#26777,#26778,#26779,#26780,#26781,#26782,#26783,#26784,
#26785,#26786,#26787,#26788,#26789,#26790,#26791,#26792,#26793,#26794,#26795,
#26796,#26797,#26798,#26799,#26800,#26801,#26802,#26803,#26804,#26805,#26806,
#26807,#26808,#26809,#26810,#26811,#26812,#26813,#26814,#26815,#26816,#26817,
#26818,#26819,#26820,#26821,#26822,#26823,#26824,#26825,#26826,#26827,#26828,
#26829,#26830,#26831,#26832,#26833,#26834),.UNSPECIFIED.,.F.,.F.,(4,2,2,
2,2,2,2,2,2,2,2,2,2,2,2,2,2,2,2,2,2,2,2,2,2,2,2,2,2,2,2,2,2,2,2,2,2,2,2,
2,2,2,2,2,2,2,2,2,2,2,2,2,2,2,2,2,2,2,2,2,2,2,2,2,2,4),(3.56373237072242,
3.58500893758219,3.61205525450633,3.62502163344836,3.63875725526822,3.66736872694212,
3.72979858715719,3.75742179782564,3.78196586164726,3.80287856553384,3.83225892708286,
3.90236218915142,3.93857485611522,3.95248185392889,3.96373358626966,3.98677654560246,
4.05658521376898,4.09642272798821,4.11840293043193,4.14044784784961,4.18093262120689,
4.23986264155682,4.26974413711665,4.28304819816273,4.29639233501895,4.32663110267408,
4.38726137784765,4.42625069116603,4.44814569393084,4.47028287207744,4.51172757481414,
4.58971329466417,4.60689960761048,4.61892315991081,4.63704975968857,4.70023433345295,
4.75121650123014,4.77412816144496,4.79551264190333,4.82969079281924,4.87882904963454,
4.92211336059089,4.93775152690358,4.94988200866164,4.96980755625938,4.99747302872111,
5.08099981152042,5.10383064968515,5.12525530834568,5.15980585491857,5.21002914245259,
5.25492534924277,5.2693475545555,5.28191143053491,5.30572909525281,5.37862579493191,
5.4157033627135,5.43740185377705,5.45979205044023,5.50404447853088,5.56445557350166,
5.58926589947181,5.60205980227513,5.61605368880105,5.65343827770255,5.69838345838743),
 .UNSPECIFIED.);
#1316=B_SPLINE_CURVE_WITH_KNOTS('',3,(#26840,#26841,#26842,#26843,#26844,
#26845,#26846,#26847,#26848,#26849,#26850,#26851),.UNSPECIFIED.,.F.,.F.,
(4,2,2,2,2,4),(-0.241179247961179,-0.205768877166292,-0.169865978853117,
-0.146695594041589,-0.120665889329961,-0.120342605042655),.UNSPECIFIED.);
#1317=B_SPLINE_CURVE_WITH_KNOTS('',3,(#26852,#26853,#26854,#26855,#26856,
#26857,#26858,#26859,#26860,#26861,#26862,#26863,#26864,#26865,#26866,#26867,
#26868,#26869,#26870,#26871,#26872,#26873,#26874,#26875,#26876,#26877,#26878,
#26879,#26880,#26881,#26882,#26883,#26884,#26885,#26886,#26887,#26888,#26889,
#26890,#26891,#26892,#26893,#26894,#26895,#26896,#26897,#26898,#26899,#26900,
#26901,#26902,#26903,#26904,#26905,#26906,#26907,#26908,#26909,#26910,#26911,
#26912,#26913,#26914,#26915,#26916,#26917,#26918,#26919,#26920,#26921,#26922,
#26923,#26924,#26925,#26926,#26927,#26928,#26929,#26930,#26931,#26932,#26933,
#26934,#26935,#26936,#26937,#26938,#26939,#26940,#26941,#26942,#26943,#26944,
#26945,#26946,#26947,#26948,#26949,#26950,#26951,#26952,#26953,#26954,#26955,
#26956,#26957,#26958,#26959,#26960,#26961,#26962,#26963,#26964,#26965,#26966,
#26967,#26968,#26969,#26970,#26971,#26972,#26973,#26974,#26975,#26976,#26977,
#26978,#26979,#26980,#26981,#26982,#26983,#26984,#26985,#26986,#26987,#26988,
#26989,#26990,#26991,#26992,#26993,#26994,#26995,#26996,#26997,#26998,#26999,
#27000,#27001,#27002,#27003,#27004,#27005,#27006,#27007,#27008,#27009,#27010,
#27011,#27012,#27013,#27014,#27015,#27016,#27017,#27018,#27019,#27020,#27021,
#27022,#27023,#27024,#27025,#27026,#27027,#27028,#27029,#27030,#27031,#27032,
#27033,#27034,#27035,#27036,#27037,#27038,#27039,#27040,#27041,#27042,#27043,
#27044,#27045,#27046,#27047,#27048,#27049,#27050,#27051,#27052,#27053),
 .UNSPECIFIED.,.F.,.F.,(4,3,3,3,3,3,3,3,3,3,3,3,3,3,3,3,3,3,3,3,3,3,3,3,
3,3,3,3,3,3,3,3,3,3,3,3,3,3,3,3,3,3,3,3,3,3,3,3,3,3,3,3,3,3,3,3,3,3,3,3,
3,3,3,3,3,3,3,4),(20.5134609524394,20.6055499763409,20.6975652948072,20.7895411354812,
20.8815009324973,20.9734681009837,21.0655223439608,21.1576198991999,21.2498633183681,
21.3324662897441,21.4247413460989,21.5169004577346,21.6089696580682,21.7009783768828,
21.7929564372439,21.8849272484514,21.976914207601,22.0689933225765,22.1611236080645,
22.2533904918466,22.3021238483688,22.3942708610428,22.486301470765,22.5782418959037,
22.6701219740309,22.7619715389531,22.8538141643628,22.9456734120041,23.0376262965107,
23.1296310296129,23.2217745889557,23.2717814069936,23.3641777908133,23.4564576141058,
23.5486467453446,23.6407737348538,23.7328689752169,23.8249557259828,23.9170572335176,
24.0092481114704,24.1014887148543,24.1938626585338,24.2414389656183,24.3337905638608,
24.4260277122443,24.5181763073473,24.6102660719698,24.7023261537227,24.7943798433827,
24.8864504202011,24.9786137485308,25.0708286878585,25.1631801049782,25.211096524243,
25.3024910772515,25.3937689813926,25.4849573994033,25.5760894638707,25.6671936952272,
25.7582945058579,25.8494162995359,25.9406426849034,26.0319260146508,26.123363113343,
26.1807540828677,26.304510185502,26.4254147545538,26.4415719136207),
 .UNSPECIFIED.);
#1318=B_SPLINE_CURVE_WITH_KNOTS('',3,(#27054,#27055,#27056,#27057,#27058,
#27059,#27060,#27061,#27062,#27063,#27064,#27065,#27066,#27067,#27068,#27069,
#27070,#27071,#27072,#27073,#27074,#27075,#27076,#27077,#27078,#27079,#27080,
#27081,#27082,#27083,#27084,#27085,#27086,#27087,#27088,#27089,#27090,#27091,
#27092,#27093,#27094,#27095,#27096,#27097,#27098,#27099,#27100,#27101,#27102,
#27103,#27104,#27105,#27106,#27107,#27108,#27109,#27110,#27111,#27112,#27113,
#27114,#27115,#27116,#27117,#27118,#27119,#27120,#27121,#27122,#27123,#27124,
#27125,#27126,#27127,#27128,#27129,#27130,#27131,#27132,#27133,#27134,#27135,
#27136,#27137,#27138,#27139,#27140,#27141,#27142,#27143,#27144,#27145,#27146,
#27147,#27148,#27149,#27150,#27151,#27152,#27153,#27154,#27155,#27156,#27157,
#27158,#27159,#27160,#27161,#27162,#27163,#27164,#27165,#27166,#27167,#27168,
#27169,#27170,#27171,#27172,#27173,#27174,#27175,#27176,#27177,#27178,#27179,
#27180,#27181,#27182,#27183),.UNSPECIFIED.,.F.,.F.,(4,2,2,2,2,2,2,2,2,2,
2,2,2,2,2,2,2,2,2,2,2,2,2,2,2,2,2,2,2,2,2,2,2,2,2,2,2,2,2,2,2,2,2,2,2,2,
2,2,2,2,2,2,2,2,2,2,2,2,2,2,2,2,2,2,4),(5.69838345838743,5.74060319572305,
5.7632661986444,5.78477844420156,5.82015647797038,5.872901481636,5.91300242004822,
5.92775728863181,5.94017853306185,5.96284937030756,5.99706344315429,6.06492185284883,
6.08901671388651,6.11001158146563,6.14035782781468,6.22316375865817,6.24842600679028,
6.26117260717653,6.27525839703446,6.31394127226314,6.39916694977668,6.4219244805174,
6.44339981060996,6.47836891746152,6.52983710275213,6.5724178679904,6.58698095509419,
6.59947360921006,6.62275706998295,6.69225512275375,6.73206194066716,6.75403029276206,
6.7760589413377,6.81646931902625,6.88902612054175,6.90993336052652,6.92215094092272,
6.93756675402472,6.95633575549997,7.00008115709449,7.05657043084698,7.07975117479927,
7.10102194001076,7.13411441019393,7.1914134114673,7.23069167280445,7.24554717201633,
7.25798769433682,7.28060404660744,7.31466797652171,7.38255608232399,7.40664697340677,
7.42771054494079,7.45833253357428,7.5427346644408,7.56670106682125,7.57927538580445,
7.59353989701433,7.63629384962888,7.71167534647685,7.7359192222688,7.75672995854454,
7.78615535500089,7.82354158989668,7.83324491651743),.UNSPECIFIED.);
#1319=B_SPLINE_CURVE_WITH_KNOTS('',3,(#27186,#27187,#27188,#27189,#27190,
#27191,#27192,#27193,#27194,#27195,#27196,#27197,#27198,#27199,#27200,#27201,
#27202,#27203,#27204,#27205,#27206,#27207,#27208,#27209,#27210,#27211,#27212,
#27213,#27214,#27215,#27216,#27217,#27218,#27219,#27220,#27221,#27222,#27223,
#27224,#27225,#27226,#27227),.UNSPECIFIED.,.F.,.F.,(4,2,2,2,2,2,2,2,2,2,
2,2,2,2,2,2,2,2,2,2,4),(7.83324491651743,7.88736378546632,7.90302452762842,
7.91511738014786,7.93479602143784,7.96188536926654,8.04728261795144,8.07014143595615,
8.0916925458198,8.12681613428747,8.17876006848774,8.21984831770643,8.23469331810836,
8.24749030579618,8.27182649576923,8.34803095583536,8.38138093447557,8.4029187966207,
8.42667316414753,8.48702841435749,8.53519991959206),.UNSPECIFIED.);
#1320=B_SPLINE_CURVE_WITH_KNOTS('',3,(#27230,#27231,#27232,#27233,#27234,
#27235,#27236,#27237,#27238,#27239),.UNSPECIFIED.,.F.,.F.,(4,2,2,2,4),(-0.120342605042655,
-0.0910596067984688,-0.0177190149419271,-0.0080247817111039,0.),
 .UNSPECIFIED.);
#1321=B_SPLINE_CURVE_WITH_KNOTS('',3,(#27242,#27243,#27244,#27245),
 .UNSPECIFIED.,.F.,.F.,(4,4),(33.9036448620551,34.557517409689),
 .UNSPECIFIED.);
#1322=B_SPLINE_CURVE_WITH_KNOTS('',3,(#27247,#27248,#27249,#27250,#27251,
#27252,#27253,#27254,#27255,#27256,#27257,#27258,#27259,#27260,#27261,#27262,
#27263,#27264,#27265,#27266,#27267,#27268,#27269,#27270,#27271,#27272,#27273,
#27274,#27275,#27276,#27277,#27278,#27279,#27280,#27281,#27282,#27283,#27284,
#27285,#27286,#27287,#27288,#27289,#27290,#27291,#27292,#27293,#27294,#27295,
#27296,#27297,#27298,#27299,#27300,#27301,#27302,#27303,#27304,#27305,#27306,
#27307,#27308,#27309,#27310,#27311,#27312,#27313,#27314,#27315,#27316,#27317,
#27318,#27319,#27320,#27321,#27322,#27323,#27324,#27325,#27326,#27327,#27328,
#27329,#27330,#27331,#27332,#27333,#27334,#27335,#27336,#27337,#27338,#27339,
#27340,#27341,#27342,#27343,#27344,#27345,#27346,#27347,#27348,#27349,#27350,
#27351,#27352,#27353,#27354,#27355,#27356,#27357,#27358,#27359,#27360,#27361,
#27362,#27363,#27364,#27365,#27366,#27367,#27368,#27369,#27370,#27371,#27372,
#27373,#27374,#27375,#27376,#27377,#27378,#27379,#27380,#27381,#27382,#27383,
#27384,#27385,#27386,#27387,#27388,#27389,#27390,#27391,#27392,#27393,#27394,
#27395,#27396,#27397,#27398,#27399,#27400,#27401,#27402,#27403,#27404,#27405,
#27406,#27407,#27408,#27409,#27410,#27411,#27412,#27413,#27414,#27415,#27416,
#27417,#27418),.UNSPECIFIED.,.F.,.F.,(4,3,3,3,3,3,3,3,3,3,3,3,3,3,3,3,3,
3,3,3,3,3,3,3,3,3,3,3,3,3,3,3,3,3,3,3,3,3,3,3,3,3,3,3,3,3,3,3,3,3,3,3,3,
3,3,3,3,4),(34.5575191894877,34.6769348838958,34.7619343778369,34.8499952335888,
34.9379496562291,35.0258202981564,35.1140417529446,35.2018216192856,35.2895904089036,
35.3773684781906,35.4659243427584,35.5538256903796,35.6427088134206,35.7315919364616,
35.8196619820676,35.9076258712916,35.9955062403964,36.0837241472326,36.1715143057049,
36.2592935793087,36.3470823108465,36.4356241069065,36.5235364515172,36.6123929733018,
36.7012494950864,36.7891973320126,36.8770385913154,36.9647960700815,37.0530599430352,
37.1407273852193,37.2283842340686,37.3160509754662,37.4047649950274,37.4925575294465,
37.5817322915788,37.6709070537111,37.7590928978415,37.8471720280796,37.9351669372927,
38.023341646673,38.1112438804587,38.1991340908128,38.2870324896825,38.3754155203458,
38.4634334250405,38.5519990186881,38.6405646123358,38.7277373495786,38.8148055298882,
38.9044381980817,38.9913694404484,39.0782741687425,39.1651736724377,39.2520892322613,
39.3390842030036,39.4261272395307,39.5132811504422,39.5318668754359),
 .UNSPECIFIED.);
#1323=B_SPLINE_CURVE_WITH_KNOTS('',3,(#27422,#27423,#27424,#27425,#27426,
#27427,#27428,#27429),.UNSPECIFIED.,.F.,.F.,(4,1,1,1,1,4),(34.5575191894877,
35.12931922981,36.0989767884347,37.0686343470595,38.0382919056842,39.0079494643089),
 .UNSPECIFIED.);
#1324=B_SPLINE_CURVE_WITH_KNOTS('',3,(#27430,#27431,#27432,#27433,#27434),
 .UNSPECIFIED.,.F.,.F.,(4,1,4),(33.9023219446702,34.1596616711853,34.5575191894877),
 .UNSPECIFIED.);
#1325=B_SPLINE_CURVE_WITH_KNOTS('',3,(#27560,#27561,#27562,#27563,#27564,
#27565,#27566,#27567,#27568,#27569,#27570,#27571,#27572,#27573,#27574,#27575,
#27576,#27577,#27578,#27579,#27580,#27581,#27582,#27583,#27584,#27585,#27586,
#27587,#27588,#27589,#27590,#27591,#27592,#27593,#27594,#27595,#27596,#27597,
#27598,#27599,#27600,#27601,#27602,#27603,#27604,#27605,#27606,#27607,#27608,
#27609,#27610,#27611,#27612,#27613,#27614,#27615,#27616,#27617,#27618,#27619,
#27620,#27621,#27622,#27623,#27624,#27625,#27626,#27627,#27628,#27629,#27630,
#27631,#27632,#27633,#27634,#27635,#27636,#27637,#27638,#27639,#27640,#27641,
#27642,#27643,#27644,#27645,#27646,#27647,#27648,#27649,#27650),
 .UNSPECIFIED.,.F.,.F.,(4,3,3,3,3,3,3,3,3,3,3,3,3,3,3,3,3,3,3,3,3,3,3,3,
3,3,3,3,3,3,4),(0.,0.0371673843853462,0.0748693007053213,0.112706345019989,
0.146754419031169,0.154576061769547,0.159872184166855,0.196816634794726,
0.233577891628905,0.269502801433578,0.298936453110779,0.306086760141218,
0.311219678986263,0.347080703449979,0.382941727913695,0.418958403167855,
0.449351754992565,0.454627452010795,0.489595285086492,0.524700175211502,
0.559247248798574,0.592850943657959,0.598655230831888,0.632673659813041,
0.665941928010469,0.67053803226665,0.677685069465016,0.685585591405337,
0.718097783781032,0.733842861978519,0.7607598169945),.UNSPECIFIED.);
#1326=B_SPLINE_CURVE_WITH_KNOTS('',3,(#27651,#27652,#27653,#27654),
 .UNSPECIFIED.,.F.,.F.,(4,4),(-0.0128693341657787,0.),.UNSPECIFIED.);
#1327=B_SPLINE_CURVE_WITH_KNOTS('',3,(#27655,#27656,#27657,#27658,#27659,
#27660,#27661,#27662,#27663,#27664,#27665,#27666,#27667,#27668,#27669,#27670,
#27671,#27672,#27673,#27674,#27675,#27676,#27677,#27678,#27679,#27680,#27681,
#27682,#27683,#27684,#27685,#27686,#27687,#27688,#27689,#27690,#27691,#27692,
#27693,#27694,#27695,#27696,#27697,#27698,#27699,#27700,#27701,#27702,#27703,
#27704,#27705,#27706,#27707,#27708,#27709,#27710,#27711,#27712,#27713,#27714,
#27715,#27716,#27717,#27718,#27719,#27720,#27721,#27722,#27723,#27724,#27725,
#27726,#27727,#27728,#27729,#27730,#27731,#27732,#27733,#27734,#27735,#27736,
#27737,#27738,#27739,#27740,#27741,#27742),.UNSPECIFIED.,.F.,.F.,(4,3,3,
3,3,3,3,3,3,3,3,3,3,3,3,3,3,3,3,3,3,3,3,3,3,3,3,3,3,4),(2.84112346422651E-15,
0.0321878095080291,0.0648568461842673,0.0983283809336569,0.128751238032108,
0.1340110409187,0.14433350266263,0.178553412701981,0.213220662816023,0.246728237516609,
0.272650549117548,0.278294855644787,0.29438467656025,0.329979550746285,
0.347250961618367,0.382122925792846,0.414901056202246,0.421530557898444,
0.45684142113921,0.49289896799214,0.529433101181703,0.562152125203941,0.568353583238998,
0.605677260428984,0.642991738905437,0.660309197270654,0.666091466789222,
0.703920126902519,0.725827582042816,0.757732684314163),.UNSPECIFIED.);
#1328=B_SPLINE_CURVE_WITH_KNOTS('',3,(#27867,#27868,#27869,#27870,#27871,
#27872,#27873,#27874,#27875,#27876,#27877,#27878,#27879,#27880,#27881,#27882,
#27883,#27884,#27885,#27886,#27887,#27888,#27889,#27890,#27891,#27892,#27893,
#27894,#27895,#27896,#27897,#27898,#27899,#27900,#27901,#27902,#27903,#27904,
#27905,#27906,#27907,#27908,#27909,#27910,#27911,#27912,#27913,#27914,#27915,
#27916,#27917,#27918,#27919,#27920,#27921,#27922,#27923,#27924,#27925,#27926,
#27927,#27928,#27929,#27930,#27931,#27932,#27933,#27934,#27935,#27936,#27937,
#27938,#27939,#27940,#27941,#27942,#27943,#27944,#27945,#27946,#27947,#27948,
#27949,#27950,#27951,#27952,#27953,#27954,#27955,#27956,#27957),
 .UNSPECIFIED.,.F.,.F.,(4,3,3,3,3,3,3,3,3,3,3,3,3,3,3,3,3,3,3,3,3,3,3,3,
3,3,3,3,3,3,4),(0.,0.0321876396051637,0.0648564132377103,0.0983277964673542,
0.128750558420655,0.134005598284691,0.143992997014492,0.178320378143294,
0.212997816940641,0.247571536985515,0.268680605758807,0.273376200123601,
0.2783803293651,0.314015287499765,0.347250961618176,0.382123065927106,0.414901307298664,
0.421530568332327,0.456928426576089,0.492963289038479,0.529560343224023,
0.553903620195441,0.562418678032901,0.567813497614329,0.605133071291381,
0.642450419073943,0.660309272119139,0.666091576557883,0.703920232934646,
0.725827582042572,0.757703647974356),.UNSPECIFIED.);
#1329=B_SPLINE_CURVE_WITH_KNOTS('',3,(#27958,#27959,#27960,#27961,#27962,
#27963,#27964,#27965,#27966,#27967,#27968,#27969,#27970,#27971,#27972,#27973,
#27974,#27975,#27976,#27977,#27978,#27979,#27980,#27981,#27982,#27983,#27984,
#27985,#27986,#27987,#27988,#27989,#27990,#27991,#27992,#27993,#27994,#27995,
#27996,#27997,#27998,#27999,#28000,#28001,#28002,#28003,#28004,#28005,#28006,
#28007,#28008,#28009,#28010,#28011,#28012,#28013,#28014,#28015,#28016,#28017,
#28018,#28019,#28020,#28021,#28022,#28023,#28024,#28025,#28026,#28027,#28028,
#28029,#28030,#28031,#28032,#28033,#28034,#28035,#28036,#28037,#28038,#28039,
#28040,#28041,#28042,#28043,#28044,#28045),.UNSPECIFIED.,.F.,.F.,(4,3,3,
3,3,3,3,3,3,3,3,3,3,3,3,3,3,3,3,3,3,3,3,3,3,3,3,3,3,4),(2.19148179006735E-15,
0.0367103964528547,0.0744331778325135,0.112337565911546,0.149893962136006,
0.154575496994253,0.159872057743945,0.196816523045437,0.233577852742176,
0.269502850644212,0.298936418321743,0.306086670949945,0.311219649844233,
0.347080688878984,0.382941727913735,0.418958395967714,0.449351764007576,
0.454627460526605,0.489595295166872,0.524700180321969,0.559247313820411,
0.59285103833404,0.598655234317479,0.632644611325471,0.665820672120261,
0.677685668474962,0.683715521223274,0.716251000825657,0.733842861978756,
0.760759816994732),.UNSPECIFIED.);
#1330=B_SPLINE_CURVE_WITH_KNOTS('',3,(#28117,#28118,#28119,#28120,#28121,
#28122),.UNSPECIFIED.,.F.,.F.,(4,1,1,4),(36.7819582801311,37.0686343470595,
38.0382919056842,39.0079494643089),.UNSPECIFIED.);
#1331=B_SPLINE_CURVE_WITH_KNOTS('',3,(#28125,#28126,#28127,#28128,#28129,
#28130,#28131,#28132,#28133,#28134,#28135,#28136,#28137,#28138,#28139,#28140,
#28141,#28142,#28143,#28144,#28145,#28146,#28147,#28148,#28149,#28150,#28151,
#28152,#28153,#28154,#28155,#28156,#28157,#28158,#28159,#28160,#28161,#28162,
#28163,#28164,#28165,#28166,#28167,#28168,#28169,#28170,#28171,#28172,#28173,
#28174,#28175,#28176,#28177,#28178,#28179,#28180,#28181,#28182,#28183,#28184,
#28185,#28186,#28187,#28188,#28189,#28190,#28191,#28192,#28193,#28194,#28195,
#28196,#28197,#28198,#28199,#28200,#28201,#28202,#28203,#28204,#28205,#28206,
#28207,#28208,#28209,#28210,#28211,#28212,#28213,#28214,#28215,#28216,#28217,
#28218,#28219,#28220,#28221),.UNSPECIFIED.,.F.,.F.,(4,3,3,3,3,3,3,3,3,3,
3,3,3,3,3,3,3,3,3,3,3,3,3,3,3,3,3,3,3,3,3,3,4),(36.7829914305774,36.8708819232571,
36.9586870217953,37.0477145257848,37.1354254541176,37.2231243381835,37.31083161634,
37.4008504756827,37.4886815057119,37.5797942797115,37.6709070537111,37.759070730442,
37.847128117236,37.9351017332666,38.0232845931502,38.1111667826965,38.1990374597897,
38.2869168614638,38.3753287991818,38.4633292016657,38.5519469070008,38.6405646123358,
38.7276206141432,38.8145723290877,38.9042341473813,38.9910502374452,39.0778404802797,
39.1646262745643,39.2514290109438,39.3383129672329,39.425245923642,39.5122918403307,
39.5318668754359),.UNSPECIFIED.);
#1332=B_SPLINE_CURVE_WITH_KNOTS('',3,(#28227,#28228,#28229,#28230,#28231,
#28232,#28233,#28234,#28235,#28236,#28237,#28238,#28239,#28240,#28241,#28242,
#28243,#28244,#28245,#28246,#28247,#28248,#28249,#28250,#28251,#28252,#28253,
#28254,#28255,#28256,#28257,#28258,#28259,#28260,#28261,#28262,#28263,#28264,
#28265,#28266,#28267,#28268,#28269,#28270,#28271,#28272,#28273,#28274,#28275,
#28276,#28277,#28278,#28279,#28280,#28281,#28282,#28283,#28284,#28285,#28286,
#28287,#28288,#28289,#28290,#28291,#28292,#28293,#28294,#28295,#28296,#28297,
#28298,#28299,#28300,#28301,#28302,#28303,#28304,#28305,#28306,#28307,#28308,
#28309,#28310,#28311,#28312,#28313,#28314,#28315,#28316,#28317,#28318,#28319,
#28320,#28321,#28322,#28323,#28324,#28325,#28326,#28327,#28328,#28329,#28330,
#28331,#28332,#28333,#28334,#28335,#28336,#28337,#28338,#28339,#28340,#28341,
#28342,#28343,#28344,#28345,#28346,#28347,#28348,#28349,#28350,#28351,#28352,
#28353,#28354,#28355,#28356,#28357,#28358,#28359,#28360,#28361,#28362,#28363,
#28364,#28365,#28366,#28367,#28368),.UNSPECIFIED.,.F.,.F.,(4,3,3,3,3,3,
3,3,3,3,3,3,3,3,3,3,3,3,3,3,3,3,3,3,3,3,3,3,3,3,3,3,3,3,3,3,3,3,3,3,3,3,
3,3,3,3,3,4),(30.4999802413289,30.5878062964545,30.6755881792872,30.7633486037829,
30.8511079442691,30.9388865691735,31.02675362669,31.1146697101077,31.2027123231484,
31.2506889953111,31.3387311548989,31.426666934949,31.5145190110592,31.6027474539188,
31.6905090631315,31.7782597453881,31.8660198781115,31.9546015470676,32.0424855397654,
32.1314160468506,32.2203465539358,32.3084047690471,32.3963565839447,32.4842246535543,
32.5724470859301,32.6602244808093,32.7479908409051,32.8357665249892,32.9243259218821,
33.0122250125786,33.1011145625696,33.1900041125605,33.2780544852982,33.365998586373,
33.4538590783409,33.5420844024465,33.6298545967303,33.71761391022,33.805382708972,
33.8939524495253,33.9818451089349,34.0707533900601,34.1596616711853,34.259126012611,
34.3554308697042,34.4564749532961,34.5521891341409,34.5575190368881),
 .UNSPECIFIED.);
#1333=B_SPLINE_CURVE_WITH_KNOTS('',3,(#28369,#28370,#28371,#28372,#28373,
#28374),.UNSPECIFIED.,.F.,.F.,(4,1,1,4),(34.5575191894877,35.12931922981,
36.0989767884347,36.7819582801311),.UNSPECIFIED.);
#1334=B_SPLINE_CURVE_WITH_KNOTS('',3,(#28376,#28377,#28378,#28379,#28380,
#28381,#28382,#28383,#28384,#28385,#28386,#28387,#28388,#28389,#28390,#28391,
#28392,#28393,#28394,#28395,#28396,#28397,#28398,#28399,#28400,#28401,#28402,
#28403,#28404,#28405,#28406,#28407,#28408,#28409,#28410,#28411,#28412,#28413,
#28414,#28415,#28416,#28417,#28418,#28419,#28420,#28421,#28422,#28423,#28424,
#28425,#28426,#28427,#28428,#28429,#28430,#28431,#28432,#28433,#28434,#28435,
#28436,#28437,#28438,#28439,#28440,#28441,#28442,#28443,#28444,#28445,#28446,
#28447,#28448,#28449,#28450,#28451),.UNSPECIFIED.,.F.,.F.,(4,3,3,3,3,3,
3,3,3,3,3,3,3,3,3,3,3,3,3,3,3,3,3,3,3,4),(34.5575191894877,34.6769472396894,
34.7619343778369,34.8499925930133,34.9379444079826,35.0258124776704,35.1140349100193,
35.2018123049931,35.28957866519,35.3773543493816,35.4659137461516,35.5538128369715,
35.6427023867165,35.7315919364616,35.8196423109753,35.9075864138477,35.9954469076329,
36.0836722310646,36.1714424272047,36.2592017425627,36.3469705431935,36.4355402811667,
36.5234329424662,36.6123412187763,36.7012494950864,36.7829914305774),
 .UNSPECIFIED.);
#1335=B_SPLINE_CURVE_WITH_KNOTS('',3,(#28452,#28453,#28454,#28455,#28456,
#28457,#28458,#28459,#28460,#28461,#28462,#28463,#28464,#28465,#28466,#28467,
#28468,#28469,#28470,#28471,#28472,#28473,#28474,#28475,#28476,#28477,#28478,
#28479,#28480,#28481,#28482,#28483,#28484,#28485,#28486,#28487,#28488,#28489,
#28490,#28491,#28492,#28493,#28494,#28495,#28496,#28497,#28498,#28499,#28500,
#28501,#28502,#28503,#28504,#28505,#28506,#28507,#28508,#28509,#28510,#28511,
#28512,#28513,#28514,#28515,#28516,#28517,#28518,#28519,#28520,#28521,#28522,
#28523,#28524,#28525,#28526,#28527,#28528,#28529,#28530,#28531,#28532,#28533,
#28534,#28535,#28536,#28537,#28538,#28539,#28540,#28541,#28542,#28543,#28544,
#28545,#28546,#28547,#28548,#28549,#28550,#28551,#28552,#28553,#28554,#28555,
#28556,#28557,#28558,#28559,#28560,#28561,#28562,#28563,#28564,#28565,#28566,
#28567,#28568,#28569,#28570,#28571,#28572,#28573,#28574,#28575,#28576,#28577,
#28578,#28579,#28580,#28581,#28582,#28583,#28584,#28585,#28586,#28587,#28588,
#28589,#28590,#28591,#28592,#28593),.UNSPECIFIED.,.F.,.F.,(4,3,3,3,3,3,
3,3,3,3,3,3,3,3,3,3,3,3,3,3,3,3,3,3,3,3,3,3,3,3,3,3,3,3,3,3,3,3,3,3,3,3,
3,3,3,3,3,4),(30.4992051003504,30.586988429761,30.6748619877165,30.7627878035445,
30.8508361315155,30.883304143338,30.971351451518,31.0592923914219,31.1471496318142,
31.2353761405828,31.3231428902903,31.4108986944367,31.4986639243403,31.5872383687459,
31.6751273510732,31.764044526518,31.8529617019627,31.9410103456195,32.0289526183393,
32.1168111872057,32.2050371963784,32.2928052552214,32.3805623588041,32.4683288769244,
32.5569014728401,32.6447917041248,32.7337054823561,32.8226192605874,32.9106680482244,
32.9986104795465,33.0864692212407,33.1746951709871,33.2624634359629,33.350220757762,
33.4379875058746,33.526559834209,33.6144503220714,33.7033635706418,33.7922768192122,
33.8791556016581,33.9659061262488,34.0525836832044,34.139209898208,34.2258063494768,
34.3124246592063,34.3990516191918,34.4857583354495,34.5575191893441),
 .UNSPECIFIED.);
#1336=B_SPLINE_CURVE_WITH_KNOTS('',3,(#28599,#28600,#28601,#28602,#28603,
#28604,#28605,#28606,#28607,#28608,#28609,#28610,#28611,#28612,#28613,#28614,
#28615,#28616,#28617,#28618,#28619,#28620,#28621,#28622,#28623,#28624,#28625,
#28626,#28627,#28628,#28629,#28630,#28631,#28632,#28633,#28634,#28635,#28636,
#28637,#28638,#28639,#28640,#28641,#28642,#28643,#28644,#28645,#28646,#28647,
#28648,#28649,#28650,#28651,#28652,#28653,#28654,#28655,#28656,#28657,#28658,
#28659,#28660,#28661,#28662,#28663,#28664,#28665,#28666,#28667,#28668,#28669,
#28670,#28671,#28672,#28673,#28674,#28675,#28676,#28677,#28678,#28679,#28680,
#28681,#28682,#28683,#28684,#28685,#28686,#28687,#28688,#28689,#28690,#28691,
#28692,#28693,#28694,#28695,#28696,#28697,#28698,#28699,#28700,#28701,#28702,
#28703,#28704,#28705,#28706,#28707,#28708,#28709,#28710,#28711,#28712,#28713,
#28714,#28715,#28716,#28717,#28718,#28719,#28720,#28721,#28722,#28723,#28724,
#28725,#28726,#28727,#28728,#28729,#28730,#28731,#28732,#28733,#28734,#28735,
#28736,#28737,#28738,#28739,#28740),.UNSPECIFIED.,.F.,.F.,(4,3,3,3,3,3,
3,3,3,3,3,3,3,3,3,3,3,3,3,3,3,3,3,3,3,3,3,3,3,3,3,3,3,3,3,3,3,3,3,3,3,3,
3,3,3,3,3,4),(24.2157887599059,24.303689123736,24.3917223366668,24.4630860849379,
24.5511339407958,24.6390754281485,24.7269332150507,24.8151595186147,24.9029268088915,
24.9906831503585,25.0784489136963,25.1670225961629,25.2549120974833,25.343827870523,
25.4327436435627,25.5207914947271,25.6087329783038,25.6965907623439,25.7848170673243,
25.8725843569884,25.9603406986909,26.0481064631111,26.1366801478801,26.224569652357,
26.3134854272722,26.4024012021874,26.4904491403875,26.5783907104697,26.6662485803799,
26.754474852934,26.8422422263594,26.9299986508759,27.0177644970671,27.1063380630033,
27.1942276459502,27.2831432033812,27.3720587608121,27.4592850110154,27.5464051922551,
27.63739627849,27.7243753691936,27.811326806192,27.8982718392512,27.985231708504,
28.0722711378777,28.1593574305664,28.2465577551069,28.2743338821347),
 .UNSPECIFIED.);
#1337=B_SPLINE_CURVE_WITH_KNOTS('',3,(#28741,#28742,#28743,#28744,#28745,
#28746,#28747,#28748,#28749,#28750,#28751,#28752,#28753,#28754,#28755,#28756,
#28757,#28758,#28759,#28760,#28761,#28762,#28763,#28764,#28765,#28766,#28767,
#28768,#28769,#28770,#28771,#28772,#28773,#28774,#28775,#28776,#28777,#28778,
#28779,#28780,#28781,#28782,#28783,#28784,#28785,#28786,#28787,#28788,#28789,
#28790,#28791,#28792,#28793,#28794,#28795,#28796,#28797,#28798,#28799,#28800,
#28801,#28802,#28803,#28804,#28805,#28806,#28807,#28808,#28809,#28810,#28811,
#28812,#28813,#28814,#28815,#28816,#28817,#28818,#28819),.UNSPECIFIED.,
 .F.,.F.,(4,3,3,3,3,3,3,3,3,3,3,3,3,3,3,3,3,3,3,3,3,3,3,3,3,3,4),(28.2743338823081,
28.3417163194369,28.429763627663,28.5177045676132,28.6055618080517,28.6937883168029,
28.7815550665564,28.8693108707486,28.9570761006978,29.0456505450387,29.1335395274105,
29.2224567027361,29.3113738780616,29.3994225216949,29.4873647943923,29.575223363237,
29.6634493724182,29.7512174312415,29.8389745348052,29.9267410529077,30.0153136488524,
30.1032038801215,30.1921176584039,30.2810314366863,30.3690856030647,30.4570218464002,
30.4999802413289),.UNSPECIFIED.);
#1338=B_SPLINE_CURVE_WITH_KNOTS('',3,(#28821,#28822,#28823,#28824,#28825,
#28826,#28827,#28828,#28829,#28830,#28831,#28832,#28833,#28834,#28835,#28836,
#28837,#28838,#28839,#28840,#28841,#28842,#28843,#28844,#28845,#28846,#28847,
#28848,#28849,#28850,#28851,#28852,#28853,#28854,#28855,#28856,#28857,#28858,
#28859,#28860,#28861,#28862,#28863,#28864,#28865,#28866,#28867,#28868,#28869,
#28870,#28871,#28872,#28873,#28874,#28875,#28876,#28877,#28878,#28879,#28880,
#28881,#28882,#28883,#28884,#28885,#28886,#28887,#28888,#28889,#28890,#28891,
#28892,#28893,#28894,#28895,#28896,#28897,#28898,#28899),.UNSPECIFIED.,
 .F.,.F.,(4,3,3,3,3,3,3,3,3,3,3,3,3,3,3,3,3,3,3,3,3,3,3,3,3,3,4),(28.2743338823081,
28.3617389036755,28.4491201917934,28.5364985207119,28.6238946573556,28.711380340344,
28.7989143739467,28.8865805773436,28.9439890260885,29.0320369642888,29.1199785343708,
29.2078364042814,29.2960626768354,29.3838300502608,29.4715864747772,29.5593523209684,
29.6479258869046,29.7358154698515,29.8247310272824,29.9136465847132,30.0016844203211,
30.089621717054,30.177479011169,30.2652759791166,30.3530368519356,30.4407979020362,
30.4992051003504),.UNSPECIFIED.);
#1339=B_SPLINE_CURVE_WITH_KNOTS('',3,(#28900,#28901,#28902,#28903,#28904,
#28905,#28906,#28907,#28908,#28909,#28910,#28911,#28912,#28913,#28914,#28915,
#28916,#28917,#28918,#28919,#28920,#28921,#28922,#28923,#28924,#28925,#28926,
#28927,#28928,#28929,#28930,#28931,#28932,#28933,#28934,#28935,#28936,#28937,
#28938,#28939,#28940,#28941,#28942,#28943,#28944,#28945,#28946,#28947,#28948,
#28949,#28950,#28951,#28952,#28953,#28954,#28955,#28956,#28957,#28958,#28959,
#28960,#28961,#28962,#28963,#28964,#28965,#28966,#28967,#28968,#28969,#28970,
#28971,#28972,#28973,#28974,#28975,#28976,#28977,#28978,#28979,#28980,#28981,
#28982,#28983,#28984,#28985,#28986,#28987,#28988,#28989,#28990,#28991,#28992,
#28993,#28994,#28995,#28996,#28997,#28998,#28999,#29000,#29001,#29002,#29003,
#29004,#29005,#29006,#29007,#29008,#29009,#29010,#29011,#29012,#29013,#29014,
#29015,#29016,#29017,#29018,#29019,#29020,#29021,#29022,#29023,#29024,#29025,
#29026,#29027,#29028,#29029,#29030,#29031,#29032,#29033,#29034,#29035,#29036,
#29037,#29038),.UNSPECIFIED.,.F.,.F.,(4,3,3,3,3,3,3,3,3,3,3,3,3,3,3,3,3,
3,3,3,3,3,3,3,3,3,3,3,3,3,3,3,3,3,3,3,3,3,3,3,3,3,3,3,3,3,4),(24.2167210304736,
24.3046279764685,24.3924596906217,24.4802438127573,24.5680041412365,24.6557610538041,
24.7435349206615,24.8313960220632,24.9193040568845,25.0073412999443,25.0653587915896,
25.1534068139401,25.2413484697431,25.3292064268125,25.4174326672377,25.5052001307177,
25.592956646202,25.6807225841602,25.7692960256737,25.857185701481,25.9461010258477,
26.0350163502143,26.1230642813644,26.2110058457738,26.2988637113841,26.387089986066,
26.474857358571,26.5626137834407,26.6503796312588,26.7389532006539,26.8268427883422,
26.9157583485906,27.0046739088391,27.0927217646944,27.1806632520445,27.2685210389441,
27.3567473425091,27.444514632783,27.5322709742474,27.6200367375818,27.7086104200523,
27.7964999213698,27.8854156944168,27.9743314674638,28.0790231847901,28.1827305263691,
28.2743338820653),.UNSPECIFIED.);
#1340=B_SPLINE_CURVE_WITH_KNOTS('',3,(#29044,#29045,#29046,#29047,#29048,
#29049,#29050,#29051,#29052,#29053,#29054,#29055,#29056,#29057,#29058,#29059,
#29060,#29061,#29062,#29063,#29064,#29065,#29066,#29067,#29068,#29069,#29070,
#29071,#29072,#29073,#29074,#29075,#29076,#29077,#29078,#29079,#29080,#29081,
#29082,#29083,#29084,#29085,#29086,#29087,#29088,#29089,#29090,#29091,#29092,
#29093,#29094,#29095,#29096,#29097,#29098,#29099,#29100,#29101,#29102,#29103,
#29104,#29105,#29106,#29107,#29108,#29109,#29110,#29111,#29112,#29113,#29114,
#29115,#29116,#29117,#29118,#29119,#29120,#29121,#29122),.UNSPECIFIED.,
 .F.,.F.,(4,3,3,3,3,3,3,3,3,3,3,3,3,3,3,3,3,3,3,3,3,3,3,3,3,3,4),(15.707963267949,
15.7957710138543,15.8835745324552,15.9713940336816,16.063155716253,16.1511191802592,
16.2391470622587,16.3273025206811,16.338440763967,16.4264705709007,16.5143915318638,
16.6022263810891,16.6904603737769,16.7781990734251,16.8659247701018,16.9536578857083,
17.0422679949292,17.1301202964837,17.2191093095377,17.3080983225917,17.3962407088205,
17.4842848625976,17.5722511788473,17.6623720645742,17.7502488322418,17.8414917769983,
17.9327347217548),.UNSPECIFIED.);
#1341=B_SPLINE_CURVE_WITH_KNOTS('',3,(#29124,#29125,#29126,#29127,#29128,
#29129,#29130,#29131,#29132,#29133,#29134,#29135,#29136,#29137,#29138,#29139,
#29140,#29141,#29142,#29143,#29144,#29145,#29146,#29147,#29148,#29149,#29150,
#29151,#29152,#29153,#29154,#29155,#29156,#29157,#29158,#29159,#29160,#29161,
#29162,#29163,#29164,#29165,#29166,#29167,#29168,#29169),.UNSPECIFIED.,
 .F.,.F.,(4,3,3,3,3,3,3,3,3,3,3,3,3,3,3,4),(14.3991256467175,14.4887372625192,
14.5782938203675,14.6678142643898,14.7573380508082,14.846866749863,14.9364175372311,
15.0260076033398,15.1157142880607,15.2054812603592,15.2953997278843,15.3687832053423,
15.4680291464829,15.5669343832768,15.6652600362453,15.7079632677411),
 .UNSPECIFIED.);
#1342=B_SPLINE_CURVE_WITH_KNOTS('',3,(#29173,#29174,#29175,#29176,#29177,
#29178,#29179,#29180,#29181,#29182,#29183,#29184,#29185,#29186,#29187,#29188,
#29189,#29190,#29191,#29192,#29193,#29194,#29195,#29196,#29197,#29198,#29199,
#29200,#29201,#29202,#29203,#29204,#29205,#29206,#29207,#29208,#29209,#29210,
#29211,#29212,#29213,#29214,#29215,#29216,#29217,#29218,#29219,#29220,#29221,
#29222,#29223,#29224,#29225,#29226,#29227,#29228,#29229,#29230,#29231,#29232,
#29233,#29234,#29235,#29236,#29237,#29238,#29239),.UNSPECIFIED.,.F.,.F.,
(4,3,3,3,3,3,3,3,3,3,3,3,3,3,3,3,3,3,3,3,3,3,4),(13.8752082355906,13.9622520542611,
14.0491941465953,14.1388586906072,14.2256715524859,14.3124609367983,14.3992482407091,
14.4860548552488,14.5729461563241,14.6598884952872,14.7469466691964,14.7665104986906,
14.8542641117252,14.9419129820413,15.0294801549438,15.1169913640356,15.2044736406601,
15.2919477097064,15.3794342851205,15.4670040516123,15.5546174446298,15.642360377797,
15.7079632677762),.UNSPECIFIED.);
#1343=B_SPLINE_CURVE_WITH_KNOTS('',3,(#29240,#29241,#29242,#29243,#29244,
#29245,#29246,#29247,#29248,#29249,#29250,#29251,#29252,#29253,#29254,#29255,
#29256,#29257,#29258,#29259,#29260,#29261,#29262,#29263,#29264,#29265,#29266,
#29267,#29268,#29269,#29270,#29271,#29272,#29273,#29274,#29275,#29276,#29277,
#29278,#29279,#29280,#29281,#29282,#29283,#29284,#29285,#29286,#29287,#29288,
#29289,#29290,#29291,#29292,#29293,#29294,#29295,#29296,#29297,#29298,#29299,
#29300,#29301,#29302,#29303,#29304,#29305,#29306,#29307,#29308,#29309,#29310,
#29311,#29312,#29313,#29314,#29315,#29316,#29317,#29318),.UNSPECIFIED.,
 .F.,.F.,(4,3,3,3,3,3,3,3,3,3,3,3,3,3,3,3,3,3,3,3,3,3,3,3,3,3,4),(15.707963267949,
15.7361680573154,15.8241610831544,15.9120470328636,15.9998486521347,16.0880957726104,
16.1758057263136,16.2635043973197,16.3512122236995,16.4398655717597,16.5276970079318,
16.616761311936,16.7058256159401,16.7938766861026,16.8818213483134,16.9696822656569,
17.0579073792704,17.1456776645914,17.2334369431071,17.3212055808951,17.4097749793125,
17.4976671696677,17.5865751721162,17.6754831745648,17.7635369171519,17.8514734423075,
17.9335803047654),.UNSPECIFIED.);
#1344=B_SPLINE_CURVE_WITH_KNOTS('',3,(#29324,#29325,#29326,#29327,#29328,
#29329,#29330,#29331,#29332,#29333,#29334,#29335,#29336,#29337,#29338,#29339,
#29340,#29341,#29342,#29343,#29344,#29345,#29346,#29347,#29348,#29349,#29350,
#29351,#29352,#29353,#29354,#29355,#29356,#29357,#29358,#29359,#29360,#29361,
#29362,#29363,#29364,#29365,#29366,#29367,#29368,#29369,#29370,#29371,#29372,
#29373,#29374,#29375,#29376,#29377,#29378,#29379,#29380,#29381,#29382,#29383,
#29384,#29385,#29386,#29387,#29388,#29389,#29390),.UNSPECIFIED.,.F.,.F.,
(4,3,3,3,3,3,3,3,3,3,3,3,3,3,3,3,3,3,3,3,3,3,4),(24.5162658903767,24.6082166985082,
24.7001384561039,24.7920546616798,24.8839888029008,24.9760185491963,25.0681011382561,
25.1603243519034,25.211096524243,25.3029055078245,25.3945969257777,25.4861975074927,
25.5777382907594,25.6692490484609,25.7607538070406,25.852276581861,25.9438972266317,
26.0355716555317,26.1273911794012,26.1807540828677,26.3014629469111,26.419796833611,
26.4415677385481),.UNSPECIFIED.);
#1345=B_SPLINE_CURVE_WITH_KNOTS('',3,(#29392,#29393,#29394,#29395,#29396,
#29397,#29398,#29399,#29400,#29401,#29402,#29403,#29404,#29405,#29406,#29407,
#29408,#29409),.UNSPECIFIED.,.F.,.F.,(4,2,2,2,2,2,2,2,4),(-0.241287041643189,
-0.201278706532095,-0.169751970886667,-0.147404851836541,-0.120690417364664,
-0.0894452412599869,-0.0185648330825772,-0.00833841566500538,0.),
 .UNSPECIFIED.);
#1346=B_SPLINE_CURVE_WITH_KNOTS('',3,(#29412,#29413,#29414,#29415,#29416,
#29417,#29418,#29419,#29420,#29421,#29422,#29423,#29424,#29425,#29426,#29427,
#29428,#29429,#29430,#29431,#29432,#29433,#29434,#29435,#29436,#29437,#29438,
#29439,#29440,#29441,#29442,#29443,#29444,#29445,#29446,#29447,#29448,#29449,
#29450,#29451,#29452,#29453,#29454,#29455,#29456,#29457,#29458,#29459,#29460,
#29461,#29462,#29463,#29464,#29465,#29466,#29467,#29468,#29469,#29470,#29471,
#29472,#29473,#29474,#29475,#29476,#29477,#29478,#29479,#29480,#29481,#29482,
#29483,#29484,#29485,#29486,#29487,#29488,#29489,#29490,#29491,#29492,#29493,
#29494,#29495,#29496,#29497,#29498,#29499),.UNSPECIFIED.,.F.,.F.,(4,2,2,
2,2,2,2,2,2,2,2,2,2,2,2,2,2,2,2,2,2,2,2,2,2,2,2,2,2,2,2,2,2,2,2,2,2,2,2,
2,2,2,2,4),(-2.95683205450919,-2.86790352209954,-2.83680152208547,-2.81554813900449,
-2.79126588069924,-2.72638080838598,-2.69160704482108,-2.66872106054633,
-2.65615319116664,-2.64105148047836,-2.56539716564425,-2.51854787912015,
-2.49584443926592,-2.47409451419977,-2.43754352803279,-2.36406204816355,
-2.34011675234167,-2.32748571753471,-2.31302440587022,-2.24660389965472,
-2.20875882479134,-2.17909299647199,-2.15819216538313,-2.13388645412246,
-2.05870209572999,-2.0158818595516,-2.00158111968677,-1.98895608666696,
-1.96546548961181,-1.90449453714366,-1.8590959800648,-1.8365639919602,-1.81484042688886,
-1.77798281779561,-1.70491213313605,-1.6810549345542,-1.66845638116302,
-1.65394117366334,-1.61494840554818,-1.56104678509474,-1.52528634866078,
-1.50368686658543,-1.48099447654482,-1.48084820763969),.UNSPECIFIED.);
#1347=B_SPLINE_CURVE_WITH_KNOTS('',3,(#29505,#29506,#29507,#29508,#29509,
#29510,#29511,#29512,#29513,#29514,#29515,#29516,#29517,#29518,#29519,#29520,
#29521,#29522,#29523,#29524,#29525,#29526,#29527,#29528,#29529,#29530,#29531,
#29532,#29533,#29534,#29535,#29536,#29537,#29538,#29539,#29540,#29541,#29542,
#29543,#29544,#29545,#29546,#29547,#29548,#29549,#29550,#29551,#29552,#29553,
#29554,#29555,#29556,#29557,#29558,#29559,#29560,#29561,#29562,#29563,#29564,
#29565,#29566,#29567,#29568,#29569,#29570,#29571),.UNSPECIFIED.,.F.,.F.,
(4,3,3,3,3,3,3,3,3,3,3,3,3,3,3,3,3,3,3,3,3,3,4),(18.2320682153439,18.3277809146069,
18.4234936138699,18.5157463972682,18.6078830172538,18.6999295422289,18.7919154110862,
18.8838705252868,18.9758183248721,19.0677822376285,19.1598383932109,19.25194573998,
19.3441899321623,19.3931511724946,19.4888064687578,19.5796902392352,19.6704968772054,
19.7612512482406,19.8519781640647,19.9427327251429,20.0335034792163,20.1243541251064,
20.1583935426),.UNSPECIFIED.);
#1348=B_SPLINE_CURVE_WITH_KNOTS('',3,(#29572,#29573,#29574,#29575,#29576,
#29577,#29578,#29579,#29580,#29581,#29582,#29583,#29584,#29585,#29586,#29587,
#29588,#29589,#29590,#29591,#29592,#29593,#29594,#29595,#29596,#29597,#29598,
#29599,#29600,#29601,#29602,#29603,#29604,#29605,#29606,#29607,#29608,#29609,
#29610,#29611,#29612,#29613,#29614,#29615,#29616,#29617,#29618,#29619,#29620,
#29621,#29622,#29623,#29624,#29625,#29626,#29627,#29628,#29629,#29630,#29631,
#29632,#29633,#29634,#29635,#29636,#29637,#29638,#29639,#29640,#29641,#29642,
#29643,#29644,#29645,#29646,#29647,#29648,#29649,#29650,#29651,#29652,#29653,
#29654,#29655,#29656,#29657,#29658,#29659,#29660,#29661,#29662,#29663,#29664,
#29665,#29666,#29667,#29668,#29669,#29670,#29671,#29672,#29673,#29674,#29675,
#29676,#29677,#29678,#29679,#29680,#29681,#29682,#29683,#29684,#29685,#29686,
#29687,#29688,#29689,#29690,#29691,#29692,#29693,#29694,#29695,#29696,#29697,
#29698,#29699,#29700,#29701,#29702,#29703,#29704,#29705,#29706,#29707,#29708,
#29709,#29710,#29711,#29712,#29713,#29714,#29715,#29716,#29717,#29718,#29719),
 .UNSPECIFIED.,.F.,.F.,(4,3,3,3,3,3,3,3,3,3,3,3,3,3,3,3,3,3,3,3,3,3,3,3,
3,3,3,3,3,3,3,3,3,3,3,3,3,3,3,3,3,3,3,3,3,3,3,3,3,4),(20.1583935427702,
20.2835238295359,20.3628087311194,20.4550713921864,20.5472178413458,20.6392741334725,
20.7312696360706,20.82323429651,20.9151915425651,21.0071647896763,21.0992300537185,
21.1913463922247,21.2835993107372,21.3324662897441,21.4247207357871,21.5168591112654,
21.6089074798315,21.7008953116684,21.7928524611761,21.8848023644005,21.9767684451869,
22.0688268502357,22.1609364952792,22.2531830376279,22.3021238483688,22.3943152466139,
22.4863902988358,22.5783751618252,22.6702994876033,22.7621931622762,22.8540797045629,
22.945982621076,23.0379785399895,23.130026004017,23.222211422785,23.2717814069936,
23.3641545650046,23.4564116286072,23.5485784965439,23.6406840587817,23.7327584028345,
23.8248248167588,23.9169065758691,24.0090787190171,24.1013011415748,24.193657934791,
24.2414389656183,24.3336416928871,24.4257215341127,24.5162658903767),
 .UNSPECIFIED.);
#1349=B_SPLINE_CURVE_WITH_KNOTS('',3,(#29721,#29722,#29723,#29724,#29725,
#29726,#29727,#29728,#29729,#29730,#29731,#29732,#29733,#29734,#29735,#29736,
#29737,#29738,#29739,#29740,#29741,#29742,#29743,#29744,#29745,#29746,#29747,
#29748,#29749,#29750,#29751,#29752,#29753,#29754,#29755,#29756,#29757,#29758,
#29759,#29760,#29761,#29762,#29763,#29764,#29765,#29766,#29767,#29768,#29769,
#29770,#29771,#29772,#29773,#29774,#29775,#29776,#29777,#29778,#29779,#29780,
#29781,#29782,#29783,#29784,#29785,#29786,#29787,#29788,#29789,#29790,#29791,
#29792,#29793,#29794,#29795,#29796,#29797,#29798,#29799,#29800,#29801,#29802,
#29803,#29804,#29805,#29806,#29807,#29808,#29809,#29810,#29811,#29812),
 .UNSPECIFIED.,.F.,.F.,(4,2,2,2,2,2,2,2,2,2,2,2,2,2,2,2,2,2,2,2,2,2,2,2,
2,2,2,2,2,2,2,2,2,2,2,2,2,2,2,2,2,2,2,2,2,4),(-1.48084820763969,-1.43329533170974,
-1.37132751089461,-1.35010317640515,-1.33794394056275,-1.32265784737522,
-1.30412790396548,-1.26164454881705,-1.20350041856723,-1.1802595174912,
-1.15895538514111,-1.12582808339709,-1.06670722704322,-1.02838445314857,
-1.01388575701412,-1.00131160682934,-0.977558379347592,-0.905174625587634,
-0.867656378337848,-0.845873370891219,-0.82346873664529,-0.779447826705011,
-0.699291096654322,-0.684670886669094,-0.672141558145518,-0.648769291765022,
-0.578828284061989,-0.539347239257186,-0.517362300251839,-0.495202218953017,
-0.453916966488133,-0.376883831426887,-0.359114276288713,-0.347065989059489,
-0.3294347080856,-0.3065446534078,-0.234282136893858,-0.203602891856948,
-0.182535210417779,-0.15847243035184,-0.131761322573367,-0.0735433135885103,
-0.0387754740265174,-0.0248091469507901,-0.0134569621051135,-0.000876788281526703),
 .UNSPECIFIED.);
#1350=B_SPLINE_CURVE_WITH_KNOTS('',3,(#29813,#29814,#29815,#29816,#29817,
#29818,#29819,#29820,#29821,#29822,#29823,#29824,#29825,#29826,#29827,#29828,
#29829,#29830,#29831,#29832,#29833,#29834,#29835,#29836,#29837,#29838,#29839,
#29840,#29841,#29842,#29843,#29844,#29845,#29846,#29847,#29848,#29849,#29850,
#29851,#29852),.UNSPECIFIED.,.F.,.F.,(4,2,2,2,2,2,2,2,2,2,2,2,2,2,2,2,2,
2,2,4),(-4.27008307975396,-4.19036405881084,-4.1501032589128,-4.12803790197118,
-4.10595437322849,-4.06549781421076,-3.99675679471902,-3.97357760736626,
-3.9610709666391,-3.94639393247533,-3.90500558091448,-3.85292088405322,
-3.81773409769697,-3.79619916165051,-3.77340722906428,-3.68808992672072,
-3.64942509893504,-3.63532334730152,-3.62253225736476,-3.61563567609935),
 .UNSPECIFIED.);
#1351=B_SPLINE_CURVE_WITH_KNOTS('',3,(#29858,#29859,#29860,#29861,#29862,
#29863,#29864,#29865,#29866,#29867,#29868,#29869,#29870,#29871,#29872,#29873,
#29874,#29875,#29876,#29877,#29878,#29879,#29880,#29881,#29882,#29883,#29884,
#29885,#29886,#29887,#29888,#29889,#29890,#29891,#29892,#29893,#29894,#29895,
#29896,#29897,#29898,#29899,#29900,#29901,#29902,#29903,#29904,#29905,#29906,
#29907,#29908,#29909,#29910,#29911,#29912,#29913,#29914,#29915,#29916,#29917,
#29918,#29919,#29920,#29921),.UNSPECIFIED.,.F.,.F.,(4,3,3,3,3,3,3,3,3,3,
3,3,3,3,3,3,3,3,3,3,3,4),(11.9498038827978,12.0417734588683,12.1337218267211,
12.2256724204771,12.3206413808882,12.4127165016283,12.5091323818749,12.6055482621215,
12.6978000692492,12.7899356996167,12.8819812232005,12.9739660775169,13.0659201695579,
13.1578669407371,13.249829820208,13.3418849413676,13.4339912517699,13.5262344142757,
13.5752058207462,13.6848961706205,13.7935323056319,13.8752082353862),
 .UNSPECIFIED.);
#1352=B_SPLINE_CURVE_WITH_KNOTS('',3,(#29922,#29923,#29924,#29925,#29926,
#29927,#29928,#29929,#29930,#29931,#29932,#29933,#29934,#29935,#29936,#29937,
#29938,#29939,#29940,#29941,#29942,#29943,#29944,#29945,#29946,#29947,#29948,
#29949,#29950,#29951,#29952,#29953,#29954,#29955,#29956,#29957,#29958,#29959,
#29960,#29961,#29962,#29963,#29964,#29965,#29966,#29967,#29968,#29969,#29970,
#29971,#29972,#29973,#29974,#29975,#29976,#29977,#29978,#29979,#29980,#29981,
#29982,#29983,#29984,#29985,#29986,#29987,#29988,#29989,#29990,#29991,#29992,
#29993,#29994,#29995,#29996,#29997,#29998,#29999,#30000,#30001,#30002,#30003,
#30004,#30005,#30006,#30007,#30008,#30009,#30010,#30011,#30012,#30013,#30014,
#30015,#30016,#30017,#30018,#30019,#30020,#30021,#30022,#30023,#30024,#30025,
#30026,#30027,#30028,#30029,#30030,#30031,#30032,#30033,#30034,#30035,#30036,
#30037,#30038,#30039,#30040,#30041,#30042,#30043,#30044,#30045,#30046,#30047,
#30048,#30049,#30050,#30051,#30052,#30053,#30054,#30055,#30056,#30057,#30058,
#30059,#30060,#30061,#30062,#30063,#30064,#30065,#30066,#30067,#30068,#30069,
#30070,#30071,#30072),.UNSPECIFIED.,.F.,.F.,(4,3,3,3,3,3,3,3,3,3,3,3,3,
3,3,3,3,3,3,3,3,3,3,3,3,3,3,3,3,3,3,3,3,3,3,3,3,3,3,3,3,3,3,3,3,3,3,3,3,
3,4),(13.8752082355906,13.966786515321,14.0583392857893,14.1498904407232,
14.2414638661191,14.3331348167784,14.4248632482533,14.5167262289635,14.544863379371,
14.6371152727752,14.7292509898415,14.8212966004213,14.9132815418156,15.0052357209429,
15.0971825791062,15.1891455453485,15.2812007524455,15.3733071484209,15.4655503951418,
15.5145209379957,15.6067729212884,15.6989087296117,15.7909544326659,15.8829394679299,
15.9748937417402,16.0668406952681,16.1588037574262,16.2508590606815,16.3429655530728,
16.4352088956974,16.4841784966204,16.5764297299234,16.6685647867363,16.7606097378519,
16.8525940237409,16.9445475501442,17.0364937592073,17.1284560808191,17.2205106539199,
17.3126164211333,17.404859053096,17.4538360552452,17.5461006300452,17.6382219581942,
17.7302613152847,17.8222422297013,17.9141881766539,18.0061482785894,18.0981158143603,
18.1901507760465,18.2320682153439),.UNSPECIFIED.);
#1353=B_SPLINE_CURVE_WITH_KNOTS('',3,(#30073,#30074,#30075,#30076,#30077,
#30078,#30079,#30080,#30081,#30082,#30083,#30084,#30085,#30086,#30087,#30088,
#30089,#30090,#30091,#30092,#30093,#30094,#30095,#30096,#30097,#30098,#30099,
#30100,#30101,#30102,#30103,#30104,#30105,#30106,#30107,#30108,#30109,#30110,
#30111,#30112,#30113,#30114,#30115,#30116,#30117,#30118,#30119,#30120,#30121,
#30122,#30123,#30124,#30125,#30126,#30127,#30128,#30129,#30130,#30131,#30132,
#30133,#30134,#30135,#30136,#30137,#30138,#30139,#30140,#30141,#30142,#30143,
#30144,#30145,#30146,#30147,#30148,#30149,#30150,#30151,#30152,#30153,#30154,
#30155,#30156,#30157,#30158,#30159,#30160,#30161,#30162,#30163,#30164,#30165,
#30166,#30167,#30168,#30169,#30170,#30171,#30172,#30173,#30174,#30175,#30176,
#30177,#30178,#30179,#30180,#30181,#30182,#30183,#30184,#30185,#30186,#30187,
#30188,#30189,#30190,#30191,#30192,#30193,#30194,#30195,#30196,#30197,#30198,
#30199,#30200,#30201,#30202),.UNSPECIFIED.,.F.,.F.,(4,2,2,2,2,2,2,2,2,2,
2,2,2,2,2,2,2,2,2,2,2,2,2,2,2,2,2,2,2,2,2,2,2,2,2,2,2,2,2,2,2,2,2,2,2,2,
2,2,2,2,2,2,2,2,2,2,2,2,2,2,2,2,2,2,4),(-3.61563567609935,-3.59707278652811,
-3.53670443164277,-3.4927916853173,-3.47039092706641,-3.44859865477452,
-3.41101756909211,-3.34862210908414,-3.32688633479163,-3.3098501478452,
-3.29778510175537,-3.27934071796878,-3.20328579142537,-3.16216848920136,
-3.14002029114605,-3.11801718888111,-3.07837698961676,-3.01848227903406,
-2.99707669182181,-2.98021466254453,-2.96814092523396,-2.94947755048121,
-2.87375295013127,-2.83269831188747,-2.81055657012403,-2.78854856362336,
-2.74885436654806,-2.67920456151832,-2.6558792618633,-2.64335492463655,
-2.62872161719908,-2.58676161681923,-2.5294746957831,-2.49745588185999,
-2.47625631513722,-2.45267124683846,-2.37896921866108,-2.34718790487122,
-2.32547563260878,-2.3131417310094,-2.29796159310292,-2.23913679044331,
-2.18003244284178,-2.1563477812173,-2.13518234071414,-2.10347915092546,
-2.06095557425161,-2.00579933929683,-1.99031568667032,-1.97806024715624,
-1.95707054386516,-1.92701113996785,-1.84865166362859,-1.82552256914947,
-1.80415534906218,-1.77051479778477,-1.72293991708584,-1.67699779514533,
-1.66125849499533,-1.64916906903982,-1.62885690363851,-1.60035004587229,
-1.52232246792104,-1.49831885547463,-1.48105208187109),.UNSPECIFIED.);
#1354=B_SPLINE_CURVE_WITH_KNOTS('',3,(#30208,#30209,#30210,#30211,#30212,
#30213,#30214,#30215,#30216,#30217,#30218,#30219,#30220,#30221,#30222,#30223,
#30224,#30225,#30226,#30227,#30228,#30229,#30230,#30231,#30232,#30233,#30234,
#30235,#30236,#30237,#30238,#30239,#30240,#30241,#30242,#30243,#30244,#30245,
#30246,#30247,#30248,#30249,#30250,#30251,#30252,#30253,#30254,#30255,#30256,
#30257,#30258,#30259,#30260,#30261,#30262,#30263,#30264,#30265,#30266,#30267,
#30268,#30269,#30270,#30271,#30272,#30273,#30274),.UNSPECIFIED.,.F.,.F.,
(4,3,3,3,3,3,3,3,3,3,3,3,3,3,3,3,3,3,3,3,3,3,4),(-1.92436839018911,-1.83258031210896,
-1.74090544344235,-1.64932058448165,-1.55778627637879,-1.46627808473474,
-1.37477198624503,-1.28324396560501,-1.19161600512138,-1.09993074983352,
-1.00810461130262,-0.96965755862473,-0.875424683643867,-0.781323325762907,
-0.683657910042544,-0.589768614211507,-0.495936151858874,-0.402140717131423,
-0.308362541712838,-0.214555248867951,-0.120731767065434,-0.0268415123618111,
0.),.UNSPECIFIED.);
#1355=B_SPLINE_CURVE_WITH_KNOTS('',3,(#30277,#30278,#30279,#30280,#30281,
#30282,#30283,#30284,#30285,#30286,#30287,#30288,#30289,#30290,#30291,#30292,
#30293,#30294,#30295,#30296,#30297,#30298,#30299,#30300,#30301,#30302,#30303,
#30304,#30305,#30306,#30307,#30308,#30309,#30310,#30311,#30312,#30313,#30314,
#30315,#30316,#30317,#30318,#30319,#30320,#30321,#30322,#30323,#30324,#30325,
#30326,#30327,#30328,#30329,#30330,#30331,#30332,#30333,#30334,#30335,#30336,
#30337,#30338,#30339,#30340,#30341,#30342,#30343,#30344,#30345,#30346,#30347,
#30348,#30349,#30350,#30351,#30352,#30353,#30354,#30355,#30356,#30357,#30358,
#30359,#30360,#30361,#30362,#30363,#30364,#30365,#30366,#30367,#30368,#30369,
#30370,#30371,#30372,#30373,#30374,#30375,#30376,#30377,#30378,#30379,#30380,
#30381,#30382,#30383,#30384,#30385,#30386,#30387,#30388,#30389,#30390,#30391,
#30392,#30393,#30394,#30395,#30396,#30397,#30398,#30399,#30400),
 .UNSPECIFIED.,.F.,.F.,(4,3,3,3,3,3,3,3,3,3,3,3,3,3,3,3,3,3,3,3,3,3,3,3,
3,3,3,3,3,3,3,3,3,3,3,3,3,3,3,3,3,4),(2.0176960437804,2.10889583919491,
2.19998459169105,2.29098582172404,2.38193982122487,2.47287122408923,2.56380463909107,
2.65481792315395,2.7458720173498,2.83706482123993,2.90897267587419,3.00133749550434,
3.09358792998079,3.18574987119399,3.27785305426829,3.36992659951255,3.46199379371309,
3.55407791216226,3.64625479384758,3.73848331266857,3.83084825439588,3.87863023449892,
3.97082459235909,4.06290199864244,4.15488861259772,4.24681378604394,4.33870774856359,
4.43059401932917,4.52249610496381,4.6144903485617,4.70653565631031,4.79871818850885,
4.84828779312365,4.94055232855515,5.03267482099036,5.12471616095592,5.2166998705942,
5.30864941974567,5.40062107605425,5.49260045125405,5.58466667839021,5.66572400274839),
 .UNSPECIFIED.);
#1356=B_SPLINE_CURVE_WITH_KNOTS('',3,(#30403,#30404,#30405,#30406,#30407,
#30408,#30409,#30410,#30411,#30412,#30413,#30414,#30415,#30416,#30417,#30418,
#30419,#30420,#30421,#30422,#30423,#30424,#30425,#30426,#30427,#30428,#30429,
#30430,#30431,#30432,#30433,#30434,#30435,#30436,#30437,#30438,#30439,#30440,
#30441,#30442,#30443,#30444,#30445,#30446,#30447,#30448,#30449,#30450,#30451,
#30452,#30453,#30454,#30455,#30456,#30457,#30458,#30459,#30460,#30461,#30462,
#30463,#30464,#30465,#30466,#30467,#30468,#30469),.UNSPECIFIED.,.F.,.F.,
(4,3,3,3,3,3,3,3,3,3,3,3,3,3,3,3,3,3,3,3,3,3,4),(5.66572400274839,5.75796559638503,
5.81794535174838,5.91020685033311,6.00235237503373,6.09440797976452,6.1864031499091,
6.27836769795418,6.37032505149634,6.4622986259719,6.55436454906352,6.64648173567859,
6.73873578885576,6.78760291037311,6.87854574101344,6.96935218416102,7.06008153265442,
7.1507587229741,7.24140863757461,7.33209537265635,7.42279809674976,7.51360445676476,
7.59202292823699),.UNSPECIFIED.);
#1357=B_SPLINE_CURVE_WITH_KNOTS('',3,(#30470,#30471,#30472,#30473,#30474,
#30475,#30476,#30477,#30478,#30479,#30480,#30481,#30482,#30483,#30484,#30485,
#30486,#30487,#30488,#30489,#30490,#30491,#30492,#30493,#30494,#30495,#30496,
#30497,#30498,#30499,#30500,#30501,#30502,#30503,#30504,#30505,#30506,#30507,
#30508,#30509,#30510,#30511,#30512,#30513,#30514,#30515,#30516,#30517,#30518,
#30519,#30520,#30521,#30522,#30523,#30524,#30525,#30526,#30527,#30528,#30529,
#30530,#30531,#30532,#30533,#30534,#30535,#30536,#30537,#30538,#30539,#30540,
#30541,#30542,#30543,#30544,#30545,#30546,#30547,#30548,#30549,#30550,#30551,
#30552,#30553,#30554,#30555,#30556,#30557,#30558,#30559,#30560,#30561,#30562,
#30563,#30564,#30565,#30566,#30567,#30568,#30569,#30570,#30571,#30572,#30573,
#30574,#30575,#30576,#30577,#30578,#30579,#30580,#30581,#30582,#30583,#30584,
#30585,#30586,#30587,#30588,#30589,#30590,#30591,#30592,#30593,#30594,#30595,
#30596,#30597,#30598,#30599,#30600,#30601,#30602,#30603,#30604,#30605,#30606,
#30607,#30608,#30609,#30610,#30611,#30612,#30613,#30614,#30615,#30616,#30617,
#30618,#30619,#30620),.UNSPECIFIED.,.F.,.F.,(4,3,3,3,3,3,3,3,3,3,3,3,3,
3,3,3,3,3,3,3,3,3,3,3,3,3,3,3,3,3,3,3,3,3,3,3,3,3,3,3,3,3,3,3,3,3,3,3,3,
3,4),(7.592022928411,7.73002674859181,7.75726046899785,7.84951329700286,
7.94164995246269,8.03369650381667,8.12568238543364,8.21763750395079,8.30958529941616,
8.40154919961633,8.49360532991555,8.58571264414763,8.67795679279574,8.72691802762258,
8.81917056833466,8.91130694839282,9.00335323657964,9.09533887448395,9.18729376149322,
9.27924133799731,9.37120503213437,9.46326097733344,9.55536811813824,9.64761211328743,
9.69657558624731,9.78882686092544,9.88096195064293,9.97300692622614,10.0649912239508,
10.1569447543583,10.2488909596008,10.340853269567,10.4329078192168,10.525013556251,
10.6172561478338,10.666233144872,10.7584851264444,10.8506209333997,10.9426666354368,
11.0346516702088,11.1266059438525,11.2185528975395,11.3105159601817,11.4025712644119,
11.4946777580579,11.5869211023612,11.6358907034968,11.7281280137823,11.820263349795,
11.9123037001377,11.9498038827978),.UNSPECIFIED.);
#1358=B_SPLINE_CURVE_WITH_KNOTS('',3,(#30622,#30623,#30624,#30625,#30626,
#30627,#30628,#30629,#30630,#30631,#30632,#30633,#30634,#30635,#30636,#30637,
#30638,#30639,#30640,#30641,#30642,#30643,#30644,#30645,#30646,#30647,#30648,
#30649,#30650,#30651,#30652,#30653,#30654,#30655,#30656,#30657,#30658,#30659,
#30660,#30661,#30662,#30663,#30664,#30665,#30666,#30667,#30668,#30669,#30670,
#30671,#30672,#30673,#30674,#30675,#30676,#30677,#30678,#30679,#30680,#30681,
#30682,#30683,#30684,#30685,#30686,#30687,#30688,#30689,#30690,#30691,#30692,
#30693,#30694,#30695,#30696,#30697,#30698,#30699,#30700,#30701,#30702,#30703,
#30704,#30705,#30706,#30707,#30708,#30709,#30710,#30711,#30712,#30713),
 .UNSPECIFIED.,.F.,.F.,(4,2,2,2,2,2,2,2,2,2,2,2,2,2,2,2,2,2,2,2,2,2,2,2,
2,2,2,2,2,2,2,2,2,2,2,2,2,2,2,2,2,2,2,2,2,4),(-1.48105208187109,-1.47723202852845,
-1.44638155789707,-1.36042020369283,-1.3378247980845,-1.32551240332599,
-1.31074165133099,-1.25968614889842,-1.19377480945142,-1.16948545946754,
-1.14847361746651,-1.11835730611952,-1.03710095242182,-1.01048351932531,
-0.997551245477823,-0.983677889304862,-0.948149263517353,-0.878152216446806,
-0.848263275169742,-0.827258278678024,-0.802834045623177,-0.775467624264196,
-0.714879430991743,-0.683780419244092,-0.669986975788721,-0.656964392336876,
-0.629700329593723,-0.58148735246408,-0.530544102745518,-0.507584410023389,
-0.486111062093909,-0.451603610301627,-0.401584260728747,-0.359850339699052,
-0.344145714276371,-0.332026565269392,-0.312215708944257,-0.28479702414513,
-0.200486142329031,-0.177699231763394,-0.156320302408579,-0.121906422413231,
-0.0623764867994372,-0.0255370712176183,-0.0117280735918997,-0.000901374079214656),
 .UNSPECIFIED.);
#1359=B_SPLINE_CURVE_WITH_KNOTS('',3,(#30714,#30715,#30716,#30717,#30718,
#30719,#30720,#30721,#30722,#30723,#30724,#30725,#30726,#30727,#30728,#30729,
#30730,#30731,#30732,#30733,#30734,#30735,#30736,#30737,#30738,#30739,#30740,
#30741,#30742,#30743,#30744,#30745,#30746,#30747,#30748,#30749,#30750,#30751,
#30752,#30753,#30754,#30755,#30756,#30757,#30758,#30759,#30760,#30761,#30762,
#30763,#30764,#30765,#30766,#30767,#30768,#30769,#30770,#30771,#30772,#30773,
#30774,#30775,#30776,#30777,#30778,#30779,#30780,#30781,#30782,#30783),
 .UNSPECIFIED.,.F.,.F.,(4,3,3,3,3,3,3,3,3,3,3,3,3,3,3,3,3,3,3,3,3,3,3,4),
(-3.85042544491851,-3.7584786014718,-3.66664683940555,-3.57193756896413,
-3.48025410630045,-3.38859847531267,-3.2969468418714,-3.20527538156021,
-3.11351194514312,-3.02169316046402,-2.92974733078309,-2.90897267587419,
-2.81676305457636,-2.72466756475499,-2.63266007968529,-2.54070992917899,
-2.44878844927304,-2.35687214176041,-2.26493751899187,-2.17290708811915,
-2.08082347305532,-1.98859964503748,-1.93931511724946,-1.92436839018911),
 .UNSPECIFIED.);
#1360=B_SPLINE_CURVE_WITH_KNOTS('',3,(#30786,#30787,#30788,#30789,#30790,
#30791,#30792,#30793,#30794,#30795,#30796,#30797,#30798,#30799,#30800,#30801,
#30802,#30803,#30804,#30805,#30806,#30807,#30808,#30809,#30810,#30811,#30812,
#30813,#30814,#30815,#30816,#30817,#30818,#30819,#30820,#30821,#30822,#30823,
#30824,#30825,#30826,#30827,#30828,#30829,#30830,#30831,#30832,#30833,#30834,
#30835,#30836,#30837,#30838,#30839,#30840,#30841,#30842,#30843,#30844,#30845,
#30846,#30847,#30848,#30849,#30850,#30851,#30852,#30853,#30854,#30855,#30856,
#30857,#30858,#30859,#30860,#30861,#30862,#30863,#30864,#30865,#30866,#30867,
#30868,#30869,#30870,#30871,#30872,#30873,#30874,#30875,#30876,#30877,#30878,
#30879,#30880,#30881,#30882,#30883,#30884,#30885,#30886,#30887,#30888,#30889,
#30890,#30891,#30892,#30893,#30894,#30895,#30896,#30897,#30898,#30899,#30900,
#30901,#30902,#30903,#30904,#30905,#30906,#30907,#30908,#30909,#30910,#30911,
#30912,#30913,#30914,#30915,#30916,#30917,#30918,#30919,#30920,#30921,#30922,
#30923,#30924),.UNSPECIFIED.,.F.,.F.,(4,3,3,3,3,3,3,3,3,3,3,3,3,3,3,3,3,
3,3,3,3,3,3,3,3,3,3,3,3,3,3,3,3,3,3,3,3,3,3,3,3,3,3,3,3,3,4),(17.9335803047654,
18.0225253583185,18.1103038525756,18.1980703397971,18.2858451790672,18.3756690675978,
18.4635667843356,18.5543537587626,18.6451407331896,18.7331832167028,18.8211192573837,
18.9089715310756,18.997199876168,19.0849615276785,19.1727121937118,19.2604722517004,
19.3490537617289,19.4369375365909,19.5258679142026,19.6147982918143,19.7028471218928,
19.7907895873348,19.8786483548595,19.9668742918069,20.0546425621996,20.1423998817223,
20.230166619867,20.31873892751,20.406629386596,20.4955426185175,20.584455850439,
20.6725044064358,20.7604466086221,20.8483051240143,20.9365311596455,21.0242992070283,
21.1120563149855,21.1998228533126,21.2883954922504,21.3762857824584,21.4651995957611,
21.5541134090638,21.6485773884456,21.7427641575297,21.8367783692867,21.9305359866766,
21.9911485749473),.UNSPECIFIED.);
#1361=B_SPLINE_CURVE_WITH_KNOTS('',3,(#30925,#30926,#30927,#30928,#30929,
#30930,#30931,#30932,#30933,#30934,#30935,#30936,#30937,#30938,#30939,#30940,
#30941,#30942,#30943,#30944,#30945,#30946,#30947,#30948,#30949,#30950,#30951,
#30952,#30953,#30954,#30955,#30956,#30957,#30958,#30959,#30960,#30961,#30962,
#30963,#30964,#30965,#30966,#30967,#30968,#30969,#30970,#30971,#30972,#30973,
#30974,#30975,#30976,#30977,#30978,#30979,#30980,#30981,#30982,#30983,#30984,
#30985,#30986,#30987,#30988,#30989,#30990,#30991,#30992,#30993,#30994,#30995,
#30996,#30997,#30998,#30999,#31000,#31001,#31002,#31003),.UNSPECIFIED.,
 .F.,.F.,(4,3,3,3,3,3,3,3,3,3,3,3,3,3,3,3,3,3,3,3,3,3,3,3,3,3,4),(21.9911485751286,
22.0812832713838,22.1714804226723,22.261826529727,22.3522487536846,22.4428476766967,
22.5237709676885,22.6118189900162,22.6997606457963,22.7876186028424,22.8758448432762,
22.9636123067326,23.0513688221931,23.1391347601272,23.2277082016737,23.3155978774572,
23.4045132018852,23.4934285263132,23.5837235555123,23.6716503950898,23.7595005030845,
23.8472943416567,23.939417946219,24.0271767650983,24.1149384979725,24.2027438832918,
24.2157887599059),.UNSPECIFIED.);
#1362=B_SPLINE_CURVE_WITH_KNOTS('',3,(#31005,#31006,#31007,#31008,#31009,
#31010,#31011,#31012,#31013,#31014,#31015,#31016,#31017,#31018,#31019,#31020,
#31021,#31022,#31023,#31024,#31025,#31026,#31027,#31028,#31029,#31030,#31031,
#31032,#31033,#31034,#31035,#31036,#31037,#31038,#31039,#31040,#31041,#31042,
#31043,#31044,#31045,#31046,#31047,#31048,#31049,#31050,#31051,#31052,#31053,
#31054,#31055,#31056,#31057,#31058,#31059,#31060,#31061,#31062,#31063,#31064,
#31065,#31066,#31067,#31068,#31069,#31070,#31071,#31072,#31073,#31074,#31075,
#31076,#31077,#31078,#31079,#31080,#31081,#31082,#31083),.UNSPECIFIED.,
 .F.,.F.,(4,3,3,3,3,3,3,3,3,3,3,3,3,3,3,3,3,3,3,3,3,3,3,3,3,3,4),(21.9911485751286,
22.1228635067403,22.1563861157154,22.2444349459262,22.3323774115027,22.4202361791641,
22.5084621160611,22.5962303865945,22.6839877062593,22.7717544445469,22.8603267519952,
22.9482172112254,23.0371304427827,23.1260436743401,23.2140922303503,23.302034432551,
23.3898929479589,23.4781189835846,23.5658870309858,23.6536441389621,23.7414106773092,
23.8299833162231,23.9178736064531,24.006787419709,24.0957012329649,24.1837486634078,
24.2167210304736),.UNSPECIFIED.);
#1363=B_SPLINE_CURVE_WITH_KNOTS('',3,(#31084,#31085,#31086,#31087,#31088,
#31089,#31090,#31091,#31092,#31093,#31094,#31095,#31096,#31097,#31098,#31099,
#31100,#31101,#31102,#31103,#31104,#31105,#31106,#31107,#31108,#31109,#31110,
#31111,#31112,#31113,#31114,#31115,#31116,#31117,#31118,#31119,#31120,#31121,
#31122,#31123,#31124,#31125,#31126,#31127,#31128,#31129,#31130,#31131,#31132,
#31133,#31134,#31135,#31136,#31137,#31138,#31139,#31140,#31141,#31142,#31143,
#31144,#31145,#31146,#31147,#31148,#31149,#31150,#31151,#31152,#31153,#31154,
#31155,#31156,#31157,#31158,#31159,#31160,#31161,#31162,#31163,#31164,#31165,
#31166,#31167,#31168,#31169,#31170,#31171,#31172,#31173,#31174,#31175,#31176,
#31177,#31178,#31179,#31180,#31181,#31182,#31183,#31184,#31185,#31186,#31187,
#31188,#31189,#31190,#31191,#31192,#31193,#31194,#31195,#31196,#31197,#31198,
#31199,#31200,#31201,#31202,#31203,#31204,#31205,#31206,#31207,#31208,#31209,
#31210,#31211,#31212,#31213,#31214,#31215,#31216,#31217,#31218,#31219,#31220,
#31221,#31222,#31223,#31224,#31225),.UNSPECIFIED.,.F.,.F.,(4,3,3,3,3,3,
3,3,3,3,3,3,3,3,3,3,3,3,3,3,3,3,3,3,3,3,3,3,3,3,3,3,3,3,3,3,3,3,3,3,3,3,
3,3,3,3,3,4),(17.9327347217548,18.0207028334297,18.1087133098411,18.1968591847413,
18.2777558812165,18.3657489057899,18.4536348542302,18.5414364722316,18.6296835931828,
18.7173935456239,18.8050922153734,18.8928000405043,18.9814533903386,19.0692848252938,
19.1583491325675,19.2474134398412,19.3354645118875,19.4234091759826,19.5112700952095,
19.5994952081166,19.687265495308,19.775024775687,19.8627934153293,19.9513628111135,
20.0392550032863,20.1281630008761,20.2170709984659,20.3051281041348,20.3930790264297,
20.4809464194359,20.5691691866428,20.6569464368303,20.7447128527237,20.8324887930608,
20.9210487340683,21.008948571148,21.0978385641194,21.1867285570907,21.273527087034,
21.3632297730275,21.4498281548608,21.5363771958627,21.6228985324255,21.7094137732703,
21.7959775267575,21.8825708026085,21.9692510829171,21.9911485749818),
 .UNSPECIFIED.);
#1364=B_SPLINE_CURVE_WITH_KNOTS('',3,(#31351,#31352,#31353,#31354,#31355,
#31356,#31357,#31358,#31359,#31360,#31361,#31362,#31363,#31364,#31365,#31366,
#31367,#31368,#31369,#31370,#31371,#31372,#31373,#31374,#31375,#31376,#31377,
#31378,#31379,#31380,#31381,#31382,#31383,#31384,#31385,#31386,#31387,#31388,
#31389,#31390,#31391,#31392,#31393,#31394,#31395,#31396,#31397,#31398,#31399,
#31400,#31401,#31402,#31403,#31404,#31405,#31406,#31407,#31408,#31409,#31410,
#31411,#31412,#31413,#31414,#31415,#31416,#31417,#31418,#31419,#31420,#31421,
#31422,#31423,#31424,#31425,#31426,#31427,#31428,#31429,#31430,#31431,#31432,
#31433,#31434,#31435,#31436,#31437,#31438,#31439,#31440,#31441,#31442,#31443,
#31444,#31445,#31446,#31447),.UNSPECIFIED.,.F.,.F.,(4,3,3,3,3,3,3,3,3,3,
3,3,3,3,3,3,3,3,3,3,3,3,3,3,3,3,3,3,3,3,3,3,4),(0.,0.0368147651103806,0.074501375546203,
0.112342565701432,0.146724444798353,0.154519180409614,0.159861819792071,
0.196798717360609,0.233592540188374,0.269524566381248,0.298932809818202,
0.306076330027527,0.311216260529057,0.347078994221376,0.382941727913695,
0.418902115841158,0.438585912474743,0.449351195385943,0.454626931743855,
0.489598596886897,0.524685601953606,0.559397454224109,0.58120313019341,
0.59285263403861,0.598656049365913,0.632452752519065,0.657800279883928,
0.670541577997107,0.677750468942682,0.683202198273149,0.715752223335255,
0.733842861978519,0.7607598169945),.UNSPECIFIED.);
#1365=B_SPLINE_CURVE_WITH_KNOTS('',3,(#31448,#31449,#31450,#31451,#31452,
#31453,#31454,#31455,#31456,#31457,#31458,#31459,#31460,#31461,#31462,#31463,
#31464,#31465,#31466,#31467,#31468,#31469,#31470,#31471,#31472,#31473,#31474,
#31475,#31476,#31477,#31478,#31479,#31480,#31481,#31482,#31483,#31484,#31485,
#31486,#31487,#31488,#31489,#31490,#31491,#31492,#31493,#31494,#31495,#31496,
#31497,#31498,#31499,#31500,#31501,#31502,#31503,#31504,#31505,#31506,#31507,
#31508,#31509,#31510,#31511,#31512,#31513,#31514,#31515,#31516,#31517,#31518,
#31519,#31520,#31521,#31522,#31523,#31524,#31525,#31526,#31527,#31528,#31529,
#31530,#31531,#31532,#31533,#31534,#31535,#31536,#31537,#31538,#31539,#31540,
#31541),.UNSPECIFIED.,.F.,.F.,(4,3,3,3,3,3,3,3,3,3,3,3,3,3,3,3,3,3,3,3,
3,3,3,3,3,3,3,3,3,3,3,4),(0.,0.0317286290156565,0.0642501424452636,0.0974595459930366,
0.128683472946203,0.13417368264342,0.138863677582811,0.172961043862833,
0.207570732336978,0.242490789657325,0.268680832647586,0.273374565791653,
0.278378882268977,0.314014888610594,0.347250961618367,0.381919138299765,
0.403413416033706,0.414921668851046,0.421531186875753,0.456779694785063,
0.493075652037049,0.529371609289035,0.553928605883257,0.562469494994855,
0.567815809877077,0.60521901315643,0.635283559248348,0.660319223571335,
0.666105225726651,0.703933093791132,0.725827582042816,0.757697664562209),
 .UNSPECIFIED.);
#1366=B_SPLINE_CURVE_WITH_KNOTS('',3,(#31542,#31543,#31544,#31545),
 .UNSPECIFIED.,.F.,.F.,(4,4),(-0.0141321293118755,0.),.UNSPECIFIED.);
#1367=B_SPLINE_CURVE_WITH_KNOTS('',3,(#31670,#31671,#31672,#31673,#31674,
#31675,#31676,#31677,#31678,#31679,#31680,#31681,#31682,#31683,#31684,#31685,
#31686,#31687,#31688,#31689,#31690,#31691,#31692,#31693,#31694,#31695,#31696,
#31697,#31698,#31699,#31700,#31701,#31702,#31703,#31704,#31705,#31706,#31707,
#31708,#31709,#31710,#31711,#31712,#31713,#31714,#31715,#31716,#31717,#31718,
#31719,#31720,#31721,#31722,#31723,#31724,#31725,#31726,#31727,#31728,#31729,
#31730,#31731,#31732,#31733,#31734,#31735,#31736,#31737,#31738,#31739,#31740,
#31741,#31742,#31743,#31744,#31745,#31746,#31747,#31748,#31749,#31750,#31751,
#31752,#31753,#31754,#31755,#31756,#31757,#31758,#31759,#31760,#31761,#31762,
#31763),.UNSPECIFIED.,.F.,.F.,(4,3,3,3,3,3,3,3,3,3,3,3,3,3,3,3,3,3,3,3,
3,3,3,3,3,3,3,3,3,3,3,4),(0.,0.0321250758863861,0.0642501517727722,0.0977017688573295,
0.128683484204146,0.134173763202423,0.13886369439468,0.172961064488349,
0.207570755159294,0.242490806774014,0.268680845485055,0.273374584290101,
0.278378886542516,0.314014893103864,0.347250961618176,0.381919136552636,
0.403413414395757,0.414921666320687,0.421531186815446,0.456944022746122,
0.492989037452285,0.529588353331513,0.553928602645526,0.562469488501506,
0.567815809339951,0.605219012373712,0.63528355843125,0.660319221884543,
0.666105223775399,0.703933092116297,0.725827582042572,0.757697666925817),
 .UNSPECIFIED.);
#1368=B_SPLINE_CURVE_WITH_KNOTS('',3,(#31764,#31765,#31766,#31767,#31768,
#31769,#31770,#31771,#31772,#31773,#31774,#31775,#31776,#31777,#31778,#31779,
#31780,#31781,#31782,#31783,#31784,#31785,#31786,#31787,#31788,#31789,#31790,
#31791,#31792,#31793,#31794,#31795,#31796,#31797,#31798,#31799,#31800,#31801,
#31802,#31803,#31804,#31805,#31806,#31807,#31808,#31809,#31810,#31811,#31812,
#31813,#31814,#31815,#31816,#31817,#31818,#31819,#31820,#31821,#31822,#31823,
#31824,#31825,#31826,#31827,#31828,#31829,#31830,#31831,#31832,#31833,#31834,
#31835,#31836,#31837,#31838,#31839,#31840,#31841,#31842,#31843,#31844,#31845,
#31846,#31847,#31848,#31849,#31850,#31851,#31852,#31853,#31854,#31855,#31856,
#31857,#31858,#31859,#31860),.UNSPECIFIED.,.F.,.F.,(4,3,3,3,3,3,3,3,3,3,
3,3,3,3,3,3,3,3,3,3,3,3,3,3,3,3,3,3,3,3,3,3,4),(0.,0.0371460267140582,0.0748361240619943,
0.112676081007043,0.146724449836877,0.15451918997546,0.159861821081083,
0.19680457436756,0.233592541347715,0.269524566606476,0.298932810470348,
0.306076332066899,0.311216261220193,0.347078994566964,0.382941727913735,
0.418902116039512,0.438585912660715,0.449351195759605,0.454626932097783,
0.489598597399228,0.524659768090933,0.559397455171815,0.581203131022683,
0.592852635112903,0.598656049141822,0.632468594886279,0.657800279757981,
0.67054157736057,0.677750458032431,0.683202182754059,0.715752207345716,
0.733842861978756,0.760759816994732),.UNSPECIFIED.);
#1369=B_SPLINE_CURVE_WITH_KNOTS('',3,(#31905,#31906,#31907,#31908,#31909,
#31910,#31911,#31912,#31913,#31914,#31915,#31916,#31917,#31918,#31919,#31920,
#31921,#31922,#31923,#31924,#31925,#31926,#31927,#31928,#31929,#31930,#31931,
#31932,#31933,#31934,#31935,#31936,#31937,#31938,#31939,#31940,#31941,#31942,
#31943,#31944,#31945,#31946,#31947,#31948,#31949,#31950,#31951,#31952,#31953,
#31954,#31955,#31956,#31957,#31958,#31959,#31960,#31961,#31962,#31963,#31964,
#31965,#31966,#31967,#31968,#31969,#31970,#31971,#31972,#31973,#31974,#31975,
#31976,#31977,#31978,#31979,#31980,#31981,#31982,#31983,#31984,#31985,#31986,
#31987,#31988,#31989,#31990,#31991,#31992,#31993,#31994,#31995,#31996,#31997,
#31998,#31999,#32000,#32001,#32002,#32003,#32004,#32005,#32006,#32007,#32008,
#32009,#32010,#32011,#32012,#32013),.UNSPECIFIED.,.F.,.F.,(4,3,3,3,3,3,
3,3,3,3,3,3,3,3,3,3,3,3,3,3,3,3,3,3,3,3,3,3,3,3,3,3,3,3,3,3,4),(10.3763408596307,
10.4685035879595,10.5605450798931,10.6540126042865,10.7459016202891,10.8377629934542,
10.9296224595031,11.0242881633874,11.1162731126776,11.2122791938588,11.3082852750401,
11.4015231451061,11.4946379598422,11.5876571073663,11.6806117932315,11.7735333702322,
11.8664464519442,11.9593756382665,12.0524050043333,12.1454872708207,12.2387236347795,
12.3061361167675,12.3991530832475,12.4920433843522,12.5848347338002,12.6775576307686,
12.7702450445746,12.8629218677855,12.9556129776305,13.0484029190153,13.1412446433811,
13.2342411237987,13.3039869584949,13.3970673240037,13.4900377484096,13.5829076752469,
13.662003513089),.UNSPECIFIED.);
#1370=B_SPLINE_CURVE_WITH_KNOTS('',3,(#32016,#32017,#32018,#32019,#32020,
#32021,#32022,#32023,#32024,#32025,#32026,#32027,#32028,#32029,#32030,#32031,
#32032,#32033,#32034,#32035,#32036,#32037,#32038,#32039,#32040,#32041,#32042,
#32043,#32044,#32045,#32046,#32047,#32048,#32049,#32050,#32051,#32052,#32053,
#32054,#32055,#32056,#32057,#32058,#32059,#32060,#32061,#32062,#32063,#32064,
#32065,#32066,#32067,#32068,#32069,#32070,#32071,#32072,#32073,#32074,#32075,
#32076,#32077,#32078,#32079,#32080,#32081,#32082,#32083,#32084,#32085,#32086,
#32087,#32088,#32089,#32090,#32091),.UNSPECIFIED.,.F.,.F.,(4,2,2,2,2,2,
2,2,2,2,2,2,2,2,2,2,2,2,2,2,2,2,2,2,2,2,2,2,2,2,2,2,2,2,2,2,2,4),(-3.35381526931575,
-3.35208315295462,-3.34983146774722,-3.34483876368488,-3.32619197630295,
-3.27122359195305,-3.22306543606155,-3.21388437505902,-3.20858010275596,
-3.20392890877022,-3.19813032562173,-3.18910420019164,-3.13190644661067,
-3.085595133377,-3.0428844389819,-3.03704710102653,-3.03458254610874,-3.03213833675085,
-3.02994487981598,-3.02689266704973,-3.01892914498056,-2.97007407985262,
-2.8972840853171,-2.88320402228536,-2.87743187246694,-2.87328482018027,
-2.86951031673175,-2.86444987637415,-2.85214471248006,-2.77985001500164,
-2.72230605211448,-2.71296395890366,-2.70954291846262,-2.70717462614405,
-2.70497732276349,-2.70196675866152,-2.69435955099127,-2.69261509225713),
 .UNSPECIFIED.);
#1371=B_SPLINE_CURVE_WITH_KNOTS('',3,(#32097,#32098,#32099,#32100,#32101,
#32102,#32103,#32104,#32105,#32106,#32107,#32108,#32109,#32110,#32111,#32112,
#32113,#32114,#32115,#32116,#32117,#32118,#32119,#32120,#32121,#32122,#32123,
#32124,#32125,#32126,#32127,#32128,#32129,#32130,#32131,#32132,#32133,#32134,
#32135,#32136,#32137,#32138,#32139,#32140,#32141,#32142,#32143,#32144,#32145,
#32146,#32147,#32148,#32149,#32150,#32151,#32152,#32153,#32154,#32155,#32156,
#32157,#32158,#32159,#32160,#32161,#32162,#32163,#32164,#32165,#32166,#32167,
#32168,#32169,#32170,#32171,#32172,#32173,#32174,#32175,#32176,#32177,#32178,
#32179,#32180,#32181,#32182,#32183,#32184,#32185,#32186,#32187,#32188,#32189,
#32190,#32191,#32192,#32193,#32194,#32195,#32196,#32197,#32198,#32199,#32200,
#32201,#32202,#32203,#32204,#32205,#32206,#32207,#32208,#32209,#32210,#32211,
#32212,#32213,#32214,#32215,#32216,#32217,#32218,#32219,#32220,#32221,#32222,
#32223,#32224,#32225,#32226,#32227,#32228,#32229,#32230,#32231,#32232,#32233,
#32234,#32235,#32236,#32237,#32238,#32239,#32240,#32241,#32242,#32243,#32244,
#32245,#32246,#32247,#32248,#32249,#32250),.UNSPECIFIED.,.F.,.F.,(4,2,2,
2,2,2,2,2,2,2,2,2,2,2,2,2,2,2,2,2,2,2,2,2,2,2,2,2,2,2,2,2,2,2,2,2,2,2,2,
2,2,2,2,2,2,2,2,2,2,2,2,2,2,2,2,2,2,2,2,2,2,2,2,2,2,2,2,2,2,2,2,2,2,2,2,
2,4),(-1.37017729781545,-1.35353780576373,-1.33257834742348,-1.32548122187877,
-1.32094726490235,-1.31668689964161,-1.31096736598667,-1.29797497597591,
-1.28014171544337,-1.22883793443645,-1.17254957458835,-1.16452266794228,
-1.16142937281249,-1.15920630467273,-1.15677107461307,-1.15323034881184,
-1.14384503173126,-1.12960173098574,-1.07886840906787,-1.01403121697174,
-1.00580271677102,-1.00054113135373,-0.996340483931179,-0.991578637763216,
-0.983437132773718,-0.94758375686734,-0.900429253094662,-0.850308959919973,
-0.842205213330912,-0.839101245359232,-0.836875455818964,-0.834442726563618,
-0.830915196301282,-0.821620279122071,-0.807562779774907,-0.707110833613374,
-0.687412651737281,-0.680481782934284,-0.675983987862879,-0.671707272617472,
-0.665887232896476,-0.652307404813528,-0.63340940348293,-0.52946292793793,
-0.520056255652633,-0.516402835476207,-0.514188674404075,-0.511743014886738,
-0.508153924649882,-0.498442083047438,-0.437387510478215,-0.374545774329483,
-0.36194259260325,-0.356351857845128,-0.352095452245071,-0.351582388850521,
-0.346996720500453,-0.339433075634769,-0.330361169326727,-0.31215093911564,
-0.258879006166635,-0.205305953728267,-0.197214129082237,-0.194111637054782,
-0.191885985176512,-0.189453999882711,-0.185926160343614,-0.176621297251876,
-0.162541792995744,-0.0693764045847394,-0.0438024477556163,-0.0361792526774839,
-0.0315321654369022,-0.0274544150076456,-0.0233724540897795,-0.0181340863993818,
-0.000954368308936828),.UNSPECIFIED.);
#1372=B_SPLINE_CURVE_WITH_KNOTS('',3,(#32251,#32252,#32253,#32254,#32255,
#32256,#32257,#32258,#32259,#32260,#32261,#32262,#32263,#32264,#32265,#32266,
#32267,#32268,#32269,#32270,#32271,#32272,#32273,#32274,#32275,#32276,#32277,
#32278,#32279,#32280,#32281,#32282,#32283,#32284,#32285,#32286,#32287,#32288,
#32289,#32290,#32291,#32292,#32293,#32294,#32295,#32296,#32297,#32298,#32299,
#32300,#32301,#32302,#32303,#32304,#32305,#32306,#32307,#32308,#32309,#32310,
#32311,#32312,#32313,#32314,#32315,#32316,#32317),.UNSPECIFIED.,.F.,.F.,
(4,3,3,3,3,3,3,3,3,3,3,3,3,3,3,3,3,3,3,3,3,3,4),(13.662003513089,13.7547833390107,
13.8475493001619,13.9403261705392,14.0331997127964,14.1261218245434,14.2192021029353,
14.3018378002224,14.3949470159261,14.4879308398322,14.5808168538984,14.6736357436152,
14.7664199360917,14.8591942106715,14.9519833318896,15.0448715509177,15.1378118541448,
15.2309063867031,15.2996886419498,15.4024334558436,15.5048979103914,15.6068616102991,
15.7079632677851),.UNSPECIFIED.);
#1373=B_SPLINE_CURVE_WITH_KNOTS('',3,(#32318,#32319,#32320,#32321,#32322,
#32323,#32324,#32325,#32326,#32327,#32328,#32329,#32330,#32331,#32332,#32333,
#32334,#32335,#32336,#32337,#32338,#32339,#32340,#32341,#32342,#32343,#32344,
#32345,#32346,#32347,#32348,#32349,#32350,#32351,#32352,#32353,#32354,#32355,
#32356,#32357,#32358,#32359,#32360,#32361,#32362,#32363,#32364,#32365,#32366,
#32367,#32368,#32369,#32370,#32371,#32372,#32373,#32374,#32375,#32376,#32377,
#32378,#32379,#32380,#32381,#32382,#32383,#32384,#32385,#32386,#32387,#32388,
#32389,#32390,#32391,#32392,#32393,#32394,#32395,#32396,#32397,#32398,#32399,
#32400,#32401,#32402,#32403,#32404,#32405,#32406,#32407,#32408,#32409,#32410,
#32411,#32412,#32413,#32414,#32415,#32416,#32417,#32418,#32419,#32420,#32421,
#32422,#32423,#32424,#32425,#32426,#32427,#32428,#32429,#32430,#32431,#32432,
#32433,#32434,#32435,#32436,#32437,#32438,#32439,#32440,#32441,#32442,#32443,
#32444,#32445,#32446,#32447,#32448,#32449,#32450,#32451,#32452,#32453,#32454,
#32455,#32456,#32457,#32458,#32459,#32460,#32461,#32462,#32463,#32464,#32465,
#32466,#32467,#32468,#32469,#32470,#32471,#32472,#32473,#32474,#32475,#32476,
#32477,#32478,#32479,#32480,#32481,#32482,#32483,#32484,#32485,#32486,#32487,
#32488,#32489,#32490,#32491,#32492,#32493,#32494,#32495,#32496,#32497,#32498,
#32499,#32500,#32501,#32502,#32503,#32504,#32505,#32506,#32507,#32508,#32509,
#32510,#32511,#32512,#32513,#32514,#32515,#32516,#32517,#32518,#32519,#32520,
#32521,#32522,#32523),.UNSPECIFIED.,.F.,.F.,(4,2,2,2,2,2,2,2,2,2,2,2,2,
2,2,2,2,2,2,2,2,2,2,2,2,2,2,2,2,2,2,2,2,2,2,2,2,2,2,2,2,2,2,2,2,2,2,2,2,
2,2,2,2,2,2,2,2,2,2,2,2,2,2,2,2,2,2,2,2,2,2,2,2,2,2,2,2,2,2,2,2,2,2,2,2,
2,2,2,2,2,2,2,2,2,2,2,2,2,2,2,2,2,4),(-2.69261509225713,-2.62840556418915,
-2.58320465660134,-2.5581209019691,-2.55077455147651,-2.54615710481637,
-2.54186963989729,-2.53628654202243,-2.52389960895418,-2.45910092414662,
-2.4210319306056,-2.40355810669151,-2.39304293511801,-2.38930168080884,
-2.38679274096041,-2.3845680187088,-2.38153097868239,-2.37396463106057,
-2.30781275498151,-2.26343067004595,-2.2387077651925,-2.23141206564109,
-2.22681501059143,-2.2225389684779,-2.21696070820388,-2.2045480219227,-2.13407070170969,
-2.09168152552772,-2.07873550345086,-2.06998367493561,-2.06652831838317,
-2.06410214583396,-2.06154906462413,-2.05743810090315,-2.04471366480278,
-1.98789225372189,-1.94149850550134,-1.92468076243408,-1.91226986600097,
-1.9066669592139,-1.90243878318937,-1.89788730673565,-1.89065283231372,
-1.86838897281277,-1.77038951237406,-1.75641322232236,-1.74716598949256,
-1.7436560940739,-1.74123374683306,-1.73900610856686,-1.73590083064744,
-1.72778977032303,-1.67764324502658,-1.60086409733971,-1.58888035541318,
-1.58339341499287,-1.57914615353389,-1.57453929754588,-1.56713943598796,
-1.54113295901057,-1.49279730227811,-1.4325400897938,-1.42466346939064,
-1.4215877574702,-1.41936452244751,-1.41691652161779,-1.41333076945456,
-1.40366591344044,-1.34341237495997,-1.27959500561132,-1.2682908828538,
-1.26214778234246,-1.25785023721058,-1.25344256823369,-1.24696345539816,
-1.22907832395468,-1.20167432452606,-1.14575664002757,-1.10638950402625,
-1.1013280534111,-1.09828618603912,-1.0959209094728,-1.09319654623698,-1.08833367065206,
-1.06433817920143,-0.998898346786502,-0.95149052745457,-0.943379214362556,
-0.938151699456961,-0.93395191356894,-0.929162535952773,-0.920901870025552,
-0.883096196407596,-0.838553402197201,-0.787896978384544,-0.779795442219594,
-0.776690718998467,-0.77446410452002,-0.77202874119717,-0.768496558743206,
-0.759185453215502,-0.745099087974622,-0.662096941273505),.UNSPECIFIED.);
#1374=B_SPLINE_CURVE_WITH_KNOTS('',3,(#32528,#32529,#32530,#32531,#32532,
#32533,#32534,#32535,#32536,#32537,#32538,#32539,#32540,#32541,#32542,#32543,
#32544,#32545,#32546,#32547,#32548,#32549,#32550,#32551,#32552,#32553,#32554,
#32555,#32556,#32557,#32558,#32559,#32560,#32561,#32562,#32563,#32564,#32565,
#32566,#32567,#32568,#32569,#32570,#32571,#32572,#32573,#32574,#32575,#32576,
#32577,#32578,#32579,#32580,#32581,#32582,#32583,#32584,#32585,#32586,#32587,
#32588,#32589,#32590,#32591,#32592,#32593,#32594,#32595,#32596,#32597,#32598,
#32599,#32600,#32601,#32602,#32603,#32604,#32605,#32606,#32607,#32608,#32609,
#32610,#32611,#32612,#32613,#32614,#32615,#32616,#32617,#32618,#32619,#32620,
#32621,#32622,#32623,#32624,#32625,#32626,#32627,#32628,#32629,#32630,#32631,
#32632,#32633,#32634,#32635,#32636,#32637,#32638,#32639,#32640,#32641,#32642,
#32643,#32644,#32645,#32646,#32647,#32648,#32649,#32650,#32651,#32652,#32653,
#32654,#32655,#32656,#32657,#32658,#32659,#32660,#32661,#32662,#32663,#32664,
#32665,#32666,#32667,#32668,#32669,#32670,#32671,#32672,#32673,#32674,#32675,
#32676,#32677,#32678,#32679,#32680,#32681,#32682,#32683,#32684,#32685,#32686,
#32687,#32688,#32689,#32690,#32691,#32692,#32693,#32694,#32695,#32696,#32697,
#32698,#32699,#32700,#32701,#32702,#32703,#32704,#32705,#32706,#32707,#32708,
#32709,#32710,#32711,#32712,#32713,#32714,#32715,#32716,#32717,#32718,#32719,
#32720,#32721,#32722,#32723,#32724,#32725,#32726,#32727,#32728,#32729,#32730,
#32731,#32732,#32733,#32734,#32735,#32736,#32737,#32738,#32739,#32740,#32741,
#32742,#32743),.UNSPECIFIED.,.F.,.F.,(4,2,2,2,2,2,2,2,2,2,2,2,2,2,2,2,2,
2,2,2,2,2,2,2,2,2,2,2,2,2,2,2,2,2,2,2,2,2,2,2,2,2,2,2,2,2,2,2,2,2,2,2,2,
2,2,2,2,2,2,2,2,2,2,2,2,2,2,2,2,2,2,2,2,2,2,2,2,2,2,2,2,2,2,2,2,2,2,2,2,
2,2,2,2,2,2,2,2,2,2,2,2,2,2,2,2,2,2,4),(-3.40019978283383,-3.33785962504013,
-3.27156335607859,-3.26196291641992,-3.25689126660038,-3.25274339360484,
-3.24785601059373,-3.23936276391376,-3.20122700787053,-3.13428425247534,
-3.11273789666227,-3.10425562390685,-3.09792357910148,-3.09489880588864,
-3.0925428382484,-3.08977834312619,-3.08485968336625,-3.06265332848916,
-3.05368678966229,-2.97168692317334,-2.95423949296249,-2.94146336005877,
-2.93578327087505,-2.93153065855957,-2.92753524058326,-2.92087524358251,
-2.90309438654935,-2.80027475110723,-2.78612759229225,-2.77679034859233,
-2.77325708904298,-2.77082366780496,-2.7685997250947,-2.76550173993936,
-2.75743816373339,-2.70348014953057,-2.69708672421599,-2.64887963959844,
-2.6316680928851,-2.61902423762827,-2.61336685598548,-2.60911709669841,
-2.60511402393393,-2.59841657818522,-2.58038378126111,-2.47785358116976,
-2.46371480757022,-2.45438115837674,-2.4508479951634,-2.44841424146137,
-2.44618967052223,-2.44309039405311,-2.43502044916619,-2.38084305956231,
-2.32807198872925,-2.30995858474924,-2.29680936902852,-2.29106277359642,
-2.28679816252814,-2.28227446379223,-2.2752241378696,-2.25460537193083,
-2.15520087420387,-2.14118020174492,-2.13190379206863,-2.12837873404686,
-2.12594627243598,-2.12371947728022,-2.12061261366701,-2.11248935071206,
-2.0628865616765,-2.05184291245054,-2.03165746075049,-1.98115202486522,
-1.97295607823159,-1.96770379425843,-1.96350320435912,-1.95873350139782,
-1.95055869366086,-1.91417959380968,-1.86556923818777,-1.84083175773657,
-1.81296855049339,-1.8081940458159,-1.80520683283672,-1.80285246102468,
-1.80005713013371,-1.79486026441714,-1.76326575464596,-1.69715013019003,
-1.65800113698883,-1.64945192898591,-1.64455037798679,-1.64040093780557,
-1.63534023612804,-1.62580017436166,-1.61380059407552,-1.58648490115453,
-1.54466786480509,-1.49516457585576,-1.48703173834883,-1.48392355454095,
-1.48169642532567,-1.47926424364828,-1.4757407321054,-1.46647480103462,
-1.45247710770272,-1.37017729781545),.UNSPECIFIED.);
#1375=B_SPLINE_CURVE_WITH_KNOTS('',3,(#32745,#32746,#32747,#32748,#32749,
#32750,#32751,#32752,#32753,#32754,#32755,#32756,#32757,#32758,#32759,#32760,
#32761,#32762,#32763,#32764,#32765,#32766,#32767,#32768,#32769,#32770,#32771,
#32772,#32773,#32774,#32775,#32776,#32777,#32778,#32779,#32780,#32781,#32782,
#32783,#32784,#32785,#32786,#32787,#32788,#32789,#32790,#32791,#32792,#32793,
#32794,#32795,#32796,#32797,#32798,#32799,#32800,#32801,#32802,#32803,#32804,
#32805,#32806,#32807,#32808,#32809,#32810,#32811,#32812,#32813,#32814,#32815,
#32816,#32817,#32818,#32819,#32820,#32821,#32822,#32823,#32824,#32825,#32826,
#32827,#32828,#32829,#32830,#32831,#32832,#32833,#32834,#32835,#32836,#32837,
#32838),.UNSPECIFIED.,.F.,.F.,(4,2,2,2,2,2,2,2,2,2,2,2,2,2,2,2,2,2,2,2,
2,2,2,2,2,2,2,2,2,2,2,2,2,2,2,2,2,2,2,2,2,2,2,2,2,2,4),(-0.662096941273505,
-0.644012719739959,-0.624813906700673,-0.617946465357201,-0.61345872401671,
-0.609168813828691,-0.603294615271159,-0.589416215840541,-0.569974529301255,
-0.512373160929998,-0.488520616481295,-0.460872434565717,-0.456103611975906,
-0.453116473389265,-0.450759955505912,-0.447959352362998,-0.442744501743739,
-0.410724261387381,-0.342088399887239,-0.305684066271292,-0.297260779481479,
-0.29238538676688,-0.288365535647978,-0.288284500126682,-0.288213905080228,
-0.288152183486406,-0.288098050919491,-0.288050444656379,-0.287954023183898,
-0.287859928484098,-0.287767993288569,-0.287678062119022,-0.287589990493134,
-0.28267224182747,-0.277034907874753,-0.267897316736875,-0.24950233237944,
-0.195245063880915,-0.143014950278401,-0.134905540056361,-0.131798965530057,
-0.12957116488514,-0.127136232799798,-0.1236049776553,-0.114296766641828,
-0.100215253267655,-0.000985697035008145),.UNSPECIFIED.);
#1376=B_SPLINE_CURVE_WITH_KNOTS('',3,(#32839,#32840,#32841,#32842,#32843,
#32844,#32845,#32846,#32847,#32848,#32849,#32850,#32851,#32852,#32853,#32854,
#32855,#32856,#32857,#32858,#32859,#32860,#32861,#32862,#32863,#32864,#32865,
#32866,#32867,#32868,#32869,#32870,#32871,#32872,#32873,#32874,#32875,#32876,
#32877,#32878,#32879,#32880,#32881,#32882,#32883,#32884,#32885,#32886,#32887,
#32888,#32889,#32890,#32891,#32892,#32893,#32894,#32895,#32896,#32897,#32898,
#32899,#32900,#32901,#32902,#32903,#32904,#32905,#32906,#32907,#32908,#32909,
#32910,#32911,#32912,#32913,#32914,#32915,#32916,#32917,#32918,#32919,#32920,
#32921,#32922,#32923,#32924,#32925,#32926,#32927,#32928,#32929,#32930,#32931,
#32932,#32933,#32934,#32935,#32936,#32937,#32938,#32939,#32940,#32941,#32942,
#32943,#32944,#32945,#32946,#32947,#32948,#32949,#32950,#32951,#32952,#32953,
#32954,#32955,#32956,#32957,#32958,#32959,#32960,#32961,#32962,#32963,#32964,
#32965,#32966,#32967,#32968,#32969,#32970,#32971,#32972,#32973,#32974,#32975,
#32976,#32977,#32978,#32979,#32980,#32981,#32982,#32983,#32984,#32985,#32986,
#32987,#32988,#32989,#32990,#32991,#32992),.UNSPECIFIED.,.F.,.F.,(4,2,2,
2,2,2,2,2,2,2,2,2,2,2,2,2,2,2,2,2,2,2,2,2,2,2,2,2,2,2,2,2,2,2,2,2,2,2,2,
2,2,2,2,2,2,2,2,2,2,2,2,2,2,2,2,2,2,2,2,2,2,2,2,2,2,2,2,2,2,2,2,2,2,2,2,
2,4),(-4.06157145021908,-4.04807440817928,-4.03856467987825,-4.03393873005346,
-4.03000157592306,-4.02604097088093,-4.02081706246017,-4.0127177091575,
-3.98635579660403,-3.93397204242227,-3.87725700878007,-3.87157254187659,
-3.86867490169071,-3.86655357980012,-3.86378019163222,-3.85882924332806,
-3.83611505747223,-3.82812448825048,-3.74575260748455,-3.72826727557778,
-3.71944848640976,-3.71205572037451,-3.70862621689302,-3.70451682093695,
-3.6996433166824,-3.69122350406628,-3.65476818366308,-3.58656708036991,
-3.5646363935611,-3.55186345142934,-3.54788547798063,-3.54535623137956,
-3.54294778829835,-3.53942598139824,-3.53082103944866,-3.43334018119189,
-3.39825062761908,-3.39015482394934,-3.38540143114383,-3.38119710041741,
-3.37591602986257,-3.36762759654677,-3.3100044839404,-3.25400106117824,
-3.23104430626754,-3.22624029043099,-3.22352897176375,-3.22116286531749,
-3.21810376350195,-3.21142587089775,-3.20983109897739,-3.14421900669202,
-3.09930666832812,-3.08279270303488,-3.07054387065534,-3.06495503698883,
-3.06071316305695,-3.05668515368407,-3.04986715839868,-3.03100524868918,
-2.92951427869627,-2.91541286568839,-2.90609619336183,-2.90256407293655,
-2.90012931035266,-2.89790234827737,-2.89479773397084,-2.88669902542398,
-2.83637454939601,-2.7894259719955,-2.75364633096651,-2.74550579395821,
-2.7407419736787,-2.73653799902376,-2.73127009425987,-2.72302728728776,
-2.69274389685463),.UNSPECIFIED.);
#1377=B_SPLINE_CURVE_WITH_KNOTS('',3,(#32998,#32999,#33000,#33001,#33002,
#33003,#33004,#33005,#33006,#33007,#33008,#33009,#33010,#33011,#33012,#33013,
#33014,#33015,#33016,#33017,#33018,#33019,#33020,#33021,#33022,#33023,#33024,
#33025,#33026,#33027,#33028,#33029,#33030,#33031,#33032,#33033,#33034,#33035,
#33036,#33037,#33038,#33039,#33040,#33041,#33042,#33043,#33044,#33045,#33046,
#33047,#33048,#33049,#33050,#33051,#33052,#33053,#33054,#33055,#33056,#33057,
#33058,#33059,#33060,#33061,#33062,#33063,#33064,#33065,#33066,#33067,#33068,
#33069,#33070,#33071,#33072,#33073,#33074,#33075,#33076,#33077,#33078,#33079,
#33080,#33081,#33082,#33083,#33084,#33085,#33086,#33087,#33088,#33089,#33090,
#33091,#33092,#33093,#33094,#33095,#33096,#33097,#33098,#33099,#33100,#33101,
#33102,#33103,#33104,#33105,#33106,#33107,#33108,#33109,#33110,#33111,#33112,
#33113,#33114,#33115,#33116,#33117,#33118,#33119,#33120,#33121,#33122,#33123,
#33124,#33125,#33126,#33127,#33128,#33129,#33130,#33131,#33132,#33133,#33134,
#33135,#33136,#33137,#33138,#33139,#33140,#33141,#33142,#33143,#33144,#33145,
#33146,#33147,#33148,#33149),.UNSPECIFIED.,.F.,.F.,(4,2,2,2,2,2,2,2,2,2,
2,2,2,2,2,2,2,2,2,2,2,2,2,2,2,2,2,2,2,2,2,2,2,2,2,2,2,2,2,2,2,2,2,2,2,2,
2,2,2,2,2,2,2,2,2,2,2,2,2,2,2,2,2,2,2,2,2,2,2,2,2,2,2,2,2,4),(-1.36994781431221,
-1.35403913083624,-1.30344451495222,-1.29534465922271,-1.29224063884764,
-1.29001441570313,-1.28758086695492,-1.284051378108,-1.27474675702159,-1.26067054126231,
-1.15978907963419,-1.14042544509649,-1.13353898820462,-1.12905010352677,
-1.12476737954213,-1.11891624827375,-1.10515593004192,-1.08592797343983,
-1.0295047467755,-1.00849221602317,-0.995577372928076,-0.975607063867324,
-0.970839979704906,-0.968109192655276,-0.965984214333597,-0.963035164179288,
-0.957092937533464,-0.900753006527331,-0.871047715508243,-0.822183027676799,
-0.814028034181265,-0.808788214836695,-0.804588745105528,-0.799810765179259,
-0.79159769912195,-0.754575788575409,-0.709524470366712,-0.658574742817765,
-0.650476594600359,-0.647373049335334,-0.645147122086622,-0.642713844579556,
-0.639184662296964,-0.629880349919068,-0.615804162916471,-0.51489121218588,
-0.495565690712209,-0.48868503262247,-0.484197755986418,-0.479914982646323,
-0.474061270508087,-0.460282955098616,-0.441021101492656,-0.384405622040821,
-0.336076920641187,-0.327990508575039,-0.324613060896587,-0.322232382556755,
-0.320035548214643,-0.317527490258593,-0.310319907611356,-0.27831689190842,
-0.203602816193235,-0.175281078771535,-0.167359374787102,-0.162645440414172,
-0.158858100496402,-0.153726603826024,-0.143840700829879,-0.131287186479607,
-0.102074471247827,-0.0455501577320752,-0.0103273183728019,-0.00448290106007735,
-0.00200870709752073,-0.000951636744030443),.UNSPECIFIED.);
#1378=B_SPLINE_CURVE_WITH_KNOTS('',3,(#33150,#33151,#33152,#33153,#33154,
#33155,#33156,#33157,#33158,#33159,#33160,#33161,#33162,#33163,#33164,#33165,
#33166,#33167,#33168,#33169,#33170,#33171,#33172,#33173,#33174,#33175,#33176,
#33177,#33178,#33179,#33180,#33181,#33182,#33183,#33184,#33185,#33186,#33187,
#33188,#33189,#33190,#33191,#33192,#33193,#33194,#33195,#33196,#33197,#33198,
#33199,#33200,#33201,#33202,#33203,#33204,#33205,#33206,#33207,#33208,#33209,
#33210,#33211,#33212,#33213,#33214,#33215,#33216,#33217,#33218,#33219,#33220,
#33221,#33222,#33223,#33224,#33225,#33226,#33227,#33228,#33229,#33230,#33231),
 .UNSPECIFIED.,.F.,.F.,(4,2,2,2,2,2,2,2,2,2,2,2,2,2,2,2,2,2,2,2,2,2,2,2,
2,2,2,2,2,2,2,2,2,2,2,2,2,2,2,2,4),(-4.06098341928092,-4.06080310437317,
-4.05935516277898,-4.05671553698414,-4.05219170774946,-4.03466221784105,
-4.02168389330639,-3.95943259813033,-3.9294978819508,-3.91673927325081,
-3.90672647937867,-3.90157048021314,-3.89737939171005,-3.89254604393623,
-3.88428972131288,-3.84994246621341,-3.78067236244368,-3.74986832349323,
-3.74279775147556,-3.74030418116452,-3.73810805690436,-3.73577611157493,
-3.73239875285325,-3.7243079361267,-3.67421012083181,-3.62711858962269,
-3.59129729265715,-3.5831601040997,-3.57840024782517,-3.57420102377141,
-3.56894077754901,-3.56071341638611,-3.4967801651768,-3.43164404785125,
-3.42167540578113,-3.41805158700942,-3.41560011089201,-3.4133942115017,
-3.41036560161198,-3.40273282390601,-3.40019978283383),.UNSPECIFIED.);
#1379=B_SPLINE_CURVE_WITH_KNOTS('',3,(#33232,#33233,#33234,#33235,#33236,
#33237,#33238,#33239,#33240,#33241,#33242,#33243,#33244,#33245,#33246,#33247,
#33248,#33249,#33250,#33251,#33252,#33253,#33254,#33255,#33256,#33257,#33258,
#33259,#33260,#33261,#33262,#33263,#33264,#33265,#33266,#33267,#33268,#33269,
#33270,#33271,#33272,#33273,#33274,#33275,#33276,#33277,#33278,#33279,#33280,
#33281,#33282,#33283,#33284,#33285,#33286,#33287,#33288,#33289,#33290,#33291,
#33292,#33293,#33294,#33295,#33296,#33297,#33298,#33299,#33300,#33301,#33302,
#33303,#33304,#33305,#33306,#33307,#33308,#33309,#33310,#33311,#33312,#33313,
#33314,#33315,#33316,#33317,#33318,#33319,#33320,#33321,#33322,#33323,#33324,
#33325,#33326,#33327,#33328,#33329,#33330,#33331,#33332,#33333,#33334,#33335,
#33336,#33337,#33338,#33339,#33340,#33341,#33342,#33343,#33344,#33345,#33346,
#33347,#33348,#33349,#33350,#33351,#33352,#33353,#33354,#33355,#33356,#33357,
#33358,#33359,#33360,#33361,#33362,#33363,#33364,#33365,#33366,#33367,#33368,
#33369,#33370,#33371,#33372,#33373,#33374,#33375,#33376,#33377,#33378,#33379,
#33380,#33381,#33382,#33383,#33384,#33385,#33386,#33387,#33388,#33389,#33390,
#33391,#33392,#33393,#33394,#33395,#33396,#33397,#33398,#33399,#33400,#33401,
#33402,#33403,#33404,#33405,#33406,#33407,#33408,#33409,#33410,#33411,#33412,
#33413,#33414,#33415,#33416,#33417,#33418,#33419,#33420,#33421,#33422,#33423,
#33424,#33425,#33426,#33427,#33428,#33429,#33430,#33431,#33432,#33433,#33434,
#33435),.UNSPECIFIED.,.F.,.F.,(4,2,2,2,2,2,2,2,2,2,2,2,2,2,2,2,2,2,2,2,
2,2,2,2,2,2,2,2,2,2,2,2,2,2,2,2,2,2,2,2,2,2,2,2,2,2,2,2,2,2,2,2,2,2,2,2,
2,2,2,2,2,2,2,2,2,2,2,2,2,2,2,2,2,2,2,2,2,2,2,2,2,2,2,2,2,2,2,2,2,2,2,2,
2,2,2,2,2,2,2,2,2,4),(-2.69274389685463,-2.65996324899456,-2.5940083245505,
-2.58398511534276,-2.58035127739488,-2.57789588111239,-2.57568859799975,
-2.57266070754016,-2.5650433537799,-2.49977345661444,-2.45461787405291,
-2.43804912217385,-2.42576824498821,-2.42017276544664,-2.41592906755699,
-2.41190171986369,-2.40509070832018,-2.3862860780695,-2.28469466397845,
-2.27058696871724,-2.26126662798916,-2.25773342786145,-2.25529802074957,
-2.25307056346958,-2.249965360392,-2.24186588944671,-2.1913523066016,-2.14701024489156,
-2.10902042255395,-2.10074745671393,-2.09595409934006,-2.09175264908689,
-2.08652540626277,-2.07841887302653,-2.03121996720006,-1.95853249084424,
-1.94105335883462,-1.93643514861003,-1.93376367154131,-1.93138732723421,
-1.92820172854944,-1.92101776454692,-1.88925390955357,-1.81583422100394,
-1.78610184135241,-1.77807670352973,-1.77333719074546,-1.76954917635182,
-1.7644426491467,-1.75469352519467,-1.69098145621153,-1.62333472717303,
-1.6158904626649,-1.61289153189135,-1.61069103901612,-1.60822586071836,
-1.60454749758677,-1.5942058307455,-1.57794603520031,-1.52900603173646,
-1.46565346051885,-1.45740777443098,-1.4521380063163,-1.44793256000442,
-1.44316708803954,-1.43502378360481,-1.39923642008227,-1.35228919612668,
-1.30185436566104,-1.29375156543399,-1.29064560089792,-1.28841776736352,
-1.28598212442745,-1.28244889138968,-1.2731301027863,-1.25902781619956,
-1.15751015588664,-1.13867014178734,-1.13185348835024,-1.12782460480089,
-1.12358057710361,-1.11798685569063,-1.10571894011434,-1.08917192751295,
-1.04412096424067,-0.978594791679027,-0.970986860739619,-0.967960196775019,
-0.96575293080583,-0.963296487188248,-0.959659276591147,-0.949614993131925,
-0.883328351109479,-0.820657355393565,-0.812412410319363,-0.807143198990509,
-0.802938250023272,-0.798173398399364,-0.790031295670248,-0.754251857247748,
-0.707320128128854,-0.662256880685031),.UNSPECIFIED.);
#1380=B_SPLINE_CURVE_WITH_KNOTS('',3,(#33440,#33441,#33442,#33443,#33444,
#33445,#33446,#33447,#33448,#33449,#33450,#33451,#33452,#33453,#33454,#33455,
#33456,#33457,#33458,#33459,#33460,#33461,#33462,#33463,#33464,#33465,#33466,
#33467,#33468,#33469,#33470,#33471,#33472,#33473,#33474,#33475,#33476,#33477,
#33478,#33479,#33480,#33481,#33482,#33483,#33484,#33485,#33486,#33487,#33488,
#33489,#33490,#33491,#33492,#33493,#33494,#33495,#33496,#33497,#33498,#33499,
#33500,#33501,#33502,#33503,#33504,#33505,#33506,#33507,#33508,#33509,#33510,
#33511,#33512,#33513,#33514,#33515,#33516,#33517,#33518,#33519,#33520,#33521,
#33522,#33523,#33524,#33525,#33526,#33527,#33528,#33529,#33530,#33531,#33532,
#33533,#33534,#33535,#33536,#33537,#33538,#33539,#33540,#33541,#33542,#33543,
#33544,#33545,#33546,#33547,#33548,#33549,#33550,#33551,#33552,#33553,#33554,
#33555,#33556,#33557,#33558,#33559,#33560,#33561,#33562,#33563,#33564,#33565,
#33566,#33567,#33568,#33569,#33570,#33571,#33572,#33573,#33574,#33575,#33576,
#33577,#33578,#33579,#33580,#33581,#33582,#33583,#33584,#33585,#33586,#33587,
#33588,#33589,#33590,#33591,#33592,#33593,#33594,#33595,#33596,#33597,#33598,
#33599,#33600,#33601,#33602,#33603,#33604,#33605,#33606,#33607,#33608,#33609,
#33610,#33611,#33612,#33613,#33614,#33615,#33616,#33617,#33618,#33619,#33620,
#33621,#33622,#33623,#33624,#33625,#33626,#33627,#33628,#33629,#33630,#33631,
#33632,#33633,#33634,#33635,#33636,#33637,#33638,#33639,#33640,#33641,#33642,
#33643,#33644,#33645,#33646,#33647,#33648,#33649,#33650,#33651,#33652,#33653,
#33654,#33655,#33656,#33657),.UNSPECIFIED.,.F.,.F.,(4,2,2,2,2,2,2,2,2,2,
2,2,2,2,2,2,2,2,2,2,2,2,2,2,2,2,2,2,2,2,2,2,2,2,2,2,2,2,2,2,2,2,2,2,2,2,
2,2,2,2,2,2,2,2,2,2,2,2,2,2,2,2,2,2,2,2,2,2,2,2,2,2,2,2,2,2,2,2,2,2,2,2,
2,2,2,2,2,2,2,2,2,2,2,2,2,2,2,2,2,2,2,2,2,2,2,2,2,2,4),(-3.40027864395219,
-3.39526694442771,-3.38941664528869,-3.38513479929102,-3.38064707582144,
-3.37376289130956,-3.35440901647098,-3.25349185689639,-3.23941222672951,
-3.2301071528882,-3.22657797302984,-3.2241448060387,-3.22191905698823,-3.21881588799011,
-3.21071925123346,-3.16005988842744,-3.1133230111501,-3.07762309782326,
-3.06949051735682,-3.06473019178421,-3.06052864131234,-3.05526294501151,
-3.04702208958492,-2.98360963409326,-2.93459138745507,-2.9104066296905,
-2.90553506137354,-2.90280965241121,-2.90044706811189,-2.89741268022228,
-2.89237057074954,-2.85396102272484,-2.79740634168158,-2.75584017368339,
-2.74738372280542,-2.7425529794996,-2.73835898118844,-2.73319279679595,
-2.72527935641716,-2.68323185626629,-2.61954662882662,-2.59861448065653,
-2.59029328708264,-2.5840541974567,-2.58104653895082,-2.57869078990821,
-2.57591114724268,-2.57092920110732,-2.54770122314852,-2.54103958949081,
-2.51769360016757,-2.46110972276335,-2.44185341715776,-2.42807640219829,
-2.42222239734796,-2.41793908721741,-2.41345095531639,-2.40656840499489,
-2.38723392729998,-2.28626169830717,-2.27217738370819,-2.26286941054893,
-2.25933925954978,-2.25690546361179,-2.25467917162272,-2.25157528803708,
-2.24347710381067,-2.19253249529662,-2.1474855412448,-2.11049101346007,
-2.10227852593253,-2.09750004571732,-2.09329963031623,-2.08805796677039,
-2.07989874173682,-2.03094988061131,-1.97766068675707,-1.94419732416433,
-1.9392284989376,-1.93618286386817,-1.933823656949,-1.93107046631797,-1.92607223916869,
-1.899377481294,-1.81096924619372,-1.78660651889419,-1.77911620346404,-1.77449584112607,
-1.77026468109079,-1.76474619788352,-1.75287763519025,-1.70446713282638,
-1.64982835813692,-1.6213852828933,-1.61658671874534,-1.61359207313376,
-1.61123695707861,-1.60844677975401,-1.60327514517467,-1.57239511476165,
-1.5285964046287,-1.46723152820404,-1.45899225371714,-1.45372656266826,
-1.44952440599155,-1.44476273927614,-1.43662624933331,-1.40088236390028,
-1.36994781431221),.UNSPECIFIED.);
#1381=B_SPLINE_CURVE_WITH_KNOTS('',3,(#33659,#33660,#33661,#33662,#33663,
#33664,#33665,#33666,#33667,#33668,#33669,#33670,#33671,#33672,#33673,#33674,
#33675,#33676,#33677,#33678,#33679,#33680,#33681,#33682,#33683,#33684,#33685,
#33686,#33687,#33688,#33689,#33690,#33691,#33692,#33693,#33694,#33695,#33696,
#33697,#33698,#33699,#33700,#33701,#33702,#33703,#33704,#33705,#33706,#33707,
#33708,#33709,#33710,#33711,#33712,#33713,#33714,#33715,#33716,#33717,#33718,
#33719,#33720,#33721,#33722,#33723,#33724,#33725,#33726,#33727,#33728,#33729,
#33730,#33731,#33732,#33733,#33734,#33735,#33736),.UNSPECIFIED.,.F.,.F.,
(4,2,2,2,2,2,2,2,2,2,2,2,2,2,2,2,2,2,2,2,2,2,2,2,2,2,2,2,2,2,2,2,2,2,2,
2,2,2,4),(-0.662256880685031,-0.656877296145055,-0.648775583122173,-0.645670006523397,
-0.643442443997101,-0.641007089033966,-0.637474259638706,-0.628156454261886,
-0.614055584043697,-0.512542794514352,-0.49371098281102,-0.486895979214415,
-0.48286773840294,-0.47862414602344,-0.473030591614327,-0.46076136733263,
-0.444211480313638,-0.399143680132143,-0.333564903143002,-0.326020670736594,
-0.322739142773218,-0.320375640873755,-0.318176010640031,-0.314383106592926,
-0.303164557881548,-0.284950987202906,-0.191332929247415,-0.171536752245391,
-0.164589855766057,-0.160086291468646,-0.155807397011775,-0.149989534546236,
-0.136438317209894,-0.117596386639476,-0.065955914197476,-0.00962864573827704,
-0.00363211110775064,-0.00165261963449196,-0.000951735584449904),
 .UNSPECIFIED.);
#1382=B_SPLINE_CURVE_WITH_KNOTS('',3,(#33737,#33738,#33739,#33740,#33741,
#33742,#33743,#33744,#33745,#33746,#33747,#33748,#33749,#33750,#33751,#33752,
#33753,#33754,#33755,#33756,#33757,#33758,#33759,#33760,#33761,#33762,#33763,
#33764,#33765,#33766,#33767,#33768,#33769,#33770,#33771,#33772,#33773,#33774,
#33775,#33776,#33777,#33778,#33779,#33780,#33781,#33782,#33783,#33784,#33785,
#33786,#33787,#33788,#33789,#33790,#33791,#33792,#33793,#33794,#33795,#33796,
#33797,#33798,#33799,#33800,#33801,#33802,#33803,#33804,#33805,#33806,#33807,
#33808,#33809,#33810,#33811,#33812,#33813,#33814,#33815,#33816,#33817,#33818,
#33819,#33820,#33821,#33822,#33823,#33824,#33825,#33826,#33827,#33828,#33829,
#33830,#33831,#33832,#33833,#33834,#33835,#33836,#33837,#33838,#33839,#33840,
#33841,#33842,#33843,#33844,#33845,#33846,#33847,#33848,#33849,#33850,#33851,
#33852,#33853,#33854,#33855,#33856,#33857,#33858,#33859,#33860,#33861,#33862,
#33863,#33864,#33865,#33866,#33867,#33868,#33869,#33870,#33871,#33872,#33873,
#33874,#33875,#33876,#33877,#33878,#33879,#33880,#33881,#33882,#33883,#33884,
#33885,#33886,#33887,#33888,#33889,#33890,#33891,#33892,#33893,#33894),
 .UNSPECIFIED.,.F.,.F.,(4,2,2,2,2,2,2,2,2,2,2,2,2,2,2,2,2,2,2,2,2,2,2,2,
2,2,2,2,2,2,2,2,2,2,2,2,2,2,2,2,2,2,2,2,2,2,2,2,2,2,2,2,2,2,2,2,2,2,2,2,
2,2,2,2,2,2,2,2,2,2,2,2,2,2,2,2,2,2,4),(-4.06163372264747,-4.06090083217341,
-4.05900435491866,-4.05659198049401,-4.05306580980933,-4.04400200753387,
-4.03568916741852,-3.98543879491345,-3.93918649778018,-3.92066637708922,
-3.90729110492638,-3.90150374185163,-3.89723050404575,-3.89325829342407,
-3.8878019798035,-3.87382110036059,-3.79357017365643,-3.76076124325672,
-3.74964330261204,-3.74184665490773,-3.73927930858579,-3.73682194472232,
-3.73450029600026,-3.73112184376486,-3.7230361537368,-3.67475064583821,
-3.61817718020949,-3.59892315249405,-3.58514643440645,-3.57929093241746,
-3.57500586756126,-3.57051526509307,-3.56362757747713,-3.54426861783956,
-3.44337221043695,-3.42929223497135,-3.41998573316167,-3.41645485421019,
-3.41402012252149,-3.41179254465429,-3.40868620732549,-3.40057653174074,
-3.35066617553326,-3.30342367805876,-3.26753425095649,-3.25938624692227,
-3.25462046029077,-3.25041620156123,-3.24514986418576,-3.23691327795004,
-3.17201045523559,-3.12129236130429,-3.1070474138008,-3.09766048185232,
-3.09411767594483,-3.09168055618969,-3.08945543886151,-3.08635859659279,
-3.07831743718965,-3.02270855622954,-2.97097056435548,-2.95305070559221,
-2.94000698244206,-2.93427582855313,-2.93001092255537,-2.92547593294475,
-2.91838505515609,-2.89748932659936,-2.88014702052472,-2.81136674876867,
-2.77857350240568,-2.77333289368799,-2.77052708218261,-2.76817160209282,
-2.76519263870322,-2.7604492421632,-2.73338088581184,-2.70810953216271,
-2.69294723752461),.UNSPECIFIED.);
#1383=B_SPLINE_CURVE_WITH_KNOTS('',3,(#33900,#33901,#33902,#33903,#33904,
#33905,#33906,#33907,#33908,#33909,#33910,#33911,#33912,#33913,#33914,#33915,
#33916,#33917,#33918,#33919,#33920,#33921,#33922,#33923,#33924,#33925,#33926,
#33927,#33928,#33929,#33930,#33931,#33932,#33933,#33934,#33935,#33936,#33937,
#33938,#33939,#33940,#33941,#33942,#33943,#33944,#33945,#33946,#33947,#33948,
#33949,#33950,#33951,#33952,#33953,#33954,#33955,#33956,#33957,#33958,#33959,
#33960,#33961,#33962,#33963,#33964,#33965,#33966,#33967,#33968,#33969,#33970,
#33971,#33972,#33973,#33974,#33975,#33976,#33977,#33978,#33979,#33980,#33981,
#33982,#33983,#33984,#33985,#33986,#33987,#33988,#33989,#33990,#33991,#33992,
#33993,#33994,#33995,#33996,#33997,#33998,#33999,#34000,#34001,#34002,#34003,
#34004,#34005,#34006,#34007,#34008,#34009,#34010,#34011,#34012,#34013,#34014,
#34015,#34016,#34017,#34018,#34019,#34020,#34021,#34022,#34023,#34024,#34025,
#34026,#34027,#34028,#34029,#34030,#34031,#34032,#34033,#34034,#34035,#34036,
#34037,#34038,#34039,#34040,#34041),.UNSPECIFIED.,.F.,.F.,(4,2,2,2,2,2,
2,2,2,2,2,2,2,2,2,2,2,2,2,2,2,2,2,2,2,2,2,2,2,2,2,2,2,2,2,2,2,2,2,2,2,2,
2,2,2,2,2,2,2,2,2,2,2,2,2,2,2,2,2,2,2,2,2,2,2,2,2,2,2,2,4),(-1.36980481141947,
-1.32341652796323,-1.27554671181702,-1.26742186076528,-1.2621910509795,
-1.25799212879625,-1.25320754541437,-1.24496482175383,-1.20743934642901,
-1.16273276497357,-1.1119896360613,-1.10389063917951,-1.10078687684696,
-1.0985608209876,-1.09612743440691,-1.09259814632891,-1.08329385649739,
-1.06921796811361,-0.968326292839698,-0.948978200079611,-0.942094196417019,
-0.937606050009271,-0.933323402980211,-0.927471381383577,-0.913704248453021,
-0.894463308978411,-0.837965362967141,-0.815715503893684,-0.806691117916107,
-0.784452820163578,-0.779530684541559,-0.776764726520455,-0.774407813870399,
-0.771382242225817,-0.765049905095009,-0.756568868566862,-0.735032763017293,
-0.668117090842425,-0.6299509699465,-0.621453761635813,-0.616564217155136,
-0.612374462419738,-0.607282778632391,-0.597591800752157,-0.535403448686576,
-0.465872499601115,-0.458460244996091,-0.45555576035116,-0.453162684317778,
-0.450611210514127,-0.446528747710044,-0.432781060465283,-0.408343299636457,
-0.328722171973697,-0.305241944957634,-0.297850193116277,-0.293252005429176,
-0.289185204219945,-0.283730560321841,-0.277790856802232,-0.267906981290785,
-0.247311259963206,-0.182682624183383,-0.140768332805188,-0.135193403957654,
-0.13228276483854,-0.129931615999683,-0.127070746644813,-0.121561146140149,
-0.0772847850799816,-0.000952358992618726),.UNSPECIFIED.);
#1384=B_SPLINE_CURVE_WITH_KNOTS('',3,(#34042,#34043,#34044,#34045,#34046,
#34047,#34048,#34049,#34050,#34051,#34052,#34053,#34054,#34055,#34056,#34057,
#34058,#34059,#34060,#34061,#34062,#34063,#34064,#34065,#34066,#34067,#34068,
#34069,#34070,#34071,#34072,#34073,#34074,#34075,#34076,#34077,#34078,#34079,
#34080,#34081,#34082,#34083,#34084,#34085,#34086,#34087,#34088,#34089,#34090,
#34091,#34092,#34093,#34094,#34095,#34096,#34097,#34098,#34099,#34100,#34101,
#34102,#34103,#34104,#34105,#34106,#34107,#34108,#34109,#34110,#34111,#34112,
#34113,#34114,#34115,#34116,#34117,#34118,#34119),.UNSPECIFIED.,.F.,.F.,
(4,2,2,2,2,2,2,2,2,2,2,2,2,2,2,2,2,2,2,2,2,2,2,2,2,2,2,2,2,2,2,2,2,2,2,
2,2,2,4),(-4.06145513647978,-4.0422638812803,-4.03712630964723,-4.03307460276732,
-4.02895028033439,-4.024215669444,-4.01619757626936,-3.98971687449884,-3.90906896261304,
-3.87808367814854,-3.87290930175311,-3.87011910938599,-3.86776485288048,
-3.86477243364192,-3.8599796077253,-3.83164267722664,-3.74766161698994,
-3.73003418075558,-3.72116690810042,-3.71374178296504,-3.71032224720732,
-3.70621477598371,-3.70136056789861,-3.6930168007416,-3.65776196781635,
-3.58879107135689,-3.56646281699231,-3.55777612704599,-3.55132561329452,
-3.54827763231599,-3.5459191678788,-3.54316981152524,-3.53831967340618,
-3.51714447982317,-3.50633181035696,-3.48468857206439,-3.42825403950671,
-3.40902715140468,-3.40027864395219),.UNSPECIFIED.);
#1385=B_SPLINE_CURVE_WITH_KNOTS('',3,(#34120,#34121,#34122,#34123,#34124,
#34125,#34126,#34127,#34128,#34129,#34130,#34131,#34132,#34133,#34134,#34135,
#34136,#34137,#34138,#34139,#34140,#34141,#34142,#34143,#34144,#34145,#34146,
#34147,#34148,#34149,#34150,#34151,#34152,#34153,#34154,#34155,#34156,#34157,
#34158,#34159,#34160,#34161,#34162,#34163,#34164,#34165,#34166,#34167,#34168,
#34169,#34170,#34171,#34172,#34173,#34174,#34175,#34176,#34177,#34178,#34179,
#34180,#34181,#34182,#34183,#34184,#34185,#34186,#34187,#34188,#34189,#34190,
#34191,#34192,#34193,#34194,#34195,#34196,#34197,#34198,#34199,#34200,#34201,
#34202,#34203,#34204,#34205,#34206,#34207,#34208,#34209,#34210,#34211,#34212,
#34213,#34214,#34215,#34216,#34217,#34218,#34219,#34220,#34221,#34222,#34223,
#34224,#34225,#34226,#34227,#34228,#34229,#34230,#34231,#34232,#34233,#34234,
#34235,#34236,#34237,#34238,#34239,#34240,#34241,#34242,#34243,#34244,#34245,
#34246,#34247,#34248,#34249,#34250,#34251,#34252,#34253,#34254,#34255,#34256,
#34257,#34258,#34259,#34260,#34261,#34262,#34263,#34264,#34265,#34266,#34267,
#34268,#34269,#34270,#34271,#34272,#34273,#34274,#34275,#34276,#34277,#34278,
#34279,#34280,#34281,#34282,#34283,#34284,#34285,#34286,#34287,#34288,#34289,
#34290,#34291,#34292,#34293,#34294,#34295,#34296,#34297,#34298,#34299,#34300,
#34301,#34302,#34303,#34304,#34305,#34306,#34307,#34308,#34309,#34310,#34311,
#34312,#34313,#34314,#34315,#34316,#34317,#34318,#34319,#34320,#34321,#34322,
#34323,#34324,#34325,#34326,#34327,#34328,#34329,#34330,#34331,#34332,#34333,
#34334,#34335,#34336,#34337,#34338,#34339,#34340,#34341,#34342,#34343,#34344,
#34345),.UNSPECIFIED.,.F.,.F.,(4,2,2,2,2,2,2,2,2,2,2,2,2,2,2,2,2,2,2,2,
2,2,2,2,2,2,2,2,2,2,2,2,2,2,2,2,2,2,2,2,2,2,2,2,2,2,2,2,2,2,2,2,2,2,2,2,
2,2,2,2,2,2,2,2,2,2,2,2,2,2,2,2,2,2,2,2,2,2,2,2,2,2,2,2,2,2,2,2,2,2,2,2,
2,2,2,2,2,2,2,2,2,2,2,2,2,2,2,2,2,2,2,2,4),(-2.69294723752461,-2.65114166127505,
-2.63181396086124,-2.61799640926919,-2.61213315788334,-2.60784590043303,
-2.60335613546443,-2.59647601992327,-2.57717949710199,-2.47617437505175,
-2.46208757005142,-2.45277710062453,-2.44924507369218,-2.44680966336363,
-2.44458155476218,-2.44147459533425,-2.43336418601692,-2.38157162990355,
-2.37298842654651,-2.32480243453079,-2.30758873872382,-2.29494035023141,
-2.28927783393323,-2.28502293341102,-2.28101405079215,-2.27430449711245,
-2.25622315165895,-2.16995516693249,-2.13684558241765,-2.12951271702238,
-2.12630037498813,-2.12392005477092,-2.12126171208211,-2.11670430902634,
-2.09996784983596,-2.08665881394654,-2.03183369741423,-1.97954074051042,
-1.97130879662538,-1.9660428950167,-1.96183739832574,-1.95706850714249,
-1.94891095631621,-1.91290303137255,-1.86535722859543,-1.81579391890578,
-1.80765968408705,-1.8045492720663,-1.80232012024329,-1.79988521408916,
-1.79635666691738,-1.78707100068286,-1.77303702667756,-1.67331007621292,
-1.65298228369763,-1.64596485836122,-1.64144513344539,-1.63717202275139,
-1.63139494962487,-1.61808965204889,-1.59969713392372,-1.54545706187921,
-1.49319291279325,-1.48508401720847,-1.48197723602652,-1.47974919675262,
-1.47731377152151,-1.4737815900337,-1.46446980817128,-1.45038184132571,
-1.34924079925545,-1.33009444563955,-1.32323508400709,-1.31919800705343,
-1.3149576750696,-1.30938945997497,-1.29726169630753,-1.24669001698659,
-1.22062722971483,-1.17066707417821,-1.16255486676606,-1.15944791094389,
-1.15722001831758,-1.15478506997232,-1.15125410628924,-1.14194855991097,
-1.12787268113652,-1.02701120747538,-1.00765021694377,-1.00076162194502,
-0.996270360425195,-0.991984614187713,-0.986128100508921,-0.972348724095114,
-0.953088506286536,-0.896494914806161,-0.873040381868709,-0.865828054025307,
-0.843168610135076,-0.838220322747817,-0.835447281227641,-0.833089210539276,
-0.830068271402717,-0.823766420254556,-0.815339323042691,-0.79401332656967,
-0.728081236908415,-0.688745099378829,-0.680183173896067,-0.675276899599574,
-0.671124902893915,-0.666062812089729,-0.662308805568785),.UNSPECIFIED.);
#1386=B_SPLINE_CURVE_WITH_KNOTS('',3,(#34350,#34351,#34352,#34353,#34354,
#34355,#34356,#34357,#34358,#34359,#34360,#34361,#34362,#34363,#34364,#34365,
#34366,#34367,#34368,#34369,#34370,#34371,#34372,#34373,#34374,#34375,#34376,
#34377,#34378,#34379,#34380,#34381,#34382,#34383,#34384,#34385,#34386,#34387,
#34388,#34389,#34390,#34391,#34392,#34393,#34394,#34395,#34396,#34397,#34398,
#34399,#34400,#34401,#34402,#34403,#34404,#34405,#34406,#34407,#34408,#34409,
#34410,#34411,#34412,#34413,#34414,#34415,#34416,#34417,#34418,#34419,#34420,
#34421,#34422,#34423,#34424,#34425,#34426,#34427,#34428,#34429,#34430,#34431,
#34432,#34433,#34434,#34435,#34436,#34437,#34438,#34439,#34440,#34441,#34442,
#34443,#34444,#34445,#34446,#34447,#34448,#34449,#34450,#34451,#34452,#34453,
#34454,#34455,#34456,#34457,#34458,#34459,#34460,#34461,#34462,#34463,#34464,
#34465,#34466,#34467,#34468,#34469,#34470,#34471,#34472,#34473,#34474,#34475,
#34476,#34477,#34478,#34479,#34480,#34481,#34482,#34483,#34484,#34485,#34486,
#34487,#34488,#34489,#34490,#34491,#34492,#34493,#34494,#34495,#34496,#34497,
#34498,#34499,#34500,#34501,#34502,#34503,#34504,#34505,#34506,#34507,#34508,
#34509,#34510,#34511,#34512,#34513,#34514,#34515,#34516,#34517,#34518,#34519,
#34520,#34521,#34522,#34523,#34524,#34525,#34526,#34527,#34528,#34529,#34530,
#34531,#34532,#34533,#34534,#34535,#34536,#34537,#34538,#34539,#34540,#34541,
#34542,#34543,#34544,#34545,#34546,#34547,#34548,#34549,#34550,#34551,#34552,
#34553,#34554,#34555,#34556,#34557,#34558,#34559,#34560,#34561,#34562,#34563,
#34564,#34565),.UNSPECIFIED.,.F.,.F.,(4,2,2,2,2,2,2,2,2,2,2,2,2,2,2,2,2,
2,2,2,2,2,2,2,2,2,2,2,2,2,2,2,2,2,2,2,2,2,2,2,2,2,2,2,2,2,2,2,2,2,2,2,2,
2,2,2,2,2,2,2,2,2,2,2,2,2,2,2,2,2,2,2,2,2,2,2,2,2,2,2,2,2,2,2,2,2,2,2,2,
2,2,2,2,2,2,2,2,2,2,2,2,2,2,2,2,2,2,4),(-3.40037133238205,-3.3958593199486,
-3.36461546646417,-3.35943142736421,-3.35663906111019,-3.35428480070634,
-3.35129470908302,-3.34650999012586,-3.31837920720899,-3.23419825261601,
-3.21655274783487,-3.2036644360115,-3.19796339735095,-3.19370627167876,
-3.18916588739566,-3.1820379692777,-3.16081370545087,-3.06213476930674,
-3.04814411461567,-3.03888249310273,-3.03535972342486,-3.03292778189279,
-3.03070060100281,-3.0275920900534,-3.019455869361,-2.97008671586442,-2.89623041871921,
-2.88180790630273,-2.87584804982145,-2.87154627579255,-2.8676157056339,
-2.86232064216408,-2.85195609985107,-2.77070955610631,-2.72112689413215,
-2.71503129612839,-2.71205177402978,-2.70992356231367,-2.70721432005216,
-2.70254137908967,-2.68371305149385,-2.59157465470434,-2.57258995275449,
-2.5589611656633,-2.55313250144345,-2.54885396683467,-2.5443583614553,-2.53743917911911,
-2.51783342132499,-2.41720738501874,-2.40313773446656,-2.39383723351361,
-2.39030846532504,-2.38787516400173,-2.38564895831586,-2.38254471582826,
-2.37444200018048,-2.32258548975452,-2.26808310769906,-2.24964664370148,
-2.23631799341665,-2.2305396995894,-2.22626907552939,-2.22175513490086,
-2.21475326426898,-2.19452066729164,-2.1108810785795,-2.07484271013731,
-2.06950656862376,-2.06668153128964,-2.06432862136666,-2.06137659699598,
-2.05671950955988,-2.03127784426511,-1.95202516198594,-1.91905425562225,
-1.91088583218888,-1.90607042791539,-1.90187447426128,-1.89668623178858,
-1.88652523567147,-1.87352770166731,-1.84275512796906,-1.77770978290299,
-1.75210906098205,-1.74744428462096,-1.74448998382192,-1.74213703485185,
-1.73931406332338,-1.73398756143383,-1.69828432680799,-1.61866415959717,
-1.59497847791425,-1.58756282683782,-1.5829589000224,-1.57872303241422,
-1.57316971161573,-1.56111123827875,-1.51110459863466,-1.46986828877692,
-1.43039794495249,-1.42533913716731,-1.42229975558202,-1.41993645468558,
-1.41721389594947,-1.41235617664627,-1.38842975984289,-1.36980481141947),
 .UNSPECIFIED.);
#1387=B_SPLINE_CURVE_WITH_KNOTS('',3,(#34567,#34568,#34569,#34570,#34571,
#34572,#34573,#34574,#34575,#34576,#34577,#34578,#34579,#34580,#34581,#34582,
#34583,#34584,#34585,#34586,#34587,#34588,#34589,#34590,#34591,#34592,#34593,
#34594,#34595,#34596,#34597,#34598,#34599,#34600,#34601,#34602,#34603,#34604,
#34605,#34606,#34607,#34608,#34609,#34610,#34611,#34612,#34613,#34614,#34615,
#34616,#34617,#34618,#34619,#34620,#34621,#34622,#34623,#34624,#34625,#34626,
#34627,#34628,#34629,#34630,#34631,#34632,#34633,#34634,#34635,#34636,#34637,
#34638,#34639,#34640,#34641,#34642),.UNSPECIFIED.,.F.,.F.,(4,2,2,2,2,2,
2,2,2,2,2,2,2,2,2,2,2,2,2,2,2,2,2,2,2,2,2,2,2,2,2,2,2,2,2,2,2,4),(-0.662308805568785,
-0.656525263118195,-0.586929482800625,-0.525386354673078,-0.517571766729085,
-0.514510554571795,-0.512294682743695,-0.509848358376822,-0.506259578976813,
-0.496556046832651,-0.435653921453166,-0.372625495080247,-0.360019643289771,
-0.354426724262138,-0.350168227778875,-0.349648983064658,-0.345057398224343,
-0.340228047237268,-0.333051091433346,-0.320033327103222,-0.289193350981699,
-0.221973600570761,-0.198484353892505,-0.193484794861598,-0.190700046208865,
-0.188342919706885,-0.185337144945508,-0.179114016182033,-0.170822245801388,
-0.150006585591807,-0.0660721055234023,-0.0417239069242697,-0.0342311404955614,
-0.0296087078489306,-0.0255413886337936,-0.021440687782664,-0.016153695933201,
-0.000950919900370663),.UNSPECIFIED.);
#1388=B_SPLINE_CURVE_WITH_KNOTS('',3,(#34643,#34644,#34645,#34646,#34647,
#34648,#34649,#34650,#34651,#34652,#34653,#34654,#34655,#34656,#34657,#34658,
#34659,#34660,#34661,#34662,#34663,#34664,#34665,#34666,#34667,#34668,#34669,
#34670,#34671,#34672,#34673,#34674,#34675,#34676,#34677,#34678,#34679,#34680,
#34681,#34682,#34683,#34684,#34685,#34686,#34687,#34688,#34689,#34690,#34691,
#34692,#34693,#34694,#34695,#34696,#34697,#34698,#34699,#34700,#34701,#34702,
#34703,#34704,#34705,#34706,#34707,#34708,#34709,#34710,#34711,#34712,#34713,
#34714,#34715,#34716,#34717,#34718,#34719,#34720,#34721,#34722,#34723,#34724,
#34725,#34726,#34727,#34728,#34729,#34730,#34731,#34732,#34733,#34734,#34735,
#34736,#34737,#34738,#34739,#34740,#34741,#34742,#34743,#34744,#34745,#34746,
#34747,#34748,#34749,#34750,#34751,#34752,#34753,#34754,#34755,#34756,#34757,
#34758,#34759,#34760,#34761,#34762,#34763,#34764,#34765,#34766,#34767,#34768,
#34769,#34770,#34771,#34772,#34773,#34774,#34775,#34776,#34777,#34778,#34779,
#34780),.UNSPECIFIED.,.F.,.F.,(4,2,2,2,2,2,2,2,2,2,2,2,2,2,2,2,2,2,2,2,
2,2,2,2,2,2,2,2,2,2,2,2,2,2,2,2,2,2,2,2,2,2,2,2,2,2,2,2,2,2,2,2,2,2,2,2,
2,2,2,2,2,2,2,2,2,2,2,2,4),(-4.06059553295812,-3.95888332605128,-3.93524837446757,
-3.93040575401771,-3.92768599130884,-3.9253213196809,-3.92227524286053,
-3.91719504024668,-3.87604943766431,-3.81089170722431,-3.79021971726244,
-3.78030903390612,-3.77435754711254,-3.76892484895596,-3.76485148118313,
-3.76082383198741,-3.75400802355856,-3.73516237649858,-3.63364989820849,
-3.61954751977705,-3.61023032757608,-3.60669808252017,-3.60426325835415,
-3.60203627375543,-3.59893165064515,-3.59083310374198,-3.5404802435321,
-3.49355026739594,-3.45777721116723,-3.4496370066841,-3.44487322144071,
-3.44066918150538,-3.43540106762591,-3.42715768475613,-3.36386456999922,
-3.31186737826032,-3.29744028523237,-3.28796528639471,-3.28440978594458,
-3.28197032439139,-3.27974813701758,-3.27666196438192,-3.26869178579942,
-3.21093535955183,-3.18768781178593,-3.14124329271754,-3.12961283582514,
-3.12413720850642,-3.11991011376656,-3.11526540704156,-3.10767013904823,
-3.0824281790699,-3.01283257539637,-2.96930448439377,-2.96380394537079,
-2.96094378331988,-2.95859093184779,-2.95567520464474,-2.95008214425666,
-2.90249776912101,-2.86138340768888,-2.81825850899877,-2.80704977295758,
-2.8016538299286,-2.79743629801213,-2.79274908381092,-2.7849605057298,-2.75779268177983,
-2.69191355936612),.UNSPECIFIED.);
#1389=B_SPLINE_CURVE_WITH_KNOTS('',3,(#34786,#34787,#34788,#34789,#34790,
#34791,#34792,#34793,#34794,#34795,#34796,#34797,#34798,#34799,#34800,#34801,
#34802,#34803,#34804,#34805,#34806,#34807,#34808,#34809,#34810,#34811,#34812,
#34813,#34814,#34815,#34816,#34817,#34818,#34819,#34820,#34821,#34822,#34823,
#34824,#34825,#34826,#34827,#34828,#34829,#34830,#34831,#34832,#34833,#34834,
#34835,#34836,#34837,#34838,#34839,#34840,#34841,#34842,#34843,#34844,#34845,
#34846,#34847,#34848,#34849,#34850,#34851,#34852,#34853,#34854,#34855,#34856,
#34857,#34858,#34859,#34860,#34861,#34862,#34863,#34864,#34865,#34866,#34867,
#34868,#34869,#34870,#34871,#34872,#34873,#34874,#34875,#34876,#34877,#34878,
#34879,#34880,#34881,#34882,#34883,#34884,#34885,#34886,#34887,#34888,#34889,
#34890,#34891,#34892,#34893,#34894,#34895,#34896,#34897,#34898,#34899,#34900,
#34901,#34902,#34903,#34904,#34905,#34906,#34907,#34908,#34909,#34910,#34911,
#34912,#34913,#34914,#34915,#34916,#34917,#34918,#34919,#34920,#34921,#34922,
#34923,#34924,#34925,#34926,#34927,#34928,#34929),.UNSPECIFIED.,.F.,.F.,
(4,2,2,2,2,2,2,2,2,2,2,2,2,2,2,2,2,2,2,2,2,2,2,2,2,2,2,2,2,2,2,2,2,2,2,
2,2,2,2,2,2,2,2,2,2,2,2,2,2,2,2,2,2,2,2,2,2,2,2,2,2,2,2,2,2,2,2,2,2,2,2,
4),(-1.37014057674011,-1.37000038523809,-1.3193807857946,-1.29516072778694,
-1.28794739647049,-1.23944085044802,-1.23437673038055,-1.23133618776153,
-1.22897325908904,-1.22625261996907,-1.22140184539273,-1.19758604490048,
-1.13325547782832,-1.08466057967899,-1.0765147763891,-1.07127828277985,
-1.06707981996203,-1.06230119291961,-1.05408248317551,-1.01694453485038,
-0.971984850747004,-0.921098890522783,-0.913002195714879,-0.90989923696995,
-0.907673737784872,-0.905240936806457,-0.901712459963499,-0.892410089673449,
-0.878336912946387,-0.777450761854404,-0.758123107234341,-0.751242968602848,
-0.746756388476347,-0.742474540756264,-0.736622507855895,-0.722850111069251,
-0.703597973752917,-0.647026385171577,-0.598686011205405,-0.59058047704131,
-0.587476560923835,-0.585250979534515,-0.58281879237831,-0.579292375241125,
-0.570002155326508,-0.555953252340658,-0.455662334292326,-0.43585605009363,
-0.428911959908986,-0.424412009479871,-0.420137880887261,-0.414328645049147,
-0.400807926092358,-0.382016788533066,-0.280500189735869,-0.269127490375588,
-0.265186292790822,-0.262916720224567,-0.260516802362791,-0.25736183148815,
-0.250124370569427,-0.239787858198167,-0.210597176892684,-0.173489617417905,
-0.11762813045963,-0.109369838681646,-0.104099278939646,-0.0998978703794037,
-0.0951420049269887,-0.0870277655722719,-0.0772405797427724,-0.000952140262247388),
 .UNSPECIFIED.);
#1390=B_SPLINE_CURVE_WITH_KNOTS('',3,(#34930,#34931,#34932,#34933,#34934,
#34935,#34936,#34937,#34938,#34939,#34940,#34941,#34942,#34943,#34944,#34945,
#34946,#34947,#34948,#34949,#34950,#34951,#34952,#34953,#34954,#34955,#34956,
#34957,#34958,#34959,#34960,#34961,#34962,#34963,#34964,#34965,#34966,#34967,
#34968,#34969,#34970,#34971,#34972,#34973,#34974,#34975,#34976,#34977,#34978,
#34979,#34980,#34981,#34982,#34983,#34984,#34985,#34986,#34987,#34988,#34989,
#34990,#34991,#34992,#34993,#34994,#34995,#34996,#34997,#34998,#34999,#35000,
#35001,#35002,#35003,#35004,#35005),.UNSPECIFIED.,.F.,.F.,(4,2,2,2,2,2,
2,2,2,2,2,2,2,2,2,2,2,2,2,2,2,2,2,2,2,2,2,2,2,2,2,2,2,2,2,2,2,4),(-4.06103572343788,
-4.01111266036306,-4.00663360504596,-4.00374863469166,-4.00102817468496,
-3.99866538066405,-3.99562502280188,-3.99056125606958,-3.95060498761795,
-3.91948798465717,-3.89209660458075,-3.85648947981115,-3.84666528987173,
-3.84154653290425,-3.83735595568599,-3.83248973437651,-3.82409407820223,
-3.78771106943414,-3.72495828224382,-3.69921592901282,-3.68967868648822,
-3.68281122484818,-3.67968765308805,-3.67731308089062,-3.6746474636272,
-3.67004803658893,-3.6527550430313,-3.64006081604174,-3.61770346282282,
-3.5797117837695,-3.53230129714135,-3.52359491254894,-3.51871081598452,
-3.51494140355726,-3.51002247526951,-3.50139420653846,-3.46063952180805,
-3.40037133238205),.UNSPECIFIED.);
#1391=B_SPLINE_CURVE_WITH_KNOTS('',3,(#35006,#35007,#35008,#35009,#35010,
#35011,#35012,#35013,#35014,#35015,#35016,#35017,#35018,#35019,#35020,#35021,
#35022,#35023,#35024,#35025,#35026,#35027,#35028,#35029,#35030,#35031,#35032,
#35033,#35034,#35035,#35036,#35037,#35038,#35039,#35040,#35041,#35042,#35043,
#35044,#35045,#35046,#35047,#35048,#35049,#35050,#35051,#35052,#35053,#35054,
#35055,#35056,#35057,#35058,#35059,#35060,#35061,#35062,#35063,#35064,#35065,
#35066,#35067,#35068,#35069,#35070,#35071,#35072,#35073,#35074,#35075,#35076,
#35077,#35078,#35079,#35080,#35081,#35082,#35083,#35084,#35085,#35086,#35087,
#35088,#35089,#35090,#35091,#35092,#35093,#35094,#35095,#35096,#35097,#35098,
#35099,#35100,#35101,#35102,#35103,#35104,#35105,#35106,#35107,#35108,#35109,
#35110,#35111,#35112,#35113,#35114,#35115,#35116,#35117,#35118,#35119,#35120,
#35121,#35122,#35123,#35124,#35125,#35126,#35127,#35128,#35129,#35130,#35131,
#35132,#35133,#35134,#35135,#35136,#35137,#35138,#35139,#35140,#35141,#35142,
#35143,#35144,#35145,#35146,#35147,#35148,#35149,#35150,#35151,#35152,#35153,
#35154,#35155,#35156,#35157,#35158,#35159,#35160,#35161,#35162,#35163,#35164,
#35165,#35166,#35167,#35168,#35169,#35170,#35171,#35172,#35173,#35174,#35175,
#35176,#35177,#35178,#35179,#35180,#35181,#35182,#35183,#35184,#35185,#35186,
#35187,#35188,#35189,#35190,#35191,#35192,#35193,#35194,#35195,#35196,#35197,
#35198,#35199,#35200,#35201,#35202,#35203,#35204,#35205,#35206,#35207,#35208,
#35209,#35210,#35211,#35212,#35213,#35214,#35215,#35216,#35217,#35218,#35219,
#35220,#35221,#35222,#35223,#35224,#35225,#35226,#35227),.UNSPECIFIED.,
 .F.,.F.,(4,2,2,2,2,2,2,2,2,2,2,2,2,2,2,2,2,2,2,2,2,2,2,2,2,2,2,2,2,2,2,
2,2,2,2,2,2,2,2,2,2,2,2,2,2,2,2,2,2,2,2,2,2,2,2,2,2,2,2,2,2,2,2,2,2,2,2,
2,2,2,2,2,2,2,2,2,2,2,2,2,2,2,2,2,2,2,2,2,2,2,2,2,2,2,2,2,2,2,2,2,2,2,2,
2,2,2,2,2,2,2,4),(-2.69191355936612,-2.68184878374859,-2.64962750863557,
-2.6423934893288,-2.63919927472136,-2.63682209906018,-2.6341558565772,-2.62956020432886,
-2.61234432288922,-2.60098330413407,-2.57591806016906,-2.52723694506063,
-2.49083173187507,-2.48265195503412,-2.47787911405952,-2.47367556933407,
-2.4684192931653,-2.46021634347588,-2.40956999335524,-2.34700678403509,
-2.32346880895875,-2.31863028669715,-2.31591079164253,-2.31354501199639,
-2.31049580633884,-2.30540686246707,-2.26354995187619,-2.25253134760833,
-2.20458580732447,-2.16844021601739,-2.16027583885786,-2.15550616301101,
-2.15130190097621,-2.14604009487562,-2.13781946487149,-2.07571383695125,
-2.03064006336576,-2.0172676511193,-2.00058561198714,-1.99603367598981,
-1.99337692070661,-1.99099685029287,-1.98778329614877,-1.98044105258042,
-1.94724040026906,-1.85898861116881,-1.84253512974541,-1.83607419011304,
-1.83211250147999,-1.82782980143794,-1.82199251772878,-1.80832941595,-1.78928348067018,
-1.71356839938967,-1.67979596935156,-1.67481446707291,-1.67176421796371,
-1.6694034362481,-1.66665058441141,-1.66165818261176,-1.63512630614493,
-1.54858834939047,-1.52257507285416,-1.51490265947789,-1.51024077814487,
-1.50601742010814,-1.50057394912769,-1.48911607922425,-1.44404879580986,
-1.38460954364073,-1.35696735814146,-1.35219985850398,-1.34921368769467,
-1.34685785045237,-1.34405792536757,-1.33884490053971,-1.30685847525199,
-1.23957586650359,-1.20188800449964,-1.19341244981074,-1.18852555077207,
-1.18433224302438,-1.17922894686774,-1.16949301778481,-1.10613369689557,
-1.03807709736447,-1.03067441271345,-1.02768293077643,-1.02526607947621,
-1.0227474627466,-1.01881996720616,-1.00649400665832,-0.985670887700816,
-0.941849897092128,-0.880505614273177,-0.872254895929421,-0.866984078665993,
-0.862779174994307,-0.858015794923948,-0.849879749482219,-0.814192933173186,
-0.767509422180126,-0.716720398314151,-0.708620216122763,-0.705514949368648,
-0.703287539502368,-0.700852270274692,-0.697319430457627,-0.688000821502116,
-0.673898053427717,-0.661876260241505),.UNSPECIFIED.);
#1392=B_SPLINE_CURVE_WITH_KNOTS('',3,(#35232,#35233,#35234,#35235,#35236,
#35237,#35238,#35239,#35240,#35241,#35242,#35243,#35244,#35245,#35246,#35247,
#35248,#35249,#35250,#35251,#35252,#35253,#35254,#35255,#35256,#35257,#35258,
#35259,#35260,#35261,#35262,#35263,#35264,#35265,#35266,#35267,#35268,#35269,
#35270,#35271,#35272,#35273,#35274,#35275,#35276,#35277,#35278,#35279,#35280,
#35281,#35282,#35283,#35284,#35285,#35286,#35287,#35288,#35289,#35290,#35291,
#35292,#35293,#35294,#35295,#35296,#35297,#35298,#35299,#35300,#35301,#35302,
#35303,#35304,#35305,#35306,#35307,#35308,#35309,#35310,#35311,#35312,#35313,
#35314,#35315,#35316,#35317,#35318,#35319,#35320,#35321,#35322,#35323,#35324,
#35325,#35326,#35327,#35328,#35329,#35330,#35331,#35332,#35333,#35334,#35335,
#35336,#35337,#35338,#35339,#35340,#35341,#35342,#35343,#35344,#35345,#35346,
#35347,#35348,#35349,#35350,#35351,#35352,#35353,#35354,#35355,#35356,#35357,
#35358,#35359,#35360,#35361,#35362,#35363,#35364,#35365,#35366,#35367,#35368,
#35369,#35370,#35371,#35372,#35373,#35374,#35375,#35376,#35377,#35378,#35379,
#35380,#35381,#35382,#35383,#35384,#35385,#35386,#35387,#35388,#35389,#35390,
#35391,#35392,#35393,#35394,#35395,#35396,#35397,#35398,#35399,#35400,#35401,
#35402,#35403,#35404,#35405,#35406,#35407,#35408,#35409,#35410,#35411,#35412,
#35413,#35414,#35415,#35416,#35417,#35418,#35419,#35420,#35421,#35422,#35423,
#35424,#35425,#35426,#35427,#35428,#35429,#35430,#35431,#35432,#35433,#35434,
#35435,#35436,#35437,#35438,#35439,#35440,#35441,#35442,#35443,#35444,#35445,
#35446,#35447,#35448,#35449,#35450,#35451),.UNSPECIFIED.,.F.,.F.,(4,2,2,
2,2,2,2,2,2,2,2,2,2,2,2,2,2,2,2,2,2,2,2,2,2,2,2,2,2,2,2,2,2,2,2,2,2,2,2,
2,2,2,2,2,2,2,2,2,2,2,2,2,2,2,2,2,2,2,2,2,2,2,2,2,2,2,2,2,2,2,2,2,2,2,2,
2,2,2,2,2,2,2,2,2,2,2,2,2,2,2,2,2,2,2,2,2,2,2,2,2,2,2,2,2,2,2,2,2,2,4),
(-3.40033477739996,-3.36451418220255,-3.33850355115555,-3.33111351743207,
-3.32651564670777,-3.32227874675779,-3.31680827106374,-3.30487416089585,
-3.22773898162582,-3.1900469364208,-3.1779632482735,-3.16966070836856,-3.16628663904097,
-3.16388241527472,-3.16161871469554,-3.15770866018037,-3.14656464589143,
-3.08084765441228,-3.03933910296471,-3.01564263934699,-3.00848007315647,
-3.00393170810425,-2.99967690825306,-2.99409202163094,-2.98151862627548,
-2.92133643796569,-2.85769459535463,-2.84781615646045,-2.84420395718218,
-2.84175404779108,-2.83954465736003,-2.8365049872345,-2.82881132234366,
-2.76535631732625,-2.69747729850175,-2.68798195818182,-2.6829306540106,
-2.67878167373204,-2.67387214990161,-2.66528724282318,-2.62543708055649,
-2.55987084501661,-2.5284221931878,-2.52323029540692,-2.5204360395077,-2.51808159580471,
-2.51509306688751,-2.51031421349815,-2.48233870089724,-2.45774467888692,
-2.4178293170681,-2.38844757720453,-2.37584418266547,-2.3659262246695,-2.36078758776022,
-2.35659508371772,-2.35174273491474,-2.34341105506712,-2.30803325116887,
-2.23907837074787,-2.20615423957555,-2.20091164713636,-2.19810650158538,
-2.19575265274773,-2.19277726726955,-2.18804246373164,-2.16113197020524,
-2.13615846063419,-2.07881470212002,-2.05942088174506,-2.0455690874852,
-2.03970235134988,-2.03541660506637,-2.03146508881164,-2.02505016896687,
-2.0075942793239,-1.98108989651934,-1.93815233230172,-1.88842594322002,
-1.88030431591139,-1.87719744081582,-1.87497052391221,-1.8725377919158,
-1.86901210387502,-1.85973251796886,-1.84570732505606,-1.74611642997218,
-1.72568507524278,-1.71865819485597,-1.71413920400873,-1.70987168243653,
-1.70410980422073,-1.6908745101837,-1.67260435650092,-1.61900483391207,
-1.56587908927099,-1.55778575098311,-1.5546829209477,-1.5524572234158,-1.55002386706463,
-1.54649402176984,-1.5371848040134,-1.52309842385622,-1.42191052763166,
-1.40281271601991,-1.39596380719189,-1.39193125184546,-1.38769452300188,
-1.38212917220927,-1.37014057674011),.UNSPECIFIED.);
#1393=B_SPLINE_CURVE_WITH_KNOTS('',3,(#35453,#35454,#35455,#35456,#35457,
#35458,#35459,#35460,#35461,#35462,#35463,#35464,#35465,#35466,#35467,#35468,
#35469,#35470,#35471,#35472,#35473,#35474,#35475,#35476,#35477,#35478,#35479,
#35480,#35481,#35482,#35483,#35484,#35485,#35486,#35487,#35488,#35489,#35490,
#35491,#35492,#35493,#35494,#35495,#35496,#35497,#35498,#35499,#35500,#35501,
#35502,#35503,#35504,#35505,#35506,#35507,#35508,#35509,#35510,#35511,#35512,
#35513,#35514,#35515,#35516,#35517,#35518,#35519,#35520,#35521,#35522),
 .UNSPECIFIED.,.F.,.F.,(4,2,2,2,2,2,2,2,2,2,2,2,2,2,2,2,2,2,2,2,2,2,2,2,
2,2,2,2,2,2,2,2,2,2,4),(-0.661876260241505,-0.572320924024388,-0.553546536125019,
-0.546739796163848,-0.542713278014369,-0.538469198202907,-0.5328711239966,
-0.520575991442001,-0.503980548303871,-0.458702214209073,-0.393461964550517,
-0.385869562379819,-0.382858738152879,-0.380655689035602,-0.378195099557297,
-0.37464115581892,-0.364986332431045,-0.30404935934828,-0.240988525311571,
-0.229681154669253,-0.223539690090359,-0.219245040381863,-0.214841833708473,
-0.2083721085236,-0.190531876219844,-0.141603338064727,-0.106446414563869,
-0.0678662765952388,-0.0628192245705687,-0.0597824591305558,-0.0574183589611437,
-0.0551959211726501,-0.0524918835236233,-0.0484568488096544,-0.000950994778662939),
 .UNSPECIFIED.);
#1394=B_SPLINE_CURVE_WITH_KNOTS('',3,(#35523,#35524,#35525,#35526,#35527,
#35528,#35529,#35530,#35531,#35532,#35533,#35534,#35535,#35536,#35537,#35538,
#35539,#35540,#35541,#35542,#35543,#35544,#35545,#35546,#35547,#35548,#35549,
#35550,#35551,#35552,#35553,#35554,#35555,#35556,#35557,#35558,#35559,#35560,
#35561,#35562,#35563,#35564,#35565,#35566,#35567,#35568,#35569,#35570,#35571,
#35572,#35573,#35574,#35575,#35576,#35577,#35578,#35579,#35580,#35581,#35582,
#35583,#35584,#35585,#35586,#35587,#35588,#35589,#35590,#35591,#35592,#35593,
#35594,#35595,#35596,#35597,#35598,#35599,#35600,#35601,#35602,#35603,#35604,
#35605,#35606,#35607,#35608,#35609,#35610,#35611,#35612,#35613,#35614,#35615,
#35616,#35617,#35618,#35619,#35620,#35621,#35622,#35623,#35624,#35625,#35626,
#35627,#35628,#35629,#35630,#35631,#35632,#35633,#35634,#35635,#35636,#35637,
#35638,#35639,#35640,#35641,#35642,#35643,#35644,#35645,#35646,#35647,#35648,
#35649,#35650,#35651,#35652,#35653,#35654,#35655,#35656,#35657,#35658,#35659,
#35660,#35661,#35662),.UNSPECIFIED.,.F.,.F.,(4,2,2,2,2,2,2,2,2,2,2,2,2,
2,2,2,2,2,2,2,2,2,2,2,2,2,2,2,2,2,2,2,2,2,2,2,2,2,2,2,2,2,2,2,2,2,2,2,2,
2,2,2,2,2,2,2,2,2,2,2,2,2,2,2,2,2,2,2,2,4),(-4.06190321821732,-3.99422219017382,
-3.97055969618172,-3.96339910922043,-3.95885005861324,-3.95459322681607,
-3.94900360402586,-3.93641013908849,-3.8748315541624,-3.82586292660814,
-3.81187828161991,-3.80272526927325,-3.79927138958828,-3.79681032664915,
-3.79460892351872,-3.7916029889917,-3.78411212354339,-3.71793194295498,
-3.6733174284296,-3.65686896625554,-3.64465770667096,-3.6390757450808,-3.63483492100245,
-3.63080480393728,-3.62397561334912,-3.60503312976436,-3.50364423680699,
-3.48954690802705,-3.48023227199527,-3.47670048658262,-3.47426581837415,
-3.47203884804385,-3.46893407685902,-3.46083389013004,-3.41047959829797,
-3.36355562486356,-3.32778547468295,-3.31964567368704,-3.31488208908652,
-3.31067820477749,-3.30541025749043,-3.29716707957948,-3.23382824406505,
-3.16813114773904,-3.15812373709248,-3.15449216483051,-3.15203728119064,
-3.14982966319807,-3.14680030871249,-3.13917403202114,-3.07407371279547,
-3.02880893743353,-3.01221655438943,-2.99992222681121,-2.99432438848688,
-2.990080422085,-2.9860539490331,-2.97924718064494,-2.96047213070521,-2.85884726887721,
-2.84473855296375,-2.83541776800587,-2.83188454890107,-2.82944917580603,
-2.82722178686823,-2.82411672792176,-2.81601799617708,-2.76521927448344,
-2.72039759015022,-2.69283977885968),.UNSPECIFIED.);
#1395=B_SPLINE_CURVE_WITH_KNOTS('',3,(#35668,#35669,#35670,#35671,#35672,
#35673,#35674,#35675,#35676,#35677,#35678,#35679,#35680,#35681,#35682,#35683,
#35684,#35685,#35686,#35687,#35688,#35689,#35690,#35691,#35692,#35693,#35694,
#35695,#35696,#35697,#35698,#35699,#35700,#35701,#35702,#35703,#35704,#35705,
#35706,#35707,#35708,#35709,#35710,#35711,#35712,#35713,#35714,#35715,#35716,
#35717,#35718,#35719,#35720,#35721,#35722,#35723,#35724,#35725,#35726,#35727,
#35728,#35729,#35730,#35731,#35732,#35733,#35734,#35735,#35736,#35737,#35738,
#35739,#35740,#35741,#35742,#35743,#35744,#35745,#35746,#35747,#35748,#35749,
#35750,#35751,#35752,#35753,#35754,#35755,#35756,#35757,#35758,#35759,#35760,
#35761,#35762,#35763,#35764,#35765,#35766,#35767,#35768,#35769,#35770,#35771,
#35772,#35773,#35774,#35775,#35776,#35777,#35778,#35779,#35780,#35781,#35782,
#35783,#35784,#35785,#35786,#35787,#35788,#35789,#35790,#35791,#35792,#35793,
#35794,#35795,#35796,#35797,#35798,#35799,#35800,#35801,#35802,#35803,#35804,
#35805,#35806,#35807,#35808,#35809,#35810,#35811,#35812,#35813,#35814,#35815,
#35816,#35817,#35818,#35819),.UNSPECIFIED.,.F.,.F.,(4,2,2,2,2,2,2,2,2,2,
2,2,2,2,2,2,2,2,2,2,2,2,2,2,2,2,2,2,2,2,2,2,2,2,2,2,2,2,2,2,2,2,2,2,2,2,
2,2,2,2,2,2,2,2,2,2,2,2,2,2,2,2,2,2,2,2,2,2,2,2,2,2,2,2,2,4),(-1.36941396256219,
-1.36567125877387,-1.36256519446724,-1.3603385606735,-1.35790579117546,
-1.35437947282384,-1.3450949253861,-1.33105934135082,-1.23119524877981,
-1.2109976269388,-1.20400105397277,-1.1994887562077,-1.19521841603027,-1.18943853237784,
-1.17609730223273,-1.15763496963987,-1.10298764942891,-1.09179077007889,
-1.04736457836952,-1.04177860583558,-1.03886563031094,-1.03651450757192,
-1.0336559940036,-1.02815750410302,-0.984557784383335,-0.914759998588243,
-0.889775031193937,-0.882217711290876,-0.877583393414395,-0.873357408829341,
-0.867871374442199,-0.856173209670865,-0.809150724069344,-0.761825987984907,
-0.724874978609838,-0.719855993301959,-0.716828534531096,-0.714466915061892,
-0.711737384530986,-0.706846024282249,-0.682280119155158,-0.633661570419317,
-0.570348738278909,-0.562109401936436,-0.556844416364295,-0.552643297270848,
-0.547883314433281,-0.539750969759379,-0.504048928642275,-0.457305903810248,
-0.406599904726469,-0.398502409888869,-0.395399233446972,-0.393173600361015,
-0.39074067891769,-0.387554196341755,-0.37943853462475,-0.367584231869073,
-0.331091999866335,-0.264847340178948,-0.24414433185155,-0.237073252008063,
-0.232544979681656,-0.228282230844111,-0.22254764351051,-0.21017947980432,
-0.166197233753262,-0.128329136877823,-0.0803772908676197,-0.074784322698507,
-0.0718699129930306,-0.0695188657834898,-0.0666619408875339,-0.063582754698667,
-0.0586294751953665,-0.000951400989500799),.UNSPECIFIED.);
#1396=B_SPLINE_CURVE_WITH_KNOTS('',3,(#35820,#35821,#35822,#35823,#35824,
#35825,#35826,#35827,#35828,#35829,#35830,#35831,#35832,#35833,#35834,#35835,
#35836,#35837,#35838,#35839,#35840,#35841,#35842,#35843,#35844,#35845,#35846,
#35847,#35848,#35849,#35850,#35851,#35852,#35853,#35854,#35855,#35856,#35857,
#35858,#35859,#35860,#35861,#35862,#35863,#35864,#35865,#35866,#35867,#35868,
#35869,#35870,#35871,#35872,#35873,#35874,#35875,#35876,#35877,#35878,#35879,
#35880,#35881,#35882,#35883,#35884,#35885,#35886,#35887,#35888,#35889),
 .UNSPECIFIED.,.F.,.F.,(4,2,2,2,2,2,2,2,2,2,2,2,2,2,2,2,2,2,2,2,2,2,2,2,
2,2,2,2,2,2,2,2,2,2,4),(-4.06178433014842,-4.00353083390514,-3.98468044596785,
-3.97655881826495,-3.97180080007593,-3.96759880296338,-3.96232925015822,
-3.95407588946756,-3.8991026474051,-3.85978061779031,-3.81936128801146,
-3.81347417331262,-3.81048213195841,-3.80812750190857,-3.80533605518293,
-3.80030150671206,-3.77615673484903,-3.69579946579093,-3.66229614839818,
-3.65416274448491,-3.64940234866229,-3.64520098502292,-3.63993585289152,
-3.6316965273176,-3.56800979274994,-3.51680918182206,-3.50211987978418,
-3.49251965507249,-3.48894732612245,-3.48650560963042,-3.48428877922437,
-3.48121973697877,-3.47335055387537,-3.41284908074069,-3.40033477739996),
 .UNSPECIFIED.);
#1397=B_SPLINE_CURVE_WITH_KNOTS('',3,(#35890,#35891,#35892,#35893,#35894,
#35895,#35896,#35897,#35898,#35899,#35900,#35901,#35902,#35903,#35904,#35905,
#35906,#35907,#35908,#35909,#35910,#35911,#35912,#35913,#35914,#35915,#35916,
#35917,#35918,#35919,#35920,#35921,#35922,#35923,#35924,#35925,#35926,#35927,
#35928,#35929,#35930,#35931,#35932,#35933,#35934,#35935,#35936,#35937,#35938,
#35939,#35940,#35941,#35942,#35943,#35944,#35945,#35946,#35947,#35948,#35949,
#35950,#35951,#35952,#35953,#35954,#35955,#35956,#35957,#35958,#35959,#35960,
#35961,#35962,#35963,#35964,#35965,#35966,#35967,#35968,#35969,#35970,#35971,
#35972,#35973,#35974,#35975,#35976,#35977,#35978,#35979,#35980,#35981,#35982,
#35983,#35984,#35985,#35986,#35987,#35988,#35989,#35990,#35991,#35992,#35993,
#35994,#35995,#35996,#35997,#35998,#35999,#36000,#36001,#36002,#36003,#36004,
#36005,#36006,#36007,#36008,#36009,#36010,#36011,#36012,#36013,#36014,#36015,
#36016,#36017,#36018,#36019,#36020,#36021,#36022,#36023,#36024,#36025,#36026,
#36027,#36028,#36029,#36030,#36031,#36032,#36033,#36034,#36035,#36036,#36037,
#36038,#36039,#36040,#36041,#36042,#36043,#36044,#36045,#36046,#36047,#36048,
#36049,#36050,#36051,#36052,#36053,#36054,#36055,#36056,#36057,#36058,#36059,
#36060,#36061,#36062,#36063,#36064,#36065,#36066,#36067,#36068,#36069,#36070,
#36071,#36072,#36073,#36074,#36075,#36076,#36077,#36078,#36079,#36080,#36081,
#36082,#36083,#36084,#36085,#36086,#36087,#36088,#36089,#36090,#36091,#36092,
#36093,#36094,#36095,#36096,#36097,#36098,#36099,#36100,#36101,#36102,#36103,
#36104,#36105),.UNSPECIFIED.,.F.,.F.,(4,2,2,2,2,2,2,2,2,2,2,2,2,2,2,2,2,
2,2,2,2,2,2,2,2,2,2,2,2,2,2,2,2,2,2,2,2,2,2,2,2,2,2,2,2,2,2,2,2,2,2,2,2,
2,2,2,2,2,2,2,2,2,2,2,2,2,2,2,2,2,2,2,2,2,2,2,2,2,2,2,2,2,2,2,2,2,2,2,2,
2,2,2,2,2,2,2,2,2,2,2,2,2,2,2,2,2,2,4),(-2.69283977885968,-2.68310143069254,
-2.67486842657118,-2.67008382205593,-2.66588145365924,-2.66064181106887,
-2.65249425890529,-2.6040282498421,-2.5395143715343,-2.51566065414712,-2.51080437591683,
-2.50808091287636,-2.50571563196259,-2.50267207434551,-2.49760289340965,
-2.4493558749743,-2.38969344019534,-2.35975336139693,-2.35202110529889,
-2.3473457218264,-2.34312475982452,-2.33770483192546,-2.32637338422226,
-2.24360973717306,-2.19520167284159,-2.1891354034682,-2.18616010202923,
-2.18403074095888,-2.18131416729415,-2.1766156201239,-2.15758405085398,
-2.13962149982905,-2.08910379444174,-2.05589198032722,-2.04222192887267,
-2.03164773590248,-2.02637447863243,-2.02216869983366,-2.01740547459455,
-2.00927255057752,-1.97365243170672,-1.92715710254637,-1.87608125906569,
-1.86797966132223,-1.86487384958149,-1.86264604821053,-1.8602103502604,
-1.85667688735662,-1.84735662834868,-1.83325135735085,-1.73165577321704,
-1.71287855813683,-1.70607068749421,-1.70204347380289,-1.69779864143056,
-1.69219954182274,-1.67990202192771,-1.66330326673895,-1.61801516288957,
-1.55285138063636,-1.54522308403937,-1.5421929733796,-1.53998483256562,
-1.5375293792845,-1.53389700427618,-1.52388744873649,-1.45817510242357,
-1.39488300134366,-1.38663835196857,-1.38136921780606,-1.37716425918247,
-1.37239932032969,-1.36425687814767,-1.3284723920359,-1.28152717622446,
-1.23110305766583,-1.2230011511352,-1.21989553930169,-1.21766796129195,
-1.2152326006997,-1.21169978210103,-1.2023821144702,-1.18828154869582,-1.08677807519096,
-1.06793823194321,-1.06112208448301,-1.0570936119629,-1.0528500986747,-1.04725719223619,
-1.03499162792078,-1.01844816000191,-0.973409877764712,-0.907879741590399,
-0.900273377247643,-0.897247178914939,-0.895040196902427,-0.892584002742436,
-0.888947046875392,-0.878902737495788,-0.812604056616784,-0.749961830993934,
-0.741717683855692,-0.736449034312483,-0.732244566690971,-0.727480295875256,
-0.719339273909858,-0.683566234576041,-0.662425644205117),.UNSPECIFIED.);
#1398=B_SPLINE_CURVE_WITH_KNOTS('',3,(#36110,#36111,#36112,#36113,#36114,
#36115,#36116,#36117,#36118,#36119,#36120,#36121,#36122,#36123,#36124,#36125,
#36126,#36127,#36128,#36129,#36130,#36131,#36132,#36133,#36134,#36135,#36136,
#36137,#36138,#36139,#36140,#36141,#36142,#36143,#36144,#36145,#36146,#36147,
#36148,#36149,#36150,#36151,#36152,#36153,#36154,#36155,#36156,#36157,#36158,
#36159,#36160,#36161,#36162,#36163,#36164,#36165,#36166,#36167,#36168,#36169,
#36170,#36171,#36172,#36173,#36174,#36175,#36176,#36177,#36178,#36179,#36180,
#36181,#36182,#36183,#36184,#36185,#36186,#36187,#36188,#36189,#36190,#36191,
#36192,#36193,#36194,#36195,#36196,#36197,#36198,#36199,#36200,#36201,#36202,
#36203,#36204,#36205,#36206,#36207,#36208,#36209,#36210,#36211,#36212,#36213,
#36214,#36215,#36216,#36217,#36218,#36219,#36220,#36221,#36222,#36223,#36224,
#36225,#36226,#36227,#36228,#36229,#36230,#36231,#36232,#36233,#36234,#36235,
#36236,#36237,#36238,#36239,#36240,#36241,#36242,#36243,#36244,#36245,#36246,
#36247,#36248,#36249,#36250,#36251,#36252,#36253,#36254,#36255,#36256,#36257,
#36258,#36259,#36260,#36261,#36262,#36263,#36264,#36265,#36266,#36267,#36268,
#36269,#36270,#36271,#36272,#36273,#36274,#36275,#36276,#36277,#36278,#36279,
#36280,#36281,#36282,#36283,#36284,#36285,#36286,#36287,#36288,#36289,#36290,
#36291,#36292,#36293,#36294,#36295,#36296,#36297,#36298,#36299,#36300,#36301,
#36302,#36303,#36304,#36305,#36306,#36307,#36308,#36309,#36310,#36311,#36312,
#36313,#36314,#36315,#36316,#36317,#36318,#36319),.UNSPECIFIED.,.F.,.F.,
(4,2,2,2,2,2,2,2,2,2,2,2,2,2,2,2,2,2,2,2,2,2,2,2,2,2,2,2,2,2,2,2,2,2,2,
2,2,2,2,2,2,2,2,2,2,2,2,2,2,2,2,2,2,2,2,2,2,2,2,2,2,2,2,2,2,2,2,2,2,2,2,
2,2,2,2,2,2,2,2,2,2,2,2,2,2,2,2,2,2,2,2,2,2,2,2,2,2,2,2,2,2,2,2,2,4),(-3.39960000691215,
-3.33661693680887,-3.3142928808857,-3.30560723188051,-3.29915729582697,
-3.2961093980794,-3.29375090991268,-3.29100142371395,-3.28615082295111,
-3.26496947575705,-3.25416660749216,-3.23251988293263,-3.17608430484181,
-3.15685709260627,-3.14309666001341,-3.13724627010666,-3.13296435954881,
-3.12847657010988,-3.12159228779436,-3.10223816022417,-3.00131944827361,
-2.98723960602559,-2.97793439231517,-2.97440515961066,-2.97197195623666,
-2.96974617394638,-2.96664295867037,-2.95854620163059,-2.90788557194195,
-2.86114835624393,-2.8254480425375,-2.81731534880772,-2.81255495389357,
-2.80835334038212,-2.80308756264278,-2.79484657498922,-2.7314242037378,
-2.68239056820158,-2.65822699640528,-2.65335651752462,-2.65063132008687,
-2.64826865929297,-2.64523384456385,-2.64019035151028,-2.60169561165248,
-2.54520155261438,-2.50365827903236,-2.49520284548529,-2.49037227682619,
-2.48617819428788,-2.48101160443384,-2.47309697379004,-2.4310204446325,
-2.36735883503205,-2.34643030917835,-2.33811003920562,-2.33187146730801,
-2.32886388262667,-2.32650810661212,-2.32372833246878,-2.31874591420167,
-2.29551083041115,-2.28868716086997,-2.20576401138959,-2.17929626884315,
-2.17186382105886,-2.167256605541,-2.16302247569691,-2.15757147253651,-2.14574457603877,
-2.06746694291484,-2.03050865497506,-2.01293960044915,-2.00831633811327,
-2.00564515046474,-2.00327137529979,-2.00009250817752,-1.99293723153902,
-1.96140636985788,-1.88905560082353,-1.85817426367366,-1.85005470192525,
-1.84529711113054,-1.84151527335835,-1.83644369989881,-1.82685128082296,
-1.7617196743932,-1.69540592252158,-1.68785209541015,-1.6848358925001,-1.68263233707729,
-1.68017540007131,-1.67652964620229,-1.6664120220225,-1.59884968159553,
-1.53751150784998,-1.52928601230348,-1.52402473995314,-1.51982331107646,
-1.51505946926798,-1.50691176652551,-1.4709780109223,-1.42361220764589,
-1.37378757915261,-1.36941396256219),.UNSPECIFIED.);
#1399=B_SPLINE_CURVE_WITH_KNOTS('',3,(#36321,#36322,#36323,#36324,#36325,
#36326,#36327,#36328,#36329,#36330,#36331,#36332,#36333,#36334,#36335,#36336,
#36337,#36338,#36339,#36340,#36341,#36342,#36343,#36344,#36345,#36346,#36347,
#36348,#36349,#36350,#36351,#36352,#36353,#36354,#36355,#36356,#36357,#36358,
#36359,#36360,#36361,#36362,#36363,#36364,#36365,#36366,#36367,#36368,#36369,
#36370,#36371,#36372,#36373,#36374,#36375,#36376,#36377,#36378,#36379,#36380,
#36381,#36382,#36383,#36384,#36385,#36386,#36387,#36388,#36389,#36390,#36391,
#36392),.UNSPECIFIED.,.F.,.F.,(4,2,2,2,2,2,2,2,2,2,2,2,2,2,2,2,2,2,2,2,
2,2,2,2,2,2,2,2,2,2,2,2,2,2,2,4),(-0.662425644205117,-0.636646086239023,
-0.586200282206748,-0.57809957168942,-0.574994362812132,-0.572767059893278,
-0.570331983817414,-0.566799550956724,-0.557482745293484,-0.543383347437845,
-0.441878150370085,-0.42305186539602,-0.416238118177119,-0.412210432428839,
-0.407967288359352,-0.40237409530578,-0.39041027985277,-0.374215799653739,
-0.330748238142239,-0.271760255898399,-0.257447218428823,-0.253141796922812,
-0.250539963589588,-0.248141685587373,-0.244808513593056,-0.237056905795168,
-0.197264095533609,-0.158093467926337,-0.105173906541785,-0.0969374812351964,
-0.0916714046660101,-0.0874674846711437,-0.0827022211851563,-0.077743904539085,
-0.0702532742700582,-0.000951723655427596),.UNSPECIFIED.);
#1400=B_SPLINE_CURVE_WITH_KNOTS('',3,(#36393,#36394,#36395,#36396,#36397,
#36398,#36399,#36400,#36401,#36402,#36403,#36404,#36405,#36406,#36407,#36408,
#36409,#36410,#36411,#36412,#36413,#36414,#36415,#36416,#36417,#36418,#36419,
#36420,#36421,#36422,#36423,#36424,#36425,#36426,#36427,#36428,#36429,#36430,
#36431,#36432,#36433,#36434,#36435,#36436,#36437,#36438,#36439,#36440,#36441,
#36442,#36443,#36444,#36445,#36446,#36447,#36448,#36449,#36450,#36451,#36452,
#36453,#36454,#36455,#36456,#36457,#36458,#36459,#36460,#36461,#36462,#36463,
#36464,#36465,#36466,#36467,#36468,#36469,#36470,#36471,#36472,#36473,#36474,
#36475,#36476,#36477,#36478,#36479,#36480,#36481,#36482,#36483,#36484,#36485,
#36486,#36487,#36488,#36489,#36490,#36491,#36492,#36493,#36494,#36495,#36496,
#36497,#36498,#36499,#36500,#36501,#36502,#36503,#36504,#36505,#36506,#36507,
#36508,#36509,#36510,#36511,#36512,#36513,#36514,#36515,#36516,#36517,#36518,
#36519,#36520,#36521,#36522,#36523,#36524,#36525,#36526,#36527,#36528,#36529,
#36530,#36531,#36532,#36533,#36534,#36535,#36536,#36537,#36538,#36539,#36540,
#36541,#36542,#36543,#36544,#36545,#36546),.UNSPECIFIED.,.F.,.F.,(4,2,2,
2,2,2,2,2,2,2,2,2,2,2,2,2,2,2,2,2,2,2,2,2,2,2,2,2,2,2,2,2,2,2,2,2,2,2,2,
2,2,2,2,2,2,2,2,2,2,2,2,2,2,2,2,2,2,2,2,2,2,2,2,2,2,2,2,2,2,2,2,2,2,2,2,
2,4),(-4.06102231635032,-3.99984654277032,-3.99488213931563,-3.99179793324655,
-3.98893724184584,-3.98658502286122,-3.98367140336896,-3.97808606014687,
-3.93457442605208,-3.92520848652895,-3.87174543846425,-3.84056175286585,
-3.83301976862949,-3.82825225104584,-3.82404958784693,-3.81878938121044,
-3.81057046516069,-3.74643132923399,-3.68145184229221,-3.67155023920359,
-3.66789780401313,-3.66543884569562,-3.66323530268854,-3.66022135328246,
-3.65268451295887,-3.58709723877599,-3.54210005530019,-3.52556699324923,
-3.51330699947153,-3.50771586185343,-3.50347336616354,-3.49944560441746,
-3.49263008229106,-3.4737883170242,-3.37226339002447,-3.35815990962468,
-3.34884202964806,-3.34530955014946,-3.3428745726869,-3.34064745450078,
-3.33754265381698,-3.32944370831833,-3.27907667702283,-3.23215156020394,
-3.19637915159503,-3.18823862251983,-3.18347458235237,-3.17927027819029,
-3.1740017811646,-3.16575769674041,-3.10235625132791,-3.05358296288273,
-3.02918520800431,-3.02430005090086,-3.02157058657536,-3.01920674510929,
-3.01617344194689,-3.0111385788302,-2.9747265282584,-2.95834211199055,-2.95366994721698,
-2.90039135989145,-2.88217927767047,-2.86897325352961,-2.86321400268094,
-2.85894452956393,-2.85441982913439,-2.84737646240552,-2.82683952173272,
-2.72733600554875,-2.71330887148643,-2.70402772734729,-2.70050019797248,
-2.69806578875981,-2.69583691796467,-2.69272669724805,-2.69249692795472),
 .UNSPECIFIED.);
#1401=B_SPLINE_CURVE_WITH_KNOTS('',3,(#36552,#36553,#36554,#36555,#36556,
#36557,#36558,#36559,#36560,#36561,#36562,#36563,#36564,#36565,#36566,#36567,
#36568,#36569,#36570,#36571,#36572,#36573,#36574,#36575,#36576,#36577,#36578,
#36579,#36580,#36581,#36582,#36583,#36584,#36585,#36586,#36587,#36588,#36589,
#36590,#36591,#36592,#36593,#36594,#36595,#36596,#36597,#36598,#36599,#36600,
#36601,#36602,#36603,#36604,#36605,#36606,#36607,#36608,#36609,#36610,#36611,
#36612,#36613,#36614,#36615,#36616,#36617,#36618,#36619,#36620,#36621,#36622,
#36623,#36624,#36625,#36626,#36627,#36628,#36629,#36630,#36631,#36632,#36633,
#36634,#36635,#36636,#36637,#36638,#36639,#36640,#36641,#36642,#36643,#36644,
#36645,#36646,#36647,#36648,#36649,#36650,#36651,#36652,#36653,#36654,#36655,
#36656,#36657,#36658,#36659,#36660,#36661,#36662,#36663,#36664,#36665,#36666,
#36667,#36668,#36669,#36670,#36671,#36672,#36673,#36674,#36675,#36676,#36677,
#36678,#36679,#36680,#36681,#36682,#36683,#36684,#36685,#36686,#36687,#36688,
#36689,#36690,#36691,#36692,#36693,#36694,#36695,#36696,#36697,#36698,#36699,
#36700,#36701,#36702,#36703,#36704,#36705,#36706,#36707,#36708,#36709,#36710,
#36711,#36712,#36713,#36714,#36715,#36716,#36717,#36718,#36719,#36720,#36721,
#36722,#36723,#36724,#36725),.UNSPECIFIED.,.F.,.F.,(4,2,2,2,2,2,2,2,2,2,
2,2,2,2,2,2,2,2,2,2,2,2,2,2,2,2,2,2,2,2,2,2,2,2,2,2,2,2,2,2,2,2,2,2,2,2,
2,2,2,2,2,2,2,2,2,2,2,2,2,2,2,2,2,2,2,2,2,2,2,2,2,2,2,2,2,2,2,2,2,2,2,2,
2,2,2,2,4),(-1.37005450945405,-1.34532621637229,-1.33713923164383,-1.33232026557117,
-1.32812570734539,-1.32294498136244,-1.31281765532065,-1.29987401033403,
-1.26928992458156,-1.20206482037715,-1.17821101179695,-1.17319296306083,
-1.17040532583634,-1.1680505098258,-1.16505391182974,-1.15887071436178,
-1.15064570957225,-1.13007348947339,-1.08598777703611,-1.02457146896735,
-1.01630014534599,-1.01102529844781,-1.00682303191568,-1.00206892750175,
-0.993964483367067,-0.958713306787006,-0.880707316432008,-0.855908346951102,
-0.851282959328518,-0.848340825524222,-0.845988681119941,-0.843155996676435,
-0.837782093555426,-0.800253821588666,-0.708523382461591,-0.695465084735774,
-0.690164237118537,-0.68623233293887,-0.68193198504365,-0.675979463883206,
-0.6616016853154,-0.595660687726437,-0.538046690996075,-0.530068087303279,
-0.526981782969047,-0.524760459911294,-0.522323132495924,-0.518772896389182,
-0.509324672644679,-0.494952274417858,-0.443322279105811,-0.379613187328578,
-0.37137298922778,-0.366107520218591,-0.361906058200078,-0.361830426505256,
-0.361734239613267,-0.361644584105557,-0.361561007518534,-0.361483088629685,
-0.361410435510148,-0.3613426834948,-0.361279493610346,-0.361220550913095,
-0.361165562721758,-0.356243218535335,-0.347125963575631,-0.33567329088123,
-0.310169957347652,-0.266182492209392,-0.215863696728321,-0.207763295774833,
-0.204659574677154,-0.202433693118009,-0.200000665598389,-0.196472178444829,
-0.187171611170168,-0.17310276781771,-0.0897815607022127,-0.0611334789419045,
-0.0495574015475814,-0.0441528060359751,-0.0399254794858704,-0.0359973851921187,
-0.0314509504551579,-0.024966113326458,-0.000950797002019388),
 .UNSPECIFIED.);
#1402=B_SPLINE_CURVE_WITH_KNOTS('',3,(#36726,#36727,#36728,#36729,#36730,
#36731,#36732,#36733,#36734,#36735,#36736,#36737,#36738,#36739,#36740,#36741,
#36742,#36743,#36744,#36745,#36746,#36747,#36748,#36749,#36750,#36751,#36752,
#36753,#36754,#36755,#36756,#36757,#36758,#36759,#36760,#36761,#36762,#36763,
#36764,#36765,#36766,#36767,#36768,#36769,#36770,#36771,#36772,#36773,#36774,
#36775,#36776,#36777,#36778,#36779,#36780,#36781,#36782,#36783,#36784,#36785,
#36786,#36787,#36788,#36789,#36790,#36791,#36792,#36793,#36794,#36795,#36796,
#36797,#36798,#36799,#36800,#36801),.UNSPECIFIED.,.F.,.F.,(4,2,2,2,2,2,
2,2,2,2,2,2,2,2,2,2,2,2,2,2,2,2,2,2,2,2,2,2,2,2,2,2,2,2,2,2,2,4),(-4.06037931501153,
-4.03713134392637,-3.95731390874865,-3.94945838041092,-3.94349344013245,
-3.9405402969288,-3.93841537819424,-3.93568880182403,-3.93093836106775,
-3.91118179479392,-3.82613353629426,-3.80372395300647,-3.79324505698843,
-3.78478041867085,-3.78003159381997,-3.77625268497845,-3.7713815870264,
-3.76296258787298,-3.72614114840973,-3.65737449341879,-3.62584161603421,
-3.620647892452,-3.61785373164648,-3.61550001578828,-3.61251323535657,-3.60773872180304,
-3.57984380918808,-3.55519470999195,-3.51532795491119,-3.48592089729895,
-3.47331143608953,-3.46339031266757,-3.45825191932105,-3.45406054465984,
-3.44921054563837,-3.44088548311329,-3.40558404251273,-3.39960000691215),
 .UNSPECIFIED.);
#1403=B_SPLINE_CURVE_WITH_KNOTS('',3,(#36802,#36803,#36804,#36805,#36806,
#36807,#36808,#36809,#36810,#36811,#36812,#36813,#36814,#36815,#36816,#36817,
#36818,#36819,#36820,#36821,#36822,#36823,#36824,#36825,#36826,#36827,#36828,
#36829,#36830,#36831,#36832,#36833,#36834,#36835,#36836,#36837,#36838,#36839,
#36840,#36841,#36842,#36843,#36844,#36845,#36846,#36847,#36848,#36849,#36850,
#36851,#36852,#36853,#36854,#36855,#36856,#36857,#36858,#36859,#36860,#36861,
#36862,#36863,#36864,#36865,#36866,#36867,#36868,#36869,#36870,#36871,#36872,
#36873,#36874,#36875,#36876,#36877,#36878,#36879,#36880,#36881,#36882,#36883,
#36884,#36885,#36886,#36887,#36888,#36889,#36890,#36891,#36892,#36893,#36894,
#36895,#36896,#36897,#36898,#36899,#36900,#36901,#36902,#36903,#36904,#36905,
#36906,#36907,#36908,#36909,#36910,#36911,#36912,#36913,#36914,#36915,#36916,
#36917,#36918,#36919,#36920,#36921,#36922,#36923,#36924,#36925,#36926,#36927,
#36928,#36929,#36930,#36931,#36932,#36933,#36934,#36935,#36936,#36937,#36938,
#36939,#36940,#36941,#36942,#36943,#36944,#36945,#36946,#36947,#36948,#36949,
#36950,#36951,#36952,#36953,#36954,#36955,#36956,#36957,#36958,#36959,#36960,
#36961,#36962,#36963,#36964,#36965,#36966,#36967,#36968,#36969,#36970,#36971,
#36972,#36973,#36974,#36975,#36976,#36977,#36978,#36979,#36980,#36981,#36982,
#36983,#36984,#36985,#36986,#36987,#36988,#36989,#36990,#36991,#36992,#36993,
#36994,#36995,#36996,#36997,#36998,#36999,#37000,#37001,#37002,#37003,#37004,
#37005,#37006,#37007,#37008,#37009),.UNSPECIFIED.,.F.,.F.,(4,2,2,2,2,2,
2,2,2,2,2,2,2,2,2,2,2,2,2,2,2,2,2,2,2,2,2,2,2,2,2,2,2,2,2,2,2,2,2,2,2,2,
2,2,2,2,2,2,2,2,2,2,2,2,2,2,2,2,2,2,2,2,2,2,2,2,2,2,2,2,2,2,2,2,2,2,2,2,
2,2,2,2,2,2,2,2,2,2,2,2,2,2,2,2,2,2,2,2,2,2,2,2,2,4),(-2.69249692795472,
-2.68459093233267,-2.63515909771338,-2.58837220213187,-2.55164942171319,
-2.54344969242352,-2.53867206666938,-2.53446842243638,-2.52921744488154,
-2.52103332506659,-2.47126740043804,-2.40790937824799,-2.38423941725221,
-2.37939300265136,-2.37667154262279,-2.37430568066648,-2.37125843245205,
-2.36617702466281,-2.31773708286663,-2.25823142450575,-2.22833085242378,
-2.22060126670146,-2.2159262141567,-2.21170473055825,-2.20628298792448,
-2.19494346244823,-2.11223027743305,-2.07799843616651,-2.06658677552773,
-2.05863353468367,-2.05531486767034,-2.0529182867092,-2.05030892016354,
-2.04597247311814,-2.03138587281004,-2.00391643861213,-1.972801849453,-1.91378450770349,
-1.90249031972551,-1.89635132693382,-1.89205608642049,-1.88765032697998,
-1.8811732125416,-1.86328866805201,-1.83588055387273,-1.77991740534245,
-1.74064312546832,-1.73558407782977,-1.7325432628246,-1.73017800414899,
-1.72745206350877,-1.72258550096841,-1.69855052211789,-1.63286880872178,
-1.58573116456729,-1.57762608914586,-1.57239888643464,-1.56819691607482,
-1.563402364319,-1.55512582175939,-1.51709213364138,-1.47273310345262,-1.42219760341824,
-1.41409521649996,-1.41098925293292,-1.40876138053682,-1.40632564906188,
-1.40279221090839,-1.39347243974879,-1.37936827826183,-1.27780829597349,
-1.25899990412908,-1.25218756727365,-1.24815943679293,-1.2439148938867,
-1.23831829085251,-1.22603497861429,-1.20946118366649,-1.16428836586456,
-1.09894566963456,-1.0913268228559,-1.08829826757187,-1.08609048620274,
-1.0836345049018,-1.07999975676878,-1.06997356739294,-1.00398933779334,
-0.940986605027574,-0.932742360363799,-0.927473285996992,-0.923268248386676,
-0.918503084326639,-0.910359918571633,-0.874565922479762,-0.827595996138246,
-0.777204540087443,-0.769102126788519,-0.765996400703885,-0.76376876082003,
-0.761333355968919,-0.757800512051332,-0.748483001564767,-0.73438287028182,
-0.661987786041638),.UNSPECIFIED.);
#1404=B_SPLINE_CURVE_WITH_KNOTS('',3,(#37014,#37015,#37016,#37017,#37018,
#37019,#37020,#37021,#37022,#37023,#37024,#37025,#37026,#37027,#37028,#37029,
#37030,#37031,#37032,#37033,#37034,#37035,#37036,#37037,#37038,#37039,#37040,
#37041,#37042,#37043,#37044,#37045,#37046,#37047,#37048,#37049,#37050,#37051,
#37052,#37053,#37054,#37055,#37056,#37057,#37058,#37059,#37060,#37061,#37062,
#37063,#37064,#37065,#37066,#37067,#37068,#37069,#37070,#37071,#37072,#37073,
#37074,#37075,#37076,#37077,#37078,#37079,#37080,#37081,#37082,#37083,#37084,
#37085,#37086,#37087,#37088,#37089,#37090,#37091,#37092,#37093,#37094,#37095,
#37096,#37097,#37098,#37099,#37100,#37101,#37102,#37103,#37104,#37105,#37106,
#37107,#37108,#37109,#37110,#37111,#37112,#37113,#37114,#37115,#37116,#37117,
#37118,#37119,#37120,#37121,#37122,#37123,#37124,#37125,#37126,#37127,#37128,
#37129,#37130,#37131,#37132,#37133,#37134,#37135,#37136,#37137,#37138,#37139,
#37140,#37141,#37142,#37143,#37144,#37145,#37146,#37147,#37148,#37149,#37150,
#37151,#37152,#37153,#37154,#37155,#37156,#37157,#37158,#37159,#37160,#37161,
#37162,#37163,#37164,#37165,#37166,#37167,#37168,#37169,#37170,#37171,#37172,
#37173,#37174,#37175,#37176,#37177,#37178,#37179,#37180,#37181,#37182,#37183,
#37184,#37185,#37186,#37187,#37188,#37189,#37190,#37191,#37192,#37193,#37194,
#37195,#37196,#37197,#37198,#37199,#37200,#37201,#37202,#37203,#37204,#37205,
#37206,#37207,#37208,#37209,#37210,#37211,#37212,#37213,#37214,#37215,#37216,
#37217,#37218,#37219,#37220,#37221),.UNSPECIFIED.,.F.,.F.,(4,2,2,2,2,2,
2,2,2,2,2,2,2,2,2,2,2,2,2,2,2,2,2,2,2,2,2,2,2,2,2,2,2,2,2,2,2,2,2,2,2,2,
2,2,2,2,2,2,2,2,2,2,2,2,2,2,2,2,2,2,2,2,2,2,2,2,2,2,2,2,2,2,2,2,2,2,2,2,
2,2,2,2,2,2,2,2,2,2,2,2,2,2,2,2,2,2,2,2,2,2,2,2,2,4),(-3.39962297301684,
-3.36254556477445,-3.32072301844083,-3.29347869106837,-3.27567482207821,
-3.26921424206043,-3.26481617221012,-3.26052572943178,-3.25438894653677,
-3.24308683145512,-3.17988975229796,-3.11904416732163,-3.10934880158451,
-3.10576352134441,-3.10331977385038,-3.10110645706124,-3.09804918492491,
-3.09024676665842,-3.02863069917918,-2.98106685553121,-2.95530619399558,
-2.94794130934146,-2.94334993988734,-2.9391128758676,-2.93363353432495,
-2.92164445962634,-2.84520787721698,-2.80708853396324,-2.79492639969945,
-2.78658405862663,-2.78320425941076,-2.78079964063717,-2.77853860760316,
-2.77463951255915,-2.76356827913853,-2.69781168589542,-2.65629825922005,
-2.63260298758734,-2.62544214508508,-2.62089517099366,-2.61664187847665,
-2.61105926946479,-2.59849230856507,-2.53879210225177,-2.48827303273349,
-2.47406131856074,-2.46469268210081,-2.4611548230828,-2.45872051950451,
-2.45649758938201,-2.45340338861596,-2.44536640765803,-2.39011735306177,
-2.33813149686875,-2.32016913092668,-2.30710450494831,-2.30137332323,-2.29711195103899,
-2.29258406501828,-2.28551135490787,-2.26475221618176,-2.16555217997405,
-2.15154194960709,-2.14227117344821,-2.13874741981798,-2.13631559133994,
-2.13408914718258,-2.13098249433349,-2.12285760583724,-2.0733265984331,
-2.03143661235886,-1.99089206067141,-1.98227443814986,-1.97735798574691,
-1.97358860900375,-1.96870232246343,-1.9599853945579,-1.91229942031345,
-1.83963590909024,-1.82215253682837,-1.81753690586894,-1.81486762544469,
-1.81249379048798,-1.80931246762411,-1.80214201042114,-1.77047150897854,
-1.6974605967261,-1.66729892104302,-1.65924545584733,-1.65450269862606,
-1.65071954550933,-1.64562927190657,-1.63594431095098,-1.57391579865678,
-1.50419093890524,-1.49689546053836,-1.49396117962422,-1.49156066965804,
-1.48902238128798,-1.48499923819309,-1.47180573113252,-1.4488109685451,
-1.37859646924867,-1.37005450945405),.UNSPECIFIED.);
#1405=B_SPLINE_CURVE_WITH_KNOTS('',3,(#37223,#37224,#37225,#37226,#37227,
#37228,#37229,#37230,#37231,#37232,#37233,#37234,#37235,#37236,#37237,#37238,
#37239,#37240,#37241,#37242,#37243,#37244,#37245,#37246,#37247,#37248,#37249,
#37250,#37251,#37252,#37253,#37254,#37255,#37256,#37257,#37258,#37259,#37260,
#37261,#37262,#37263,#37264,#37265,#37266,#37267,#37268,#37269,#37270,#37271,
#37272,#37273,#37274,#37275,#37276,#37277,#37278,#37279,#37280,#37281,#37282,
#37283,#37284,#37285,#37286,#37287,#37288,#37289,#37290,#37291,#37292,#37293,
#37294),.UNSPECIFIED.,.F.,.F.,(4,2,2,2,2,2,2,2,2,2,2,2,2,2,2,2,2,2,2,2,
2,2,2,2,2,2,2,2,2,2,2,2,2,2,2,4),(-0.661987786041638,-0.632897110421259,
-0.614040566443078,-0.607221985882824,-0.603192984919947,-0.598949576198417,
-0.593357919662498,-0.581099672443385,-0.564569101935066,-0.519590495412795,
-0.453965140633778,-0.446340790788293,-0.443324194282382,-0.441119588982708,
-0.438660474599158,-0.435009603795102,-0.424865358513279,-0.356883746135923,
-0.296098466928258,-0.287829692657471,-0.282553534244782,-0.278348307112415,
-0.273780766042135,-0.266116711546224,-0.256841741124321,-0.23804840711835,
-0.191699409280118,-0.131992292795311,-0.124097183296083,-0.121022524607124,
-0.118803138273764,-0.116360268149262,-0.112788916626733,-0.103206866529573,
-0.0885601570869462,-0.000952451209969257),.UNSPECIFIED.);
#1406=B_SPLINE_CURVE_WITH_KNOTS('',3,(#37295,#37296,#37297,#37298,#37299,
#37300,#37301,#37302,#37303,#37304,#37305,#37306,#37307,#37308,#37309,#37310,
#37311,#37312,#37313,#37314,#37315,#37316,#37317,#37318,#37319,#37320,#37321,
#37322,#37323,#37324,#37325,#37326,#37327,#37328,#37329,#37330,#37331,#37332,
#37333,#37334,#37335,#37336,#37337,#37338,#37339,#37340,#37341,#37342,#37343,
#37344,#37345,#37346,#37347,#37348,#37349,#37350,#37351,#37352,#37353,#37354,
#37355,#37356,#37357,#37358,#37359,#37360,#37361,#37362,#37363,#37364,#37365,
#37366,#37367,#37368,#37369,#37370,#37371,#37372,#37373,#37374,#37375,#37376,
#37377,#37378,#37379,#37380,#37381,#37382,#37383,#37384,#37385,#37386,#37387,
#37388,#37389,#37390,#37391,#37392,#37393,#37394,#37395,#37396,#37397,#37398,
#37399,#37400,#37401,#37402,#37403,#37404,#37405,#37406,#37407,#37408,#37409,
#37410,#37411,#37412,#37413,#37414,#37415,#37416,#37417,#37418,#37419,#37420,
#37421,#37422,#37423,#37424,#37425,#37426,#37427,#37428,#37429,#37430,#37431,
#37432,#37433,#37434,#37435,#37436,#37437,#37438,#37439,#37440,#37441,#37442,
#37443,#37444,#37445,#37446,#37447,#37448,#37449,#37450,#37451,#37452,#37453,
#37454,#37455,#37456,#37457,#37458,#37459,#37460,#37461,#37462,#37463,#37464,
#37465,#37466,#37467,#37468,#37469,#37470,#37471,#37472,#37473,#37474,#37475,
#37476,#37477,#37478,#37479,#37480),.UNSPECIFIED.,.F.,.F.,(4,2,2,2,2,2,
2,2,2,2,2,2,2,2,2,2,2,2,2,2,2,2,2,2,2,2,2,2,2,2,2,2,2,2,2,2,2,2,2,2,2,2,
2,2,2,2,2,2,2,2,2,2,2,2,2,2,2,2,2,2,2,2,2,2,2,2,2,2,2,2,2,2,2,2,2,2,2,2,
2,2,2,2,2,2,2,2,2,2,2,2,2,2,4),(-4.06207904828509,-4.04335695901034,-4.03155435033365,
-4.02608365069201,-4.0219218175068,-4.01791141510869,-4.01394354042528,
-4.00850443728747,-3.99463044250151,-3.96608070517844,-3.89310104584232,
-3.86601034442442,-3.86099291220808,-3.85823514776986,-3.85587573543404,
-3.85283451797909,-3.84788198942486,-3.81491326836232,-3.75421374358963,
-3.72578939275626,-3.71346186154221,-3.70379230963457,-3.69873314731702,
-3.69869522502636,-3.6986546351422,-3.6986111838906,-3.69856466246732,-3.69851484612974,
-3.69846149306318,-3.69840434232486,-3.69834311325685,-3.69827750334002,
-3.69820718652685,-3.69813181158868,-3.6980510004978,-3.69796434609788,
-3.69787140995314,-3.69781505718549,-3.69773644016462,-3.69353198144047,
-3.68825632802986,-3.67998736883403,-3.61926074070865,-3.55119032798046,
-3.54104165664174,-3.53739052654311,-3.5349316449013,-3.53272755204159,
-3.52971206670863,-3.52209023410478,-3.45649531650488,-3.41155530731917,
-3.39503398588419,-3.38278039276131,-3.37719003027038,-3.37294725561798,
-3.36891858385026,-3.36209993976592,-3.34323928535951,-3.24172331990386,
-3.22761900245592,-3.21830043576989,-3.2147676086336,-3.21233236397536,
-3.21010497941178,-3.20699977860134,-3.19889957488055,-3.14856130035586,
-3.10160667699447,-3.06582130039698,-3.05767929049224,-3.05291458603546,
-3.04870981787668,-3.04344090148969,-3.03519647853824,-2.97208043733708,
-2.90614951617144,-2.89612661681516,-2.89249240376657,-2.890036610716,-2.88782885383535,
-2.88480017315056,-2.87718009769879,-2.81192046776632,-2.76674133957567,
-2.75016616702003,-2.73788108055799,-2.73228419398127,-2.72803963516158,
-2.72401162364716,-2.71719986457004,-2.69839559582656,-2.69307182648613),
 .UNSPECIFIED.);
#1407=B_SPLINE_CURVE_WITH_KNOTS('',3,(#37486,#37487,#37488,#37489,#37490,
#37491,#37492,#37493,#37494,#37495,#37496,#37497,#37498,#37499,#37500,#37501,
#37502,#37503,#37504,#37505,#37506,#37507,#37508,#37509,#37510,#37511,#37512,
#37513,#37514,#37515,#37516,#37517,#37518,#37519,#37520,#37521,#37522,#37523,
#37524,#37525,#37526,#37527,#37528,#37529,#37530,#37531,#37532,#37533,#37534,
#37535,#37536,#37537,#37538,#37539,#37540,#37541,#37542,#37543,#37544,#37545,
#37546,#37547,#37548,#37549,#37550,#37551,#37552,#37553,#37554,#37555,#37556,
#37557,#37558,#37559,#37560,#37561,#37562,#37563,#37564,#37565,#37566,#37567,
#37568,#37569,#37570,#37571,#37572,#37573,#37574,#37575,#37576,#37577,#37578,
#37579,#37580,#37581,#37582,#37583,#37584,#37585,#37586,#37587,#37588,#37589,
#37590,#37591,#37592,#37593,#37594,#37595,#37596,#37597,#37598,#37599,#37600,
#37601,#37602,#37603,#37604,#37605,#37606,#37607,#37608,#37609,#37610,#37611,
#37612,#37613,#37614,#37615,#37616,#37617,#37618,#37619,#37620,#37621,#37622,
#37623,#37624,#37625,#37626,#37627,#37628,#37629,#37630,#37631,#37632,#37633,
#37634,#37635,#37636,#37637,#37638,#37639,#37640,#37641,#37642,#37643,#37644,
#37645),.UNSPECIFIED.,.F.,.F.,(4,2,2,2,2,2,2,2,2,2,2,2,2,2,2,2,2,2,2,2,
2,2,2,2,2,2,2,2,2,2,2,2,2,2,2,2,2,2,2,2,2,2,2,2,2,2,2,2,2,2,2,2,2,2,2,2,
2,2,2,2,2,2,2,2,2,2,2,2,2,2,2,2,2,2,2,2,2,2,2,4),(-1.36964948262408,-1.36420575719923,
-1.31373938642615,-1.30563991170215,-1.30253617806612,-1.3003101957542,
-1.29787695125363,-1.29434797180143,-1.28504508540802,-1.27097183769727,
-1.17013647399185,-1.15074707674252,-1.14385753627168,-1.13936834407756,
-1.13508656652235,-1.12923869397388,-1.11549534952302,-1.09629792665995,
-1.04003613625122,-1.02265040999473,-1.00463911117486,-0.985775164097792,
-0.981099564622399,-0.97838992926173,-0.976262099322461,-0.973284046195613,
-0.967194734440265,-0.917806706620069,-0.83639379839076,-0.826054390504639,
-0.820765916607833,-0.816837263675266,-0.812534679784094,-0.806568342231466,
-0.79210328442518,-0.751715343780525,-0.692487899331927,-0.664393789784042,
-0.659610476428317,-0.656620885469368,-0.654266748829769,-0.651474190879136,
-0.646288952339892,-0.615000597564471,-0.55000447140555,-0.509556781388679,
-0.500943832934489,-0.496028426132366,-0.491880314755915,-0.486837199474777,
-0.47737899579729,-0.465508878397657,-0.438625116846288,-0.396105043731741,
-0.346586726813181,-0.338492542657269,-0.335387574328687,-0.333161556135635,
-0.330778111812376,-0.32736466708586,-0.323429038475711,-0.316314861802805,
-0.299669014160669,-0.263766348410505,-0.193081405809607,-0.180731695711628,
-0.175186914976504,-0.170939079395929,-0.166375158177965,-0.159138933429679,
-0.134712397102432,-0.0911359770498033,-0.0296845051681231,-0.0174708888496529,
-0.0134213869570827,-0.0108774332789702,-0.00864748008808993,-0.0062496972863311,
-0.00349027148950385,-0.000951110743857238),.UNSPECIFIED.);
#1408=B_SPLINE_CURVE_WITH_KNOTS('',3,(#37646,#37647,#37648,#37649,#37650,
#37651,#37652,#37653,#37654,#37655,#37656,#37657,#37658,#37659,#37660,#37661,
#37662,#37663,#37664,#37665,#37666,#37667,#37668,#37669,#37670,#37671,#37672,
#37673,#37674,#37675,#37676,#37677,#37678,#37679,#37680,#37681,#37682,#37683,
#37684,#37685,#37686,#37687,#37688,#37689,#37690,#37691,#37692,#37693,#37694,
#37695,#37696,#37697,#37698,#37699,#37700,#37701,#37702,#37703,#37704,#37705,
#37706,#37707,#37708,#37709,#37710,#37711,#37712,#37713,#37714,#37715,#37716,
#37717,#37718,#37719),.UNSPECIFIED.,.F.,.F.,(4,2,2,2,2,2,2,2,2,2,2,2,2,
2,2,2,2,2,2,2,2,2,2,2,2,2,2,2,2,2,2,2,2,2,2,2,4),(-4.0605476020252,-4.04893185698267,
-4.00169615318516,-3.94952623524974,-3.9315311539863,-3.91844928136004,
-3.91271617726025,-3.90845552214372,-3.90447533819932,-3.89789429569454,
-3.88064323577898,-3.80375160388145,-3.75755716514169,-3.75361179825645,
-3.75018921449901,-3.74781264486562,-3.74559021929055,-3.74249657970057,
-3.73446780727046,-3.67905536969102,-3.62721013703199,-3.60927676923934,
-3.59622905890309,-3.59050169194357,-3.58624178192483,-3.58171417015119,
-3.57463922166177,-3.5538326711896,-3.45471519262012,-3.44071084546643,
-3.43144356007159,-3.42792086920845,-3.42548969043545,-3.42326377419266,
-3.42015777027404,-3.41203389864517,-3.39962297301684),.UNSPECIFIED.);
#1409=B_SPLINE_CURVE_WITH_KNOTS('',3,(#37720,#37721,#37722,#37723,#37724,
#37725,#37726,#37727,#37728,#37729,#37730,#37731,#37732,#37733,#37734,#37735,
#37736,#37737,#37738,#37739,#37740,#37741,#37742,#37743,#37744,#37745,#37746,
#37747,#37748,#37749,#37750,#37751,#37752,#37753,#37754,#37755,#37756,#37757,
#37758,#37759,#37760,#37761,#37762,#37763,#37764,#37765,#37766,#37767,#37768,
#37769,#37770,#37771,#37772,#37773,#37774,#37775,#37776,#37777,#37778,#37779,
#37780,#37781,#37782,#37783,#37784,#37785,#37786,#37787,#37788,#37789,#37790,
#37791,#37792,#37793,#37794,#37795,#37796,#37797,#37798,#37799,#37800,#37801,
#37802,#37803,#37804,#37805,#37806,#37807,#37808,#37809,#37810,#37811,#37812,
#37813,#37814,#37815,#37816,#37817,#37818,#37819,#37820,#37821,#37822,#37823,
#37824,#37825,#37826,#37827,#37828,#37829,#37830,#37831,#37832,#37833,#37834,
#37835,#37836,#37837,#37838,#37839,#37840,#37841,#37842,#37843,#37844,#37845,
#37846,#37847,#37848,#37849,#37850,#37851,#37852,#37853,#37854,#37855,#37856,
#37857,#37858,#37859,#37860,#37861,#37862,#37863,#37864,#37865,#37866,#37867,
#37868,#37869,#37870,#37871,#37872,#37873,#37874,#37875,#37876,#37877,#37878,
#37879,#37880,#37881,#37882,#37883,#37884,#37885,#37886,#37887,#37888,#37889,
#37890,#37891,#37892,#37893,#37894,#37895,#37896,#37897,#37898,#37899,#37900,
#37901,#37902,#37903,#37904,#37905,#37906,#37907,#37908,#37909,#37910,#37911,
#37912,#37913,#37914,#37915,#37916,#37917,#37918,#37919,#37920,#37921,#37922,
#37923),.UNSPECIFIED.,.F.,.F.,(4,2,2,2,2,2,2,2,2,2,2,2,2,2,2,2,2,2,2,2,
2,2,2,2,2,2,2,2,2,2,2,2,2,2,2,2,2,2,2,2,2,2,2,2,2,2,2,2,2,2,2,2,2,2,2,2,
2,2,2,2,2,2,2,2,2,2,2,2,2,2,2,2,2,2,2,2,2,2,2,2,2,2,2,2,2,2,2,2,2,2,2,2,
2,2,2,2,2,2,2,2,2,4),(-2.69307182648613,-2.59678002806464,-2.58266946313718,
-2.57334725562269,-2.569813366031,-2.56737748934965,-2.56514960677407,-2.56204381643266,
-2.55394285519653,-2.50340127643883,-2.45901947268785,-2.42106724034895,
-2.41279522962788,-2.4080015048615,-2.40379918536693,-2.39857014609783,
-2.39045944742972,-2.34317483864599,-2.27756504992639,-2.26146548893328,
-2.25119836077135,-2.24752990330896,-2.24506662511959,-2.24286418087539,
-2.23985801201697,-2.2323725839028,-2.16521383732554,-2.10113978677428,
-2.09137795350005,-2.08626839051568,-2.08207360121999,-2.07718914135381,
-2.06872832706745,-2.03135729068771,-1.98690299309149,-1.93631034627506,
-1.92820778362807,-1.92510170193445,-1.92287373204588,-1.92043787912758,
-1.91690424010372,-1.90758379683909,-1.8934784932247,-1.79190099462884,
-1.77310207273381,-1.7662908676212,-1.76226282620248,-1.75801795483589,
-1.75242020759388,-1.74013145100486,-1.72354836545171,-1.67833437320218,
-1.6130483248699,-1.60542581298646,-1.60239655728856,-1.60018853168595,
-1.59773259794555,-1.59409846804345,-1.58407745912395,-1.51818340250931,
-1.45507731043981,-1.44683253627665,-1.44156317159162,-1.43735793293797,
-1.43259257388242,-1.42444915684274,-1.38865558763836,-1.34168918208293,
-1.29128717680384,-1.28318446727812,-1.28007860696762,-1.27785086561257,
-1.27541534378155,-1.27188232012847,-1.26256427773527,-1.24846329069005,
-1.14696760288368,-1.12811438028997,-1.12129606883338,-1.11726699197672,
-1.1130233325632,-1.10743105848492,-1.09517027589864,-1.07863550441089,
-1.0336391276528,-0.968034913835258,-0.960432226511016,-0.957406528672747,
-0.955199571846554,-0.952742997986923,-0.949104779338261,-0.939052522610395,
-0.872628682698347,-0.810114881309919,-0.801868716541581,-0.796599263253016,
-0.792394463622042,-0.787630147865629,-0.77948987582087,-0.743735562380239,
-0.696869721637699,-0.662302199137575),.UNSPECIFIED.);
#1410=B_SPLINE_CURVE_WITH_KNOTS('',3,(#37928,#37929,#37930,#37931,#37932,
#37933,#37934,#37935,#37936,#37937,#37938,#37939,#37940,#37941,#37942,#37943,
#37944,#37945,#37946,#37947,#37948,#37949,#37950,#37951,#37952,#37953,#37954,
#37955,#37956,#37957,#37958,#37959,#37960,#37961,#37962,#37963,#37964,#37965,
#37966,#37967,#37968,#37969,#37970,#37971,#37972,#37973,#37974,#37975,#37976,
#37977,#37978,#37979,#37980,#37981,#37982,#37983,#37984,#37985,#37986,#37987,
#37988,#37989,#37990,#37991,#37992,#37993,#37994,#37995,#37996,#37997,#37998,
#37999,#38000,#38001,#38002,#38003,#38004,#38005,#38006,#38007,#38008,#38009,
#38010,#38011,#38012,#38013,#38014,#38015,#38016,#38017,#38018,#38019,#38020,
#38021,#38022,#38023,#38024,#38025,#38026,#38027,#38028,#38029,#38030,#38031,
#38032,#38033,#38034,#38035,#38036,#38037,#38038,#38039,#38040,#38041,#38042,
#38043,#38044,#38045,#38046,#38047,#38048,#38049,#38050,#38051,#38052,#38053,
#38054,#38055,#38056,#38057,#38058,#38059,#38060,#38061,#38062,#38063,#38064,
#38065,#38066,#38067,#38068,#38069,#38070,#38071,#38072,#38073,#38074,#38075,
#38076,#38077,#38078,#38079,#38080,#38081,#38082,#38083,#38084,#38085,#38086,
#38087,#38088,#38089,#38090,#38091,#38092,#38093,#38094,#38095,#38096,#38097,
#38098,#38099,#38100,#38101,#38102,#38103,#38104,#38105,#38106,#38107,#38108,
#38109,#38110,#38111,#38112,#38113,#38114,#38115,#38116,#38117,#38118,#38119,
#38120,#38121,#38122,#38123,#38124,#38125,#38126,#38127,#38128,#38129,#38130,
#38131,#38132,#38133,#38134,#38135,#38136,#38137,#38138,#38139),
 .UNSPECIFIED.,.F.,.F.,(4,2,2,2,2,2,2,2,2,2,2,2,2,2,2,2,2,2,2,2,2,2,2,2,
2,2,2,2,2,2,2,2,2,2,2,2,2,2,2,2,2,2,2,2,2,2,2,2,2,2,2,2,2,2,2,2,2,2,2,2,
2,2,2,2,2,2,2,2,2,2,2,2,2,2,2,2,2,2,2,2,2,2,2,2,2,2,2,2,2,2,2,2,2,2,2,2,
2,2,2,2,2,2,2,2,2,4),(-3.40003668949591,-3.3995458848467,-3.39528527315639,
-3.39075245278261,-3.38366004357326,-3.36273876788145,-3.26370009059015,
-3.24969421010163,-3.24042502501189,-3.23690103093427,-3.23446876842328,
-3.23224171261896,-3.22913392549394,-3.22100388915922,-3.17152048036574,
-3.12972758070188,-3.10242382901365,-3.08458973630762,-3.07812312006481,
-3.07372235011673,-3.06943035477724,-3.0632932414306,-3.05199544150283,
-2.99276379930217,-2.92819107591619,-2.91825389770932,-2.91463324653464,
-2.91218146623128,-2.90997339186421,-2.90693936812978,-2.89928021172689,
-2.8348787642099,-2.76792362484592,-2.75840448877016,-2.75334798478054,
-2.74919849754337,-2.74429279737192,-2.73572589250554,-2.69624422550159,
-2.63035838598052,-2.59882071801677,-2.59362532397676,-2.59083018590394,
-2.58847559960342,-2.5854876544926,-2.58071116661063,-2.55280070022704,
-2.52814702580471,-2.48826285625832,-2.45884746177747,-2.44623407221293,
-2.43630973931055,-2.4311695447881,-2.42697663228464,-2.42212477688976,
-2.41379633749472,-2.37847701853485,-2.30948681861726,-2.28715667571151,
-2.27422473114767,-2.27022972316123,-2.26769724939391,-2.26529218741406,
-2.26178534916213,-2.25326809873307,-2.15561271362714,-2.12050098085331,
-2.11240493649938,-2.10765232656296,-2.10344929146873,-2.0981706978445,
-2.08988794708771,-2.0305762787369,-1.96909202288149,-1.95270723530454,
-1.94817796170537,-1.94552735579411,-1.94314776525696,-1.93992813661065,
-1.93254383024007,-1.89893616989502,-1.80963848703443,-1.79427863373091,
-1.78799735292232,-1.78407026315965,-1.7797647421768,-1.77378570056311,
-1.75924615368478,-1.7147295415267,-1.66007153772704,-1.63164134458179,
-1.62684372795832,-1.62384954908988,-1.62149471665725,-1.61870477685022,
-1.61353332752726,-1.58264545923712,-1.53886030864452,-1.47750226953663,
-1.46926611785044,-1.46400169680184,-1.459800091111,-1.45503855337675,-1.44690104724737,
-1.41112960658645,-1.36964948262408),.UNSPECIFIED.);
#1411=B_SPLINE_CURVE_WITH_KNOTS('',3,(#38141,#38142,#38143,#38144,#38145,
#38146,#38147,#38148,#38149,#38150,#38151,#38152,#38153,#38154,#38155,#38156,
#38157,#38158,#38159,#38160,#38161,#38162,#38163,#38164,#38165,#38166,#38167,
#38168,#38169,#38170,#38171,#38172,#38173,#38174,#38175,#38176,#38177,#38178,
#38179,#38180,#38181,#38182,#38183,#38184,#38185,#38186,#38187,#38188,#38189,
#38190,#38191,#38192,#38193,#38194,#38195,#38196,#38197,#38198,#38199,#38200,
#38201,#38202,#38203,#38204,#38205,#38206,#38207,#38208,#38209,#38210,#38211,
#38212,#38213,#38214),.UNSPECIFIED.,.F.,.F.,(4,2,2,2,2,2,2,2,2,2,2,2,2,
2,2,2,2,2,2,2,2,2,2,2,2,2,2,2,2,2,2,2,2,2,2,2,4),(-0.662302199137575,-0.646338159767163,
-0.638237608602623,-0.635132282033017,-0.63290484978247,-0.630469579986745,
-0.626936779097043,-0.617618501748615,-0.603516436636057,-0.501959334207145,
-0.483168188665671,-0.476359077337931,-0.47233209144975,-0.468088199426295,
-0.462491519640081,-0.450204182259338,-0.433622399054046,-0.388406958720866,
-0.323067079767071,-0.315505862035146,-0.312487403021977,-0.310282438431202,
-0.307882418521396,-0.304354543721482,-0.300257642284619,-0.292722491547411,
-0.274652453728868,-0.183800054015231,-0.161638257143985,-0.154396326524713,
-0.149828921725321,-0.145577880217575,-0.139932183040148,-0.127371101476896,
-0.110307971961426,-0.0628349439114606,-0.000952237661129041),
 .UNSPECIFIED.);
#1412=B_SPLINE_CURVE_WITH_KNOTS('',3,(#38215,#38216,#38217,#38218,#38219,
#38220,#38221,#38222,#38223,#38224,#38225,#38226,#38227,#38228,#38229,#38230,
#38231,#38232,#38233,#38234,#38235,#38236,#38237,#38238,#38239,#38240,#38241,
#38242,#38243,#38244,#38245,#38246,#38247,#38248,#38249,#38250,#38251,#38252,
#38253,#38254,#38255,#38256,#38257,#38258,#38259,#38260,#38261,#38262,#38263,
#38264,#38265,#38266,#38267,#38268,#38269,#38270,#38271,#38272,#38273,#38274,
#38275,#38276,#38277,#38278,#38279,#38280,#38281,#38282,#38283,#38284,#38285,
#38286,#38287,#38288,#38289,#38290,#38291,#38292,#38293,#38294,#38295,#38296,
#38297,#38298,#38299,#38300,#38301,#38302,#38303,#38304,#38305,#38306,#38307,
#38308,#38309,#38310,#38311,#38312,#38313,#38314,#38315,#38316,#38317,#38318,
#38319,#38320,#38321,#38322,#38323,#38324,#38325,#38326,#38327,#38328,#38329,
#38330,#38331,#38332,#38333,#38334,#38335,#38336,#38337,#38338,#38339,#38340,
#38341,#38342,#38343,#38344,#38345,#38346,#38347,#38348,#38349,#38350,#38351,
#38352,#38353,#38354,#38355,#38356,#38357,#38358,#38359,#38360,#38361,#38362,
#38363,#38364,#38365,#38366),.UNSPECIFIED.,.F.,.F.,(4,2,2,2,2,2,2,2,2,2,
2,2,2,2,2,2,2,2,2,2,2,2,2,2,2,2,2,2,2,2,2,2,2,2,2,2,2,2,2,2,2,2,2,2,2,2,
2,2,2,2,2,2,2,2,2,2,2,2,2,2,2,2,2,2,2,2,2,2,2,2,2,2,2,2,2,4),(-4.06185261524568,
-4.05708505957242,-4.05285548409638,-4.05048801339724,-4.04823074791862,
-4.04563329060578,-4.04134734048006,-4.02716467492896,-3.93797472700334,
-3.9019124917828,-3.89375527840498,-3.88898819998056,-3.88478527056778,
-3.87952386631328,-3.87130138877667,-3.8091722107146,-3.7650108488942,-3.74487644788151,
-3.73676904555361,-3.73245803578029,-3.72964128156967,-3.72701440386011,
-3.72474687911975,-3.72171150001949,-3.71666839048799,-3.67821588273949,
-3.63749521856553,-3.58627285361472,-3.57407082775049,-3.56849012007095,
-3.56424904401895,-3.56021778922336,-3.55338446127771,-3.53441611565386,
-3.43304323888024,-3.41894522220792,-3.40962994361556,-3.40609779174135,
-3.40366283211739,-3.40143556427606,-3.39833033781048,-3.39022866052372,
-3.34004250345076,-3.29298931647877,-3.25716937035706,-3.24902573699305,
-3.24426094051343,-3.24005660939871,-3.23478892769658,-3.22654778293989,
-3.16433734774897,-3.09757330317497,-3.08750079468223,-3.08385986502947,
-3.0814028314911,-3.07919651201705,-3.07617304807871,-3.06858515033518,
-3.00281982176751,-2.95797595212944,-2.94147464976351,-2.9292320842113,
-2.92364319671007,-2.9194001018845,-2.91537005439773,-2.90854645208976,
-2.8896550141435,-2.78815743119671,-2.77405220546355,-2.76473281612469,
-2.76119953177653,-2.75876392605747,-2.75653617463109,-2.75343041447236,
-2.7453283942911,-2.69294542034399),.UNSPECIFIED.);
#1413=B_SPLINE_CURVE_WITH_KNOTS('',3,(#38372,#38373,#38374,#38375,#38376,
#38377,#38378,#38379,#38380,#38381,#38382,#38383,#38384,#38385,#38386,#38387,
#38388,#38389,#38390,#38391,#38392,#38393,#38394,#38395,#38396,#38397,#38398,
#38399,#38400,#38401,#38402,#38403,#38404,#38405,#38406,#38407,#38408,#38409,
#38410,#38411,#38412,#38413,#38414,#38415,#38416,#38417,#38418,#38419,#38420,
#38421,#38422,#38423,#38424,#38425,#38426,#38427,#38428,#38429,#38430,#38431,
#38432,#38433,#38434,#38435,#38436,#38437,#38438,#38439,#38440,#38441,#38442,
#38443,#38444,#38445,#38446,#38447,#38448,#38449,#38450,#38451,#38452,#38453,
#38454,#38455,#38456,#38457,#38458,#38459,#38460,#38461,#38462,#38463,#38464,
#38465,#38466,#38467,#38468,#38469,#38470,#38471,#38472,#38473,#38474,#38475,
#38476,#38477,#38478,#38479,#38480,#38481,#38482,#38483,#38484,#38485,#38486,
#38487,#38488,#38489,#38490,#38491,#38492,#38493,#38494,#38495,#38496,#38497,
#38498,#38499,#38500,#38501,#38502,#38503,#38504,#38505,#38506,#38507,#38508,
#38509,#38510,#38511,#38512,#38513,#38514,#38515,#38516,#38517,#38518,#38519,
#38520,#38521,#38522,#38523,#38524,#38525,#38526,#38527,#38528,#38529,#38530,
#38531,#38532,#38533,#38534,#38535,#38536,#38537,#38538,#38539,#38540,#38541),
 .UNSPECIFIED.,.F.,.F.,(4,2,2,2,2,2,2,2,2,2,2,2,2,2,2,2,2,2,2,2,2,2,2,2,
2,2,2,2,2,2,2,2,2,2,2,2,2,2,2,2,2,2,2,2,2,2,2,2,2,2,2,2,2,2,2,2,2,2,2,2,
2,2,2,2,2,2,2,2,2,2,2,2,2,2,2,2,2,2,2,2,2,2,2,2,4),(-1.36962177122299,-1.32182238407877,
-1.2850684154456,-1.2766479916492,-1.27177604658522,-1.2675856555344,-1.26247354222409,
-1.25268228975713,-1.18750292975858,-1.12163581844339,-1.11402897599387,
-1.11101678020998,-1.10881444934637,-1.10635682666759,-1.10270651555574,
-1.09255341807395,-1.02436884386449,-0.963808535367563,-0.955538417418492,
-0.950264073430916,-0.946062038647845,-0.941308016168192,-0.933203263951293,
-0.897942597175451,-0.821877560973487,-0.795334998583643,-0.790618255399449,
-0.787648544140803,-0.785295299188886,-0.782486233010396,-0.777224052104454,
-0.743663907147497,-0.674576387054659,-0.639984306066628,-0.631708228834379,
-0.626868871275764,-0.622675920731407,-0.61752189843231,-0.607526714675422,
-0.594797198581604,-0.564970564067933,-0.510393274605143,-0.47354531156842,
-0.468527411580614,-0.465500213898569,-0.463138548690593,-0.460408672452058,
-0.455515993119272,-0.430927490760664,-0.361423714917032,-0.318448951647306,
-0.310499590705437,-0.305322707088563,-0.301231227374083,-0.30105429487929,
-0.300902520899787,-0.300771061449599,-0.300656266565702,-0.30055532642677,
-0.300466037865446,-0.300386646236463,-0.300315734701143,-0.300252145090754,
-0.300194920288565,-0.300143261810963,-0.300096497688419,-0.299999268182783,
-0.299903724084309,-0.299809713955632,-0.299717096139761,-0.294358139630899,
-0.288464823804344,-0.278695201476487,-0.232408053373161,-0.185644132521259,
-0.167449926824457,-0.149619423537348,-0.144974576360588,-0.142298868733295,
-0.139926618290346,-0.136757270754286,-0.129653568615952,-0.0985749262887441,
-0.0571044553074189,-0.000952159825757125),.UNSPECIFIED.);
#1414=B_SPLINE_CURVE_WITH_KNOTS('',3,(#38542,#38543,#38544,#38545,#38546,
#38547,#38548,#38549,#38550,#38551,#38552,#38553,#38554,#38555,#38556,#38557,
#38558,#38559,#38560,#38561,#38562,#38563,#38564,#38565,#38566,#38567,#38568,
#38569,#38570,#38571,#38572,#38573,#38574,#38575,#38576,#38577,#38578,#38579,
#38580,#38581,#38582,#38583,#38584,#38585,#38586,#38587,#38588,#38589,#38590,
#38591,#38592,#38593,#38594,#38595,#38596,#38597,#38598,#38599,#38600,#38601,
#38602,#38603,#38604,#38605,#38606,#38607,#38608,#38609,#38610,#38611,#38612,
#38613,#38614,#38615,#38616,#38617,#38618,#38619,#38620,#38621),
 .UNSPECIFIED.,.F.,.F.,(4,2,2,2,2,2,2,2,2,2,2,2,2,2,2,2,2,2,2,2,2,2,2,2,
2,2,2,2,2,2,2,2,2,2,2,2,2,2,2,4),(-4.06117045119648,-4.05432040146447,-4.04820732500887,
-4.04405540252273,-4.04004268008692,-4.03552792660978,-4.02851751083157,
-4.00815949447454,-3.91997642877976,-3.89864540712678,-3.89021892851807,
-3.88391880491664,-3.88089961445068,-3.87854339025131,-3.87577320438849,
-3.87083180211565,-3.8482717028776,-3.79138267103709,-3.75309717597981,
-3.73812484563565,-3.7302141293804,-3.7234391480088,-3.71902805471729,-3.71489490299815,
-3.70930676310575,-3.69671262406839,-3.63713135686164,-3.58652338952762,
-3.57229722549555,-3.5629210126716,-3.55938155573755,-3.55694654878127,
-3.55472329147679,-3.55162904644104,-3.54359479034715,-3.48756188402932,
-3.43613156191842,-3.41827444551578,-3.40526776157587,-3.40003668949591),
 .UNSPECIFIED.);
#1415=B_SPLINE_CURVE_WITH_KNOTS('',3,(#38622,#38623,#38624,#38625,#38626,
#38627,#38628,#38629,#38630,#38631,#38632,#38633,#38634,#38635,#38636,#38637,
#38638,#38639,#38640,#38641,#38642,#38643,#38644,#38645,#38646,#38647,#38648,
#38649,#38650,#38651,#38652,#38653,#38654,#38655,#38656,#38657,#38658,#38659,
#38660,#38661,#38662,#38663,#38664,#38665,#38666,#38667,#38668,#38669,#38670,
#38671,#38672,#38673,#38674,#38675,#38676,#38677,#38678,#38679,#38680,#38681,
#38682,#38683,#38684,#38685,#38686,#38687,#38688,#38689,#38690,#38691,#38692,
#38693,#38694,#38695,#38696,#38697,#38698,#38699,#38700,#38701,#38702,#38703,
#38704,#38705,#38706,#38707,#38708,#38709,#38710,#38711,#38712,#38713,#38714,
#38715,#38716,#38717,#38718,#38719,#38720,#38721,#38722,#38723,#38724,#38725,
#38726,#38727,#38728,#38729,#38730,#38731,#38732,#38733,#38734,#38735,#38736,
#38737,#38738,#38739,#38740,#38741,#38742,#38743,#38744,#38745,#38746,#38747,
#38748,#38749,#38750,#38751,#38752,#38753,#38754,#38755,#38756,#38757,#38758,
#38759,#38760,#38761,#38762,#38763,#38764,#38765,#38766,#38767,#38768,#38769,
#38770,#38771,#38772,#38773,#38774,#38775,#38776,#38777,#38778,#38779,#38780,
#38781,#38782,#38783,#38784,#38785,#38786,#38787,#38788,#38789,#38790,#38791,
#38792,#38793,#38794,#38795,#38796,#38797,#38798,#38799,#38800,#38801,#38802,
#38803,#38804,#38805,#38806,#38807,#38808,#38809,#38810,#38811,#38812,#38813,
#38814,#38815,#38816,#38817,#38818,#38819,#38820,#38821,#38822,#38823,#38824,
#38825,#38826,#38827,#38828,#38829,#38830,#38831,#38832,#38833),
 .UNSPECIFIED.,.F.,.F.,(4,2,2,2,2,2,2,2,2,2,2,2,2,2,2,2,2,2,2,2,2,2,2,2,
2,2,2,2,2,2,2,2,2,2,2,2,2,2,2,2,2,2,2,2,2,2,2,2,2,2,2,2,2,2,2,2,2,2,2,2,
2,2,2,2,2,2,2,2,2,2,2,2,2,2,2,2,2,2,2,2,2,2,2,2,2,2,2,2,2,2,2,2,2,2,2,2,
2,2,2,2,2,2,2,2,2,4),(-2.69294542034399,-2.6928928505863,-2.63882773344267,
-2.62046805321308,-2.60717972549637,-2.60140556837181,-2.59713292897633,
-2.5926121473132,-2.58558988602039,-2.56522502157542,-2.48174327500305,
-2.44571414558974,-2.44037515616131,-2.43754814321433,-2.43519327223398,
-2.43223823580005,-2.42757530572775,-2.40206255512511,-2.33428226751476,
-2.30522795517801,-2.292715775396,-2.2828527242158,-2.27772241827823,-2.27352666660196,
-2.26865922006533,-2.26027326705638,-2.22412977976389,-2.15563720238791,
-2.13358950146674,-2.12076754597086,-2.11678269506573,-2.11425104527045,
-2.11184193069927,-2.1083216841153,-2.10165930919544,-2.03189129800188,
-1.9690142415646,-1.96076853474069,-1.95549855236157,-1.95129280698205,
-1.94652685895233,-1.9383823986052,-1.90258355541477,-1.85560889915667,
-1.80520447788957,-1.79710075146804,-1.79399451054906,-1.79176649850709,
-1.7893306834325,-1.78579723886,-1.77647811203658,-1.76237550650481,-1.66086984352645,
-1.64201247297892,-1.63519307551586,-1.63116346129063,-1.62691931175715,
-1.62132651941167,-1.60906512556103,-1.59252987716967,-1.54753501965914,
-1.48191211377001,-1.47430916637186,-1.47128321412731,-1.46907601844971,
-1.46661911477013,-1.4629802977569,-1.45292568784383,-1.38647487275192,
-1.32397558480673,-1.31572756343887,-1.31045721288047,-1.3062518814333,
-1.30148716026879,-1.29334668752886,-1.25760066767841,-1.2107633559977,
-1.1601774920642,-1.15207589395443,-1.14897018257566,-1.14674247846021,
-1.1443069162732,-1.14077369925754,-1.13145437067886,-1.11735075537655,
-1.01578551736578,-0.996988724428408,-0.990178316015324,-0.98615075214909,
-0.981906388702902,-0.976309319099813,-0.964022082492951,-0.947441069525992,
-0.902232903132334,-0.83695398650396,-0.829332420207833,-0.826303532047379,
-0.824095771446446,-0.821640128979283,-0.818006424100635,-0.807986549320123,
-0.742099339856279,-0.679001869411645,-0.670758081219974,-0.665489345942252,
-0.662282742015645),.UNSPECIFIED.);
#1416=B_SPLINE_CURVE_WITH_KNOTS('',3,(#38838,#38839,#38840,#38841,#38842,
#38843,#38844,#38845,#38846,#38847,#38848,#38849,#38850,#38851,#38852,#38853,
#38854,#38855,#38856,#38857,#38858,#38859,#38860,#38861,#38862,#38863,#38864,
#38865,#38866,#38867,#38868,#38869,#38870,#38871,#38872,#38873,#38874,#38875,
#38876,#38877,#38878,#38879,#38880,#38881,#38882,#38883,#38884,#38885,#38886,
#38887,#38888,#38889,#38890,#38891,#38892,#38893,#38894,#38895,#38896,#38897,
#38898,#38899,#38900,#38901,#38902,#38903,#38904,#38905,#38906,#38907,#38908,
#38909,#38910,#38911,#38912,#38913,#38914,#38915,#38916,#38917,#38918,#38919,
#38920,#38921,#38922,#38923,#38924,#38925,#38926,#38927,#38928,#38929,#38930,
#38931,#38932,#38933,#38934,#38935,#38936,#38937,#38938,#38939,#38940,#38941,
#38942,#38943,#38944,#38945,#38946,#38947,#38948,#38949,#38950,#38951,#38952,
#38953,#38954,#38955,#38956,#38957,#38958,#38959,#38960,#38961,#38962,#38963,
#38964,#38965,#38966,#38967,#38968,#38969,#38970,#38971,#38972,#38973,#38974,
#38975,#38976,#38977,#38978,#38979,#38980,#38981,#38982,#38983,#38984,#38985,
#38986,#38987,#38988,#38989,#38990,#38991,#38992,#38993,#38994,#38995,#38996,
#38997,#38998,#38999,#39000,#39001,#39002,#39003,#39004,#39005,#39006,#39007,
#39008,#39009,#39010,#39011,#39012,#39013,#39014,#39015,#39016,#39017,#39018,
#39019,#39020,#39021,#39022,#39023,#39024,#39025,#39026,#39027,#39028,#39029,
#39030,#39031,#39032,#39033,#39034,#39035,#39036,#39037,#39038,#39039,#39040,
#39041,#39042,#39043,#39044,#39045,#39046,#39047,#39048,#39049,#39050,#39051,
#39052,#39053,#39054,#39055,#39056,#39057,#39058,#39059),.UNSPECIFIED.,
 .F.,.F.,(4,2,2,2,2,2,2,2,2,2,2,2,2,2,2,2,2,2,2,2,2,2,2,2,2,2,2,2,2,2,2,
2,2,2,2,2,2,2,2,2,2,2,2,2,2,2,2,2,2,2,2,2,2,2,2,2,2,2,2,2,2,2,2,2,2,2,2,
2,2,2,2,2,2,2,2,2,2,2,2,2,2,2,2,2,2,2,2,2,2,2,2,2,2,2,2,2,2,2,2,2,2,2,2,
2,2,2,2,2,2,2,4),(-3.3994167761936,-3.39442164906984,-3.38034416848886,
-3.37104051307309,-3.36751186976563,-3.36507907224068,-3.36285366078891,
-3.35975096200867,-3.35165554862964,-3.30100762950804,-3.25427519164643,
-3.21857971483864,-3.21044830756437,-3.20568869112948,-3.20148778011025,
-3.19622290320236,-3.1879833653753,-3.1246250833392,-3.07594174580726,-3.05142103747698,
-3.04653208060429,-3.04380315307592,-3.04144155771395,-3.03841353784895,
-3.03339243686023,-2.99626609088144,-2.93884108569202,-2.89687999990697,
-2.88840549223081,-2.88357130827243,-2.87937830325598,-2.87421842624741,
-2.86632422209368,-2.8248786322846,-2.76069798320331,-2.73968637964977,
-2.73134446192148,-2.72509350438527,-2.72208381098282,-2.71972824334746,
-2.71695089919474,-2.711978011135,-2.68889421130294,-2.68210448756076,-2.65873907925416,
-2.60216153431056,-2.5829077543951,-2.56913261967478,-2.56327947306876,
-2.55899681241839,-2.55450938046214,-2.54762794246094,-2.52829684464235,
-2.4435946728105,-2.41902560223549,-2.40522957091918,-2.40114204502221,
-2.39858947688626,-2.39619704579261,-2.39329511321307,-2.38589880449259,
-2.3149433806828,-2.25319040220295,-2.24410459153482,-2.23913933008357,
-2.23536589931028,-2.23052292613989,-2.22223111821802,-2.18743592920801,
-2.11829660317755,-2.08494018612046,-2.07968405892186,-2.07687622296797,
-2.0745228139862,-2.07155139976785,-2.06682923127756,-2.04025420278267,
-2.03098288674323,-1.95130234511404,-1.9276865466937,-1.92027949207753,
-1.91567792578148,-1.91144223800245,-1.90588624872804,-1.89381024758399,
-1.84364606886248,-1.80572011082791,-1.76320794821286,-1.75762814515457,
-1.75471648680764,-1.75236536664811,-1.74950556751446,-1.74400095954611,
-1.70003078407794,-1.62925045805596,-1.60538371161242,-1.59794881307469,
-1.59334125865426,-1.58910760413258,-1.58356525366598,-1.571563048529,-1.52202261712466,
-1.47429685932129,-1.44063945666054,-1.43566504155081,-1.43265060561563,
-1.43029030101327,-1.42755186631513,-1.42261945334926,-1.39725725750434,
-1.36962177122299),.UNSPECIFIED.);
#1417=B_SPLINE_CURVE_WITH_KNOTS('',3,(#39061,#39062,#39063,#39064,#39065,
#39066,#39067,#39068,#39069,#39070,#39071,#39072,#39073,#39074,#39075,#39076,
#39077,#39078,#39079,#39080,#39081,#39082,#39083,#39084,#39085,#39086,#39087,
#39088,#39089,#39090,#39091,#39092,#39093,#39094,#39095,#39096,#39097,#39098,
#39099,#39100,#39101,#39102,#39103,#39104,#39105,#39106,#39107,#39108,#39109,
#39110,#39111,#39112,#39113,#39114,#39115,#39116,#39117,#39118,#39119,#39120,
#39121,#39122,#39123,#39124,#39125,#39126,#39127,#39128,#39129,#39130,#39131,
#39132,#39133,#39134,#39135,#39136,#39137,#39138,#39139,#39140),
 .UNSPECIFIED.,.F.,.F.,(4,2,2,2,2,2,2,2,2,2,2,2,2,2,2,2,2,2,2,2,2,2,2,2,
2,2,2,2,2,2,2,2,2,2,2,2,2,2,2,4),(-0.662282742015645,-0.661284609116616,
-0.65651981822441,-0.648377370840048,-0.612588039983296,-0.565627149997621,
-0.515231285197535,-0.507129541221009,-0.504024051326852,-0.501796575742074,
-0.499361344563022,-0.495828742688839,-0.486511813576414,-0.472412512024089,
-0.370929012965544,-0.352077976412442,-0.345260469629144,-0.34123187182051,
-0.337073255615075,-0.331647011656286,-0.325655356851237,-0.315646278901475,
-0.26372876092633,-0.200490038387841,-0.186388137487069,-0.182106016680302,
-0.179509202537946,-0.177108491527682,-0.17376192644085,-0.165636438546779,
-0.153896725804903,-0.118005807928824,-0.048596137079172,-0.0297128719064544,
-0.0228966503970393,-0.0188682031481931,-0.0148170287410706,-0.0107010941196923,
-0.00592907222480298,-0.000951129530177771),.UNSPECIFIED.);
#1418=B_SPLINE_CURVE_WITH_KNOTS('',3,(#39141,#39142,#39143,#39144,#39145,
#39146,#39147,#39148,#39149,#39150,#39151,#39152,#39153,#39154,#39155,#39156,
#39157,#39158,#39159,#39160,#39161,#39162,#39163,#39164,#39165,#39166,#39167,
#39168,#39169,#39170,#39171,#39172,#39173,#39174,#39175,#39176,#39177,#39178,
#39179,#39180,#39181,#39182,#39183,#39184,#39185,#39186,#39187,#39188,#39189,
#39190,#39191,#39192,#39193,#39194,#39195,#39196,#39197,#39198,#39199,#39200,
#39201,#39202,#39203,#39204,#39205,#39206,#39207,#39208,#39209,#39210,#39211,
#39212,#39213,#39214,#39215,#39216,#39217,#39218,#39219,#39220,#39221,#39222,
#39223,#39224,#39225,#39226,#39227,#39228,#39229,#39230,#39231,#39232,#39233,
#39234,#39235,#39236,#39237,#39238,#39239,#39240,#39241,#39242,#39243,#39244,
#39245,#39246,#39247,#39248,#39249,#39250,#39251,#39252,#39253,#39254,#39255,
#39256,#39257,#39258,#39259,#39260,#39261,#39262,#39263,#39264,#39265,#39266,
#39267,#39268,#39269,#39270,#39271,#39272,#39273,#39274,#39275,#39276,#39277,
#39278,#39279,#39280,#39281,#39282,#39283,#39284,#39285,#39286,#39287,#39288,
#39289,#39290,#39291,#39292,#39293,#39294),.UNSPECIFIED.,.F.,.F.,(4,2,2,
2,2,2,2,2,2,2,2,2,2,2,2,2,2,2,2,2,2,2,2,2,2,2,2,2,2,2,2,2,2,2,2,2,2,2,2,
2,2,2,2,2,2,2,2,2,2,2,2,2,2,2,2,2,2,2,2,2,2,2,2,2,2,2,2,2,2,2,2,2,2,2,2,
2,4),(-4.06127466498446,-4.04616684401087,-3.97047454395635,-3.92646874790103,
-3.92095911744303,-3.91809662598807,-3.91574320000556,-3.91282842395056,
-3.90724180230987,-3.86413442467703,-3.77982965630429,-3.77006485643972,
-3.76417165612202,-3.75889284262175,-3.75879592892169,-3.75869792845998,
-3.758654605828,-3.75860797743966,-3.75855767045854,-3.75850325201899,-3.75844421720845,
-3.75837997161098,-3.75435690992838,-3.74963528309801,-3.74169176430377,
-3.71296338618885,-3.63854116380484,-3.60362267173816,-3.59831544269605,
-3.59549528337143,-3.59314029656281,-3.59017777113489,-3.58548961148469,
-3.55943638261745,-3.47326493020888,-3.44636455324335,-3.43888884462978,
-3.43426964561768,-3.4300343110146,-3.42459533483568,-3.41284898050076,
-3.33373121445113,-3.29730506176416,-3.28546030294407,-3.27728027233682,
-3.27392436257466,-3.27152169357215,-3.26924992532191,-3.26530565289905,
-3.25392851460564,-3.18841759114668,-3.12778225177244,-3.118141613754,-3.11305756918907,
-3.10927184186816,-3.1045164260944,-3.09641799433392,-3.06572996883521,
-3.06035001451274,-2.99145755281917,-2.96916959972103,-2.96049080410266,
-2.95404345584398,-2.95099413708534,-2.94863328774185,-2.94587944319076,
-2.94101734350758,-2.91971424325242,-2.85128718887266,-2.80376883539671,
-2.79505251290309,-2.79016335172717,-2.78639023046136,-2.78146670796622,
-2.77283088029294,-2.73203329550979,-2.69212785249457),.UNSPECIFIED.);
#1419=B_SPLINE_CURVE_WITH_KNOTS('',3,(#39300,#39301,#39302,#39303,#39304,
#39305,#39306,#39307,#39308,#39309,#39310,#39311,#39312,#39313,#39314,#39315,
#39316,#39317,#39318,#39319,#39320,#39321,#39322,#39323,#39324,#39325,#39326,
#39327,#39328,#39329,#39330,#39331,#39332,#39333,#39334,#39335,#39336,#39337,
#39338,#39339,#39340,#39341,#39342,#39343,#39344,#39345,#39346,#39347,#39348,
#39349,#39350,#39351,#39352,#39353,#39354,#39355,#39356,#39357,#39358,#39359,
#39360,#39361,#39362,#39363,#39364,#39365,#39366,#39367,#39368,#39369,#39370,
#39371,#39372,#39373,#39374,#39375,#39376,#39377,#39378,#39379,#39380,#39381,
#39382,#39383,#39384,#39385,#39386,#39387,#39388,#39389,#39390,#39391,#39392,
#39393,#39394,#39395,#39396,#39397,#39398,#39399,#39400,#39401,#39402,#39403,
#39404,#39405,#39406,#39407,#39408,#39409,#39410,#39411,#39412,#39413,#39414,
#39415,#39416,#39417,#39418,#39419,#39420,#39421,#39422,#39423,#39424,#39425,
#39426,#39427,#39428,#39429,#39430,#39431,#39432,#39433,#39434,#39435,#39436,
#39437,#39438,#39439,#39440,#39441),.UNSPECIFIED.,.F.,.F.,(4,2,2,2,2,2,
2,2,2,2,2,2,2,2,2,2,2,2,2,2,2,2,2,2,2,2,2,2,2,2,2,2,2,2,2,2,2,2,2,2,2,2,
2,2,2,2,2,2,2,2,2,2,2,2,2,2,2,2,2,2,2,2,2,2,2,2,2,2,2,2,4),(-1.36995468810373,
-1.34524430130784,-1.30338042112438,-1.25385409901805,-1.24572391017952,
-1.24261634850845,-1.24038956640011,-1.23795771106143,-1.2344345040908,
-1.22516837960924,-1.21116959496001,-1.11217702182287,-1.09127186798715,
-1.08418208159927,-1.07965014794946,-1.07538981055964,-1.06966744815885,
-1.05665596467422,-1.03878767222862,-0.987297698675521,-0.931292979870644,
-0.92325532097066,-0.920160706027039,-0.917937472027335,-0.915502804041723,
-0.911964383517623,-0.902593932000619,-0.888380813959507,-0.837850616048762,
-0.778210893282045,-0.765644694319501,-0.760061724111958,-0.755807864754708,
-0.751260004683357,-0.744097182129189,-0.720390424635643,-0.678844055005731,
-0.613122878452704,-0.601988986900391,-0.59808069870273,-0.595817581080475,
-0.593413586299495,-0.590039224463397,-0.581732840347395,-0.569642362709692,
-0.531908990025203,-0.454926668424072,-0.442986909024379,-0.437515928056792,
-0.433279479621659,-0.42868294282424,-0.421296924545675,-0.395322131364976,
-0.347091034762141,-0.286363529461873,-0.278517086967082,-0.275452013475459,
-0.273236391064645,-0.270794024627438,-0.267423759764045,-0.258770103617987,
-0.245807996088087,-0.203212882845492,-0.133253784209077,-0.120872881083716,
-0.115322564978666,-0.111073861709748,-0.106512302107184,-0.0992868843734209,
-0.0749678591588764,-0.000952473517230175),.UNSPECIFIED.);
#1420=B_SPLINE_CURVE_WITH_KNOTS('',3,(#39442,#39443,#39444,#39445,#39446,
#39447,#39448,#39449,#39450,#39451,#39452,#39453,#39454,#39455,#39456,#39457,
#39458,#39459,#39460,#39461,#39462,#39463,#39464,#39465,#39466,#39467,#39468,
#39469,#39470,#39471,#39472,#39473,#39474,#39475,#39476,#39477,#39478,#39479,
#39480,#39481,#39482,#39483,#39484,#39485,#39486,#39487,#39488,#39489,#39490,
#39491,#39492,#39493,#39494,#39495,#39496,#39497,#39498,#39499,#39500,#39501,
#39502,#39503,#39504,#39505,#39506,#39507,#39508,#39509,#39510,#39511,#39512,
#39513),.UNSPECIFIED.,.F.,.F.,(4,2,2,2,2,2,2,2,2,2,2,2,2,2,2,2,2,2,2,2,
2,2,2,2,2,2,2,2,2,2,2,2,2,2,2,4),(-4.06017442960531,-4.0198490772075,-4.01576004008251,
-4.01303507719492,-4.01080972136062,-4.00845177097557,-4.00540465693538,
-4.00042736929215,-3.96665499648457,-3.92853463158271,-3.88846571308708,
-3.86195146965499,-3.85451667113691,-3.8499100745933,-3.84567789720946,
-3.84023133589455,-3.82842189084888,-3.75004256126864,-3.71318209887599,
-3.70125809957024,-3.69309095727252,-3.68990865565758,-3.68747609677886,
-3.68525131261838,-3.68215002334286,-3.67406227250093,-3.62558125273539,
-3.56915683250162,-3.54993314420651,-3.53617517860012,-3.53032579293961,
-3.52604460119274,-3.52155755050054,-3.5146743720624,-3.49532315562753,
-3.3994167761936),.UNSPECIFIED.);
#1421=B_SPLINE_CURVE_WITH_KNOTS('',3,(#39514,#39515,#39516,#39517,#39518,
#39519,#39520,#39521,#39522,#39523,#39524,#39525,#39526,#39527,#39528,#39529,
#39530,#39531,#39532,#39533,#39534,#39535,#39536,#39537,#39538,#39539,#39540,
#39541,#39542,#39543,#39544,#39545,#39546,#39547,#39548,#39549,#39550,#39551,
#39552,#39553,#39554,#39555,#39556,#39557,#39558,#39559,#39560,#39561,#39562,
#39563,#39564,#39565,#39566,#39567,#39568,#39569,#39570,#39571,#39572,#39573,
#39574,#39575,#39576,#39577,#39578,#39579,#39580,#39581,#39582,#39583,#39584,
#39585,#39586,#39587,#39588,#39589,#39590,#39591,#39592,#39593,#39594,#39595,
#39596,#39597,#39598,#39599,#39600,#39601,#39602,#39603,#39604,#39605,#39606,
#39607,#39608,#39609,#39610,#39611,#39612,#39613,#39614,#39615,#39616,#39617,
#39618,#39619,#39620,#39621,#39622,#39623,#39624,#39625,#39626,#39627,#39628,
#39629,#39630,#39631,#39632,#39633,#39634,#39635,#39636,#39637,#39638,#39639,
#39640,#39641,#39642,#39643,#39644,#39645,#39646,#39647,#39648,#39649,#39650,
#39651,#39652,#39653,#39654,#39655,#39656,#39657,#39658,#39659,#39660,#39661,
#39662,#39663,#39664,#39665,#39666,#39667,#39668,#39669,#39670,#39671,#39672,
#39673,#39674,#39675,#39676,#39677,#39678,#39679,#39680,#39681,#39682,#39683,
#39684,#39685,#39686,#39687,#39688,#39689,#39690,#39691,#39692,#39693,#39694,
#39695,#39696,#39697,#39698,#39699,#39700,#39701,#39702,#39703,#39704,#39705,
#39706,#39707,#39708,#39709,#39710,#39711,#39712,#39713,#39714,#39715,#39716,
#39717,#39718,#39719,#39720,#39721,#39722,#39723,#39724,#39725,#39726,#39727,
#39728,#39729,#39730,#39731,#39732,#39733),.UNSPECIFIED.,.F.,.F.,(4,2,2,
2,2,2,2,2,2,2,2,2,2,2,2,2,2,2,2,2,2,2,2,2,2,2,2,2,2,2,2,2,2,2,2,2,2,2,2,
2,2,2,2,2,2,2,2,2,2,2,2,2,2,2,2,2,2,2,2,2,2,2,2,2,2,2,2,2,2,2,2,2,2,2,2,
2,2,2,2,2,2,2,2,2,2,2,2,2,2,2,2,2,2,2,2,2,2,2,2,2,2,2,2,2,2,2,2,2,2,4),
(-2.69212785249457,-2.66727989701356,-2.64616552319342,-2.63372095713774,
-2.62977944367602,-2.62725759520586,-2.62484259551211,-2.62185868194171,
-2.61450067773853,-2.54603231520456,-2.50284379339667,-2.47854511713085,
-2.47131710508253,-2.46675188238764,-2.46249832932244,-2.45693955784036,
-2.44453044219312,-2.37500383879394,-2.33825943763338,-2.31314383103301,
-2.30822044203222,-2.3054823403991,-2.30311924247648,-2.30004646120218,
-2.29498940071131,-2.25579361013186,-2.19982510615917,-2.17242202643007,
-2.15453852058383,-2.14806190019371,-2.14365648324377,-2.13936157699765,
-2.13322307101615,-2.12192964601337,-2.05693899247034,-2.03067445315504,
-1.99189091181378,-1.98683951417776,-1.98380104542996,-1.98143619355091,
-1.97870906071893,-1.97383643370548,-1.94968474053626,-1.9006716669888,
-1.83727555436632,-1.82903016521644,-1.8237605959357,-1.81955531407384,
-1.81479003463521,-1.80664707460547,-1.77086151125462,-1.72391719760335,
-1.67348284724176,-1.6653803786339,-1.66227453779059,-1.6600467921085,-1.65761124425224,
-1.65407814741565,-1.64475970803118,-1.63065794107718,-1.52914335636685,
-1.51030482618826,-1.50348854456057,-1.49945983912708,-1.49521596877495,
-1.48962240378856,-1.47735462145513,-1.46080764957954,-1.41575566780296,
-1.350236371517,-1.34262848338344,-1.33960189497708,-1.33739470476851,-1.33493837029946,
-1.33130136381787,-1.32125791442368,-1.25498117251233,-1.19230467414953,
-1.18406010712324,-1.17879111925732,-1.17458633706122,-1.16982166203015,
-1.16167983015368,-1.12590100516029,-1.07896896824866,-1.02853118431582,
-1.0204297653349,-1.0173243075528,-1.01509683178548,-1.0126615735444,-1.00912888745757,
-0.99981147730133,-0.985711220417281,-0.884203988641315,-0.865371640796756,
-0.858556726509011,-0.854528609945143,-0.850285200428662,-0.844691974525185,
-0.832423830999553,-0.815875640377666,-0.770814398639095,-0.705325544789426,
-0.697717230149788,-0.694690778709533,-0.69248379655605,-0.690027823549075,
-0.686391575204932,-0.676351637263147,-0.661760008706104),.UNSPECIFIED.);
#1422=B_SPLINE_CURVE_WITH_KNOTS('',3,(#39738,#39739,#39740,#39741,#39742,
#39743,#39744,#39745,#39746,#39747,#39748,#39749,#39750,#39751,#39752,#39753,
#39754,#39755,#39756,#39757,#39758,#39759,#39760,#39761,#39762,#39763,#39764,
#39765,#39766,#39767,#39768,#39769,#39770,#39771,#39772,#39773,#39774,#39775,
#39776,#39777,#39778,#39779,#39780,#39781,#39782,#39783,#39784,#39785,#39786,
#39787,#39788,#39789,#39790,#39791,#39792,#39793,#39794,#39795,#39796,#39797,
#39798,#39799,#39800,#39801,#39802,#39803,#39804,#39805,#39806,#39807,#39808,
#39809,#39810,#39811,#39812,#39813,#39814,#39815,#39816,#39817,#39818,#39819,
#39820,#39821,#39822,#39823,#39824,#39825,#39826,#39827,#39828,#39829,#39830,
#39831,#39832,#39833,#39834,#39835,#39836,#39837,#39838,#39839,#39840,#39841,
#39842,#39843,#39844,#39845,#39846,#39847,#39848,#39849,#39850,#39851,#39852,
#39853,#39854,#39855,#39856,#39857,#39858,#39859,#39860,#39861,#39862,#39863,
#39864,#39865,#39866,#39867,#39868,#39869,#39870,#39871,#39872,#39873,#39874,
#39875,#39876,#39877,#39878,#39879,#39880,#39881,#39882,#39883,#39884,#39885,
#39886,#39887,#39888,#39889,#39890,#39891,#39892,#39893,#39894,#39895,#39896,
#39897,#39898,#39899,#39900,#39901,#39902,#39903,#39904,#39905,#39906,#39907,
#39908,#39909,#39910,#39911,#39912,#39913,#39914,#39915,#39916,#39917,#39918,
#39919,#39920,#39921,#39922,#39923,#39924,#39925,#39926,#39927,#39928,#39929,
#39930,#39931,#39932,#39933,#39934,#39935,#39936,#39937,#39938,#39939,#39940,
#39941,#39942,#39943,#39944,#39945,#39946,#39947,#39948,#39949,#39950,#39951,
#39952,#39953,#39954,#39955,#39956,#39957),.UNSPECIFIED.,.F.,.F.,(4,2,2,
2,2,2,2,2,2,2,2,2,2,2,2,2,2,2,2,2,2,2,2,2,2,2,2,2,2,2,2,2,2,2,2,2,2,2,2,
2,2,2,2,2,2,2,2,2,2,2,2,2,2,2,2,2,2,2,2,2,2,2,2,2,2,2,2,2,2,2,2,2,2,2,2,
2,2,2,2,2,2,2,2,2,2,2,2,2,2,2,2,2,2,2,2,2,2,2,2,2,2,2,2,2,2,2,2,2,2,4),
(-3.39979696556878,-3.37744498003102,-3.35861069348364,-3.34506488607214,
-3.33925101834471,-3.33497572703817,-3.33047659469462,-3.32353791987474,
-3.30377703941068,-3.20336296062979,-3.1893038016249,-3.1800090189603,-3.17648164754876,
-3.17404907872227,-3.17182346681411,-3.16871981388899,-3.16061696066295,
-3.10944787344756,-3.06308853098223,-3.02753177484141,-3.01940923573579,
-3.01465168317684,-3.01045070617049,-3.00518324573007,-2.99693477155237,
-2.93449580024307,-2.88962321048857,-2.87016843940872,-2.86224791829032,
-2.85624444755682,-2.85328359261279,-2.85115778200827,-2.84843645517322,
-2.84370964478586,-2.8242719558361,-2.7538353115502,-2.70624824039539,-2.6975353643801,
-2.69264991645845,-2.68888051255544,-2.68396308752625,-2.67534130214054,
-2.63471849325497,-2.56983245064334,-2.54870031757402,-2.54032646183851,
-2.5340569291915,-2.53104364118136,-2.52868785079088,-2.525913290932,-2.52095247404733,
-2.49804446124985,-2.49045724666118,-2.41808443213978,-2.3828173360825,
-2.37471294879723,-2.36995929428552,-2.36575767290137,-2.3604839659525,
-2.35221500590998,-2.29146659305402,-2.22340567794163,-2.21325993987489,
-2.209610785242,-2.20715353032138,-2.20495120965328,-2.20193864029987,-2.19440381423585,
-2.12792641458797,-2.06332607291784,-2.05355455227567,-2.0484466399312,
-2.04425662675977,-2.03938164796086,-2.03094725223126,-1.98767674593242,
-1.92449564771755,-1.91604688421022,-1.89350712134465,-1.88856683422172,
-1.88579692471071,-1.88344068060331,-1.88042116817684,-1.87411935219238,
-1.86569068148351,-1.84435244283121,-1.77833452202546,-1.73908965257323,
-1.73053662282668,-1.7256347024537,-1.72148600367427,-1.71642750066372,
-1.70689555623615,-1.63742854782449,-1.57574003668981,-1.56793526700877,
-1.56487709104276,-1.56266313280061,-1.56021867685184,-1.55663236314167,
-1.54693406861035,-1.48606811636443,-1.42291761599845,-1.41161389175017,
-1.40547567573514,-1.40118399664856,-1.39678445801982,-1.39032135314762,
-1.37250837721402,-1.36995468810373),.UNSPECIFIED.);
#1423=B_SPLINE_CURVE_WITH_KNOTS('',3,(#39959,#39960,#39961,#39962,#39963,
#39964,#39965,#39966,#39967,#39968,#39969,#39970,#39971,#39972,#39973,#39974,
#39975,#39976,#39977,#39978,#39979,#39980,#39981,#39982,#39983,#39984,#39985,
#39986,#39987,#39988,#39989,#39990,#39991,#39992,#39993,#39994,#39995,#39996,
#39997,#39998,#39999,#40000,#40001,#40002,#40003,#40004,#40005,#40006,#40007,
#40008,#40009,#40010,#40011,#40012,#40013,#40014,#40015,#40016,#40017,#40018,
#40019,#40020,#40021,#40022,#40023,#40024,#40025,#40026,#40027,#40028,#40029,
#40030,#40031,#40032),.UNSPECIFIED.,.F.,.F.,(4,2,2,2,2,2,2,2,2,2,2,2,2,
2,2,2,2,2,2,2,2,2,2,2,2,2,2,2,2,2,2,2,2,2,2,2,4),(-0.661760008706104,-0.610121130832886,
-0.547410337844604,-0.539167014544015,-0.533898736112226,-0.529694465651339,
-0.52493031223833,-0.516789226305753,-0.481010963551039,-0.434074418664113,
-0.383656778907406,-0.375556494041579,-0.372451430796078,-0.370224228012008,
-0.367789255423349,-0.36460524451549,-0.356427678910649,-0.344491835723892,
-0.30758588596065,-0.229322918807091,-0.217499950920666,-0.212047622492467,
-0.207811085975501,-0.2031998322688,-0.195757626531973,-0.169216353237172,
-0.127576692493981,-0.0880856711935334,-0.0775501452560537,-0.0561640576798613,
-0.0512972048177857,-0.0485427053965044,-0.0461826211105746,-0.0438770898741965,
-0.0408775438910002,-0.0361210025104908,-0.000950734522379934),
 .UNSPECIFIED.);
#1424=B_SPLINE_CURVE_WITH_KNOTS('',3,(#40033,#40034,#40035,#40036,#40037,
#40038,#40039,#40040,#40041,#40042,#40043,#40044,#40045,#40046,#40047,#40048,
#40049,#40050,#40051,#40052,#40053,#40054,#40055,#40056,#40057,#40058,#40059,
#40060,#40061,#40062,#40063,#40064,#40065,#40066,#40067,#40068,#40069,#40070,
#40071,#40072,#40073,#40074,#40075,#40076,#40077,#40078,#40079,#40080,#40081,
#40082,#40083,#40084,#40085,#40086,#40087,#40088,#40089,#40090,#40091,#40092,
#40093,#40094,#40095,#40096,#40097,#40098,#40099,#40100,#40101,#40102,#40103,
#40104,#40105,#40106,#40107,#40108,#40109,#40110,#40111,#40112,#40113,#40114,
#40115,#40116,#40117,#40118,#40119,#40120,#40121,#40122,#40123,#40124,#40125,
#40126,#40127,#40128,#40129,#40130,#40131,#40132,#40133,#40134,#40135,#40136,
#40137,#40138,#40139,#40140,#40141,#40142,#40143,#40144,#40145,#40146,#40147,
#40148,#40149,#40150,#40151,#40152,#40153,#40154,#40155,#40156,#40157,#40158,
#40159,#40160,#40161,#40162,#40163,#40164,#40165,#40166,#40167,#40168,#40169,
#40170,#40171,#40172,#40173,#40174,#40175,#40176,#40177),.UNSPECIFIED.,
 .F.,.F.,(4,3,3,3,3,3,3,3,3,3,3,3,3,3,3,3,3,3,3,3,3,3,3,3,3,3,3,3,3,3,3,
3,3,3,3,3,3,3,3,3,3,3,3,3,3,3,3,3,4),(122.522113490244,122.613744298623,
122.708839823948,122.80029837443,122.891723140004,122.983140229123,123.074575737944,
123.166108241455,123.257698561075,123.349426790597,123.374508501224,123.467603526403,
123.560572888272,123.653444189759,123.746248050553,123.839017024604,123.931775909089,
124.024549486236,124.117422017638,124.210346529202,124.303425262594,124.372359342951,
124.465454390665,124.558423775412,124.651295100083,124.744098984424,124.836867982237,
124.929626890668,125.022400491916,125.115273047508,125.208197583347,125.301276340902,
125.370210184679,125.46330507077,125.556274293555,125.649145456144,125.741949178877,
125.834718015426,125.927476763126,126.020250204364,126.113122602046,126.2060469809,
126.299125584598,126.368061026406,126.465860047437,126.558813461684,126.651680825063,
126.744477529307,126.759257110528),.UNSPECIFIED.);
#1425=B_SPLINE_CURVE_WITH_KNOTS('',3,(#40183,#40184,#40185,#40186,#40187,
#40188,#40189,#40190,#40191,#40192,#40193,#40194,#40195,#40196,#40197,#40198,
#40199,#40200,#40201,#40202,#40203,#40204,#40205,#40206,#40207,#40208,#40209,
#40210,#40211,#40212,#40213,#40214,#40215,#40216,#40217,#40218,#40219,#40220,
#40221,#40222,#40223,#40224,#40225,#40226,#40227,#40228,#40229,#40230,#40231,
#40232,#40233,#40234,#40235,#40236,#40237,#40238,#40239,#40240,#40241,#40242,
#40243,#40244,#40245,#40246,#40247,#40248,#40249,#40250,#40251,#40252,#40253,
#40254,#40255,#40256,#40257,#40258,#40259,#40260,#40261,#40262,#40263,#40264,
#40265,#40266,#40267,#40268,#40269,#40270,#40271,#40272,#40273,#40274,#40275,
#40276,#40277,#40278,#40279,#40280,#40281,#40282,#40283,#40284,#40285,#40286,
#40287,#40288,#40289,#40290,#40291,#40292,#40293,#40294,#40295,#40296,#40297,
#40298,#40299,#40300,#40301,#40302,#40303,#40304,#40305,#40306,#40307,#40308,
#40309,#40310,#40311,#40312,#40313,#40314,#40315,#40316,#40317,#40318,#40319,
#40320,#40321),.UNSPECIFIED.,.F.,.F.,(4,3,3,3,3,3,3,3,3,3,3,3,3,3,3,3,3,
3,3,3,3,3,3,3,3,3,3,3,3,3,3,3,3,3,3,3,3,3,3,3,3,3,3,3,3,3,4),(128.805298797437,
128.929991698155,129.054684598874,129.147795384353,129.240780462687,129.333667417213,
129.426486773064,129.519271140378,129.61204529876,129.704834012771,129.797721376801,
129.890660574789,129.98375360517,130.052535440601,130.1456368389,130.238612757127,
130.331490787099,130.424301604411,130.517077672376,130.60984377884,130.702624696804,
130.795504705468,130.888436781627,130.981523141936,131.050386282328,131.143399346805,
131.236286529022,131.329075539228,131.421797275338,131.514484251581,131.607161359868,
131.699853477369,131.792645539447,131.885490005879,131.97849021635,132.048237124056,
132.141489610871,132.234616088049,132.327643956439,132.420602734125,132.513525642518,
132.606437297571,132.699362299286,132.792382237166,132.885452744539,132.978671062894,
133.042160362488),.UNSPECIFIED.);
#1426=B_SPLINE_CURVE_WITH_KNOTS('',3,(#40322,#40323,#40324,#40325,#40326,
#40327,#40328,#40329,#40330,#40331,#40332,#40333,#40334,#40335,#40336,#40337,
#40338,#40339,#40340,#40341,#40342,#40343,#40344,#40345,#40346,#40347,#40348,
#40349,#40350,#40351,#40352,#40353,#40354,#40355,#40356,#40357,#40358,#40359,
#40360,#40361,#40362,#40363,#40364,#40365,#40366,#40367,#40368,#40369,#40370,
#40371,#40372,#40373,#40374,#40375,#40376,#40377,#40378,#40379,#40380,#40381,
#40382,#40383,#40384,#40385,#40386,#40387,#40388,#40389,#40390,#40391),
 .UNSPECIFIED.,.F.,.F.,(4,2,2,2,2,2,2,2,2,2,2,2,2,2,2,2,2,2,2,2,2,2,2,2,
2,2,2,2,2,2,2,2,2,2,4),(-4.06123088005783,-3.99915769086102,-3.99163726706931,
-3.9866691328777,-3.98189860315967,-3.97770198514831,-3.97246090317619,
-3.96429462822665,-3.91489664695743,-3.8740430317043,-3.82926394557993,
-3.82346359017865,-3.8204904331031,-3.81836400142996,-3.81565282686222,
-3.81097009832807,-3.79201981736089,-3.72967739114034,-3.69232097445996,
-3.67025118650308,-3.66342445538446,-3.65886388830599,-3.65461386369307,
-3.64905857058841,-3.63665255117785,-3.56678567827841,-3.52412808003807,
-3.51115468488872,-3.50239817690508,-3.49895195972588,-3.49653452214352,
-3.49428973781681,-3.49047539651302,-3.48002372339966,-3.39979696556878),
 .UNSPECIFIED.);
#1427=B_SPLINE_CURVE_WITH_KNOTS('',3,(#40393,#40394,#40395,#40396,#40397,
#40398,#40399,#40400,#40401,#40402,#40403,#40404,#40405,#40406,#40407,#40408,
#40409,#40410,#40411,#40412,#40413,#40414,#40415,#40416,#40417,#40418,#40419,
#40420,#40421,#40422,#40423,#40424,#40425,#40426,#40427,#40428,#40429,#40430,
#40431,#40432,#40433,#40434,#40435,#40436,#40437,#40438,#40439,#40440,#40441,
#40442,#40443,#40444,#40445,#40446,#40447,#40448,#40449,#40450,#40451,#40452,
#40453,#40454,#40455,#40456,#40457,#40458,#40459,#40460,#40461,#40462),
 .UNSPECIFIED.,.F.,.F.,(4,3,3,3,3,3,3,3,3,3,3,3,3,3,3,3,3,3,3,3,3,3,3,4),
(126.759257110528,126.852022037374,126.944782070836,127.037561992392,127.130443687958,
127.223382033601,127.316468841556,127.365911868133,127.459007116446,127.551976703792,
127.644848232775,127.737652323135,127.830421527947,127.923180644104,128.015954453555,
128.108827216787,128.201751960273,128.294830923321,128.363762709861,128.464552334364,
128.564983981233,128.665188037793,128.765060809243,128.805298796957),
 .UNSPECIFIED.);
#1428=B_SPLINE_CURVE_WITH_KNOTS('',3,(#40463,#40464,#40465,#40466,#40467,
#40468,#40469,#40470,#40471,#40472,#40473,#40474,#40475,#40476,#40477,#40478,
#40479,#40480,#40481,#40482,#40483,#40484,#40485,#40486,#40487,#40488,#40489,
#40490,#40491,#40492,#40493,#40494,#40495,#40496,#40497,#40498,#40499,#40500,
#40501,#40502,#40503,#40504,#40505,#40506,#40507,#40508,#40509,#40510,#40511,
#40512,#40513,#40514,#40515,#40516,#40517,#40518,#40519,#40520,#40521,#40522,
#40523,#40524,#40525,#40526,#40527,#40528,#40529,#40530,#40531,#40532,#40533,
#40534,#40535,#40536,#40537,#40538,#40539,#40540,#40541,#40542,#40543,#40544,
#40545,#40546,#40547,#40548,#40549,#40550,#40551,#40552,#40553,#40554,#40555,
#40556,#40557,#40558,#40559,#40560,#40561,#40562,#40563,#40564,#40565,#40566,
#40567,#40568,#40569,#40570,#40571,#40572,#40573,#40574,#40575,#40576,#40577,
#40578,#40579,#40580,#40581,#40582,#40583,#40584,#40585,#40586,#40587,#40588,
#40589,#40590,#40591,#40592,#40593,#40594,#40595,#40596,#40597,#40598,#40599,
#40600,#40601,#40602,#40603,#40604,#40605,#40606,#40607,#40608,#40609,#40610,
#40611,#40612,#40613,#40614,#40615,#40616),.UNSPECIFIED.,.F.,.F.,(4,2,2,
2,2,2,2,2,2,2,2,2,2,2,2,2,2,2,2,2,2,2,2,2,2,2,2,2,2,2,2,2,2,2,2,2,2,2,2,
2,2,2,2,2,2,2,2,2,2,2,2,2,2,2,2,2,2,2,2,2,2,2,2,2,2,2,2,2,2,2,2,2,2,2,2,
2,4),(1.36986813415593,1.41472412899457,1.42275371239178,1.42795815610329,
1.43215877399454,1.43697033725174,1.44532395773671,1.48475914832888,1.52808382678746,
1.57801766436043,1.58612816311396,1.58923460129861,1.59146233481792,1.59389580161617,
1.59742468867269,1.60672622206272,1.6207984267892,1.72155555163549,1.74101734255056,
1.74791649473522,1.75240742967011,1.75668758292653,1.76252803921264,1.77622949526211,
1.79534798025403,1.85118653392302,1.90046295084852,1.9085642526298,1.91166770971675,
1.91389316434396,1.91632694364819,1.91985632325798,1.92915698817388,1.94322649609053,
2.04392923303818,2.0634197220064,2.07032502908901,2.07481897653573,2.07910132519409,
2.08494378225342,2.09864589391576,2.11776428319321,2.17361744968784,2.2227639792405,
2.23086297872011,2.2339673672784,2.23619412675541,2.23862823951232,2.24215940538797,
2.25147388409074,2.26557238030009,2.36708984579862,2.3858867721409,2.39269421668486,
2.39671926778274,2.40087591432703,2.40630177308218,2.41229410913678,2.42230748761514,
2.47503917517413,2.5400265506722,2.55193121460002,2.55594425558728,2.55822838368599,
2.5606209119779,2.56392618471981,2.57181141164477,2.5830980277763,2.61673606462629,
2.68844376519829,2.70788382372786,2.71477326901278,2.71926253432093,2.72326380519083,
2.72743373181106,2.73269205327641,2.73843249748408),.UNSPECIFIED.);
#1429=B_SPLINE_CURVE_WITH_KNOTS('',3,(#40620,#40621,#40622,#40623,#40624,
#40625,#40626,#40627,#40628,#40629,#40630,#40631,#40632,#40633,#40634,#40635,
#40636,#40637,#40638,#40639,#40640,#40641,#40642,#40643,#40644,#40645,#40646,
#40647,#40648,#40649,#40650,#40651,#40652,#40653,#40654,#40655,#40656,#40657,
#40658,#40659,#40660,#40661,#40662,#40663,#40664,#40665,#40666,#40667,#40668,
#40669,#40670,#40671,#40672,#40673,#40674,#40675,#40676,#40677,#40678,#40679,
#40680,#40681,#40682,#40683,#40684,#40685,#40686,#40687,#40688,#40689,#40690,
#40691,#40692),.UNSPECIFIED.,.F.,.F.,(4,3,3,3,3,3,3,3,3,3,3,3,3,3,3,3,3,
3,3,3,3,3,3,3,4),(-4.09274904019424,-3.99140336690961,-3.90268063202685,
-3.81407250519492,-3.72555538516043,-3.63405502766315,-3.5456414745384,
-3.45724216684168,-3.36883591664657,-3.28040153632723,-3.19186974100238,
-3.10327972302285,-3.01456344360957,-2.99355252518221,-2.90585728432194,
-2.81827426436052,-2.73077877361514,-2.64334382474895,-2.55593995423922,
-2.46854499256392,-2.38113678182524,-2.29364202365736,-2.20610056041848,
-2.11842612027813,-2.06158267649742),.UNSPECIFIED.);
#1430=B_SPLINE_CURVE_WITH_KNOTS('',3,(#40696,#40697,#40698,#40699,#40700),
 .UNSPECIFIED.,.F.,.F.,(4,1,4),(0.,0.997850841727403,1.11004521091123),
 .UNSPECIFIED.);
#1431=B_SPLINE_CURVE_WITH_KNOTS('',3,(#40702,#40703,#40704,#40705,#40706,
#40707,#40708,#40709,#40710,#40711,#40712,#40713,#40714,#40715,#40716,#40717,
#40718,#40719,#40720,#40721,#40722,#40723,#40724,#40725,#40726,#40727,#40728,
#40729,#40730,#40731,#40732,#40733,#40734,#40735,#40736,#40737,#40738,#40739,
#40740,#40741,#40742,#40743,#40744,#40745,#40746,#40747,#40748,#40749,#40750,
#40751,#40752,#40753,#40754,#40755,#40756,#40757,#40758,#40759,#40760,#40761,
#40762,#40763,#40764,#40765,#40766,#40767,#40768,#40769,#40770,#40771,#40772,
#40773,#40774,#40775,#40776,#40777,#40778,#40779,#40780,#40781,#40782,#40783,
#40784,#40785,#40786,#40787,#40788,#40789,#40790,#40791,#40792,#40793,#40794,
#40795,#40796,#40797,#40798,#40799,#40800,#40801,#40802,#40803,#40804,#40805,
#40806,#40807,#40808,#40809,#40810,#40811,#40812,#40813,#40814,#40815,#40816,
#40817,#40818,#40819,#40820,#40821,#40822,#40823,#40824,#40825,#40826,#40827,
#40828,#40829,#40830,#40831,#40832,#40833,#40834,#40835,#40836,#40837,#40838,
#40839,#40840,#40841,#40842,#40843,#40844,#40845,#40846,#40847,#40848,#40849,
#40850,#40851,#40852,#40853,#40854,#40855,#40856,#40857,#40858,#40859,#40860,
#40861,#40862,#40863,#40864,#40865,#40866,#40867,#40868,#40869,#40870,#40871,
#40872,#40873,#40874,#40875,#40876,#40877,#40878,#40879,#40880,#40881,#40882,
#40883,#40884,#40885,#40886,#40887,#40888,#40889,#40890,#40891,#40892,#40893,
#40894,#40895,#40896,#40897,#40898,#40899,#40900,#40901,#40902,#40903,#40904,
#40905,#40906,#40907,#40908,#40909,#40910,#40911,#40912,#40913,#40914,#40915,
#40916,#40917,#40918,#40919,#40920,#40921,#40922,#40923,#40924,#40925,#40926,
#40927,#40928,#40929,#40930),.UNSPECIFIED.,.F.,.F.,(4,3,3,3,3,3,3,3,3,3,
3,3,3,3,3,3,3,3,3,3,3,3,3,3,3,3,3,3,3,3,3,3,3,3,3,3,3,3,3,3,3,3,3,3,3,3,
3,3,3,3,3,3,3,3,3,3,3,3,3,3,3,3,3,3,3,3,3,3,3,3,3,3,3,3,3,3,4),(1.11004521091123,
1.19681857962916,1.28348712019175,1.37251394059963,1.45905369666318,1.54557153490185,
1.63209020527474,1.72299307481976,1.80963167118428,1.89632823527782,1.98314923320001,
1.99570168345481,2.08428836921591,2.17275930675744,2.26113826477258,2.35269004732378,
2.44096386095791,2.52922308261749,2.61748904579692,2.70578308363948,2.79417514450019,
2.88262561661478,2.97120367664702,2.99355252518221,3.08226159218255,3.17085866821476,
3.25936734373045,3.35087184662785,3.43928348434477,3.52768329462181,3.61609246484359,
3.7045321838872,3.79307286406892,3.88167384880736,3.97040404053157,3.99140336690961,
4.07990226017908,4.16828588762427,4.25657812029096,4.34816263133422,4.43635174131991,
4.52452715507421,4.61271029903408,4.70092260011546,4.7892349478161,4.87760678960562,
4.96610841543857,4.98925420863701,5.07783461717695,5.1663006090823,5.25467595129453,
5.34622958867827,5.43450314168811,5.52276334774254,5.61103154350697,5.69932906623069,
5.78772645777222,5.8761833444269,5.96476936069165,5.98710505036441,6.07569171207561,
6.16416426366233,6.25254646262046,6.34409764130438,6.43237875249101,6.52064676413912,
6.60892300557215,6.69722880686894,6.78563478230987,6.87410044159731,6.96269544049623,
6.98495589209181,7.08702454854288,7.18451386528577,7.28173097504692,7.37854662647687,
7.3932305178961),.UNSPECIFIED.);
#1432=B_SPLINE_CURVE_WITH_KNOTS('',3,(#40932,#40933,#40934,#40935,#40936,
#40937,#40938,#40939,#40940,#40941,#40942,#40943,#40944,#40945,#40946,#40947,
#40948,#40949,#40950,#40951,#40952,#40953,#40954,#40955,#40956,#40957,#40958,
#40959,#40960,#40961,#40962,#40963,#40964,#40965,#40966,#40967,#40968,#40969,
#40970,#40971,#40972,#40973,#40974,#40975,#40976,#40977,#40978,#40979,#40980,
#40981,#40982,#40983,#40984,#40985,#40986,#40987,#40988,#40989,#40990,#40991,
#40992,#40993,#40994,#40995,#40996,#40997,#40998,#40999,#41000,#41001,#41002,
#41003,#41004,#41005,#41006,#41007,#41008,#41009,#41010,#41011,#41012,#41013,
#41014,#41015,#41016,#41017,#41018,#41019,#41020,#41021,#41022,#41023,#41024,
#41025,#41026,#41027,#41028,#41029,#41030,#41031,#41032,#41033,#41034,#41035,
#41036,#41037,#41038,#41039,#41040,#41041,#41042,#41043,#41044,#41045,#41046,
#41047,#41048,#41049,#41050,#41051,#41052,#41053,#41054,#41055,#41056,#41057,
#41058,#41059,#41060,#41061,#41062,#41063,#41064,#41065,#41066,#41067,#41068,
#41069,#41070,#41071,#41072,#41073,#41074,#41075,#41076,#41077,#41078,#41079,
#41080,#41081,#41082,#41083,#41084,#41085,#41086,#41087,#41088,#41089,#41090,
#41091,#41092,#41093,#41094,#41095,#41096,#41097,#41098,#41099,#41100,#41101,
#41102,#41103,#41104,#41105,#41106,#41107,#41108,#41109,#41110,#41111,#41112,
#41113,#41114,#41115,#41116,#41117,#41118,#41119,#41120,#41121,#41122,#41123,
#41124,#41125,#41126,#41127,#41128,#41129,#41130,#41131,#41132,#41133,#41134,
#41135,#41136,#41137,#41138,#41139,#41140,#41141,#41142,#41143,#41144,#41145,
#41146,#41147,#41148,#41149,#41150,#41151,#41152,#41153,#41154,#41155,#41156,
#41157),.UNSPECIFIED.,.F.,.F.,(4,3,3,3,3,3,3,3,3,3,3,3,3,3,3,3,3,3,3,3,
3,3,3,3,3,3,3,3,3,3,3,3,3,3,3,3,3,3,3,3,3,3,3,3,3,3,3,3,3,3,3,3,3,3,3,3,
3,3,3,3,3,3,3,3,3,3,3,3,3,3,3,3,3,3,3,4),(7.39323051809082,7.48288036686472,
7.57256220481202,7.66229492622905,7.75216069815711,7.84209994754193,7.9322010208113,
7.98280673381922,8.07138131775184,8.15984154810557,8.24821119867417,8.33976699578323,
8.42803507032422,8.51628988674049,8.60455278803785,8.69284511788348,8.7812374945029,
8.86968946404034,8.95827074499974,8.98065757554662,9.06923201113828,9.15769211569553,
9.24606166307021,9.33761750734569,9.42588553618497,9.51414032834517,9.60240322696447,
9.69069557585812,9.77908800384221,9.86754004367646,9.9561214222471,9.97850841727402,
10.067080560139,10.1555383329379,10.2439055125692,10.3354622308732,10.4237278170777,
10.5119801430473,10.6002405544998,10.688530397817,10.7769203054923,10.8653698133419,
10.9539486622742,10.9763592590014,11.0649326354006,11.1533916568987,11.2417600987877,
11.3333163490303,11.4215832232792,11.5098368446218,11.5980985573963,11.6863897066082,
11.7747809203645,11.8632317359969,11.951811885131,11.9742101007288,12.0627833654436,
12.1512422764058,12.2396106090393,12.3311669007164,12.4194336696461,12.5076871873168,
12.5959487981883,12.6842398473887,12.7726309644632,12.86108168524,12.9496617429377,
12.9720609424562,13.060105302808,13.1479581989514,13.2357263478001,13.3234317718887,
13.4116777852341,13.4993383649874,13.5878770951289,13.6764158252704),
 .UNSPECIFIED.);
#1433=B_SPLINE_CURVE_WITH_KNOTS('',3,(#41159,#41160,#41161,#41162,#41163,
#41164,#41165,#41166,#41167,#41168,#41169,#41170,#41171,#41172,#41173,#41174,
#41175,#41176,#41177,#41178,#41179,#41180,#41181,#41182,#41183,#41184,#41185,
#41186,#41187,#41188,#41189,#41190,#41191,#41192,#41193,#41194,#41195,#41196,
#41197,#41198,#41199,#41200,#41201,#41202,#41203,#41204,#41205,#41206,#41207,
#41208,#41209,#41210,#41211,#41212,#41213,#41214,#41215,#41216,#41217,#41218,
#41219,#41220,#41221,#41222,#41223,#41224,#41225,#41226,#41227,#41228,#41229,
#41230,#41231,#41232,#41233,#41234,#41235,#41236,#41237,#41238,#41239,#41240,
#41241,#41242,#41243,#41244,#41245,#41246,#41247,#41248,#41249,#41250,#41251,
#41252,#41253,#41254,#41255,#41256,#41257,#41258,#41259,#41260,#41261,#41262,
#41263,#41264,#41265,#41266,#41267,#41268,#41269,#41270,#41271,#41272,#41273,
#41274,#41275,#41276,#41277,#41278,#41279,#41280,#41281,#41282,#41283,#41284,
#41285,#41286,#41287,#41288,#41289,#41290,#41291,#41292,#41293,#41294,#41295,
#41296,#41297,#41298,#41299,#41300,#41301,#41302,#41303,#41304,#41305,#41306,
#41307,#41308,#41309,#41310,#41311,#41312,#41313,#41314,#41315,#41316,#41317,
#41318,#41319,#41320,#41321,#41322,#41323,#41324,#41325,#41326,#41327,#41328,
#41329,#41330,#41331,#41332,#41333,#41334,#41335,#41336,#41337,#41338,#41339,
#41340,#41341,#41342,#41343,#41344,#41345,#41346,#41347,#41348,#41349,#41350,
#41351,#41352,#41353,#41354,#41355,#41356,#41357,#41358,#41359,#41360,#41361,
#41362,#41363,#41364,#41365,#41366,#41367,#41368,#41369,#41370,#41371,#41372,
#41373,#41374,#41375,#41376,#41377,#41378,#41379,#41380,#41381,#41382,#41383,
#41384,#41385,#41386,#41387),.UNSPECIFIED.,.F.,.F.,(4,3,3,3,3,3,3,3,3,3,
3,3,3,3,3,3,3,3,3,3,3,3,3,3,3,3,3,3,3,3,3,3,3,3,3,3,3,3,3,3,3,3,3,3,3,3,
3,3,3,3,3,3,3,3,3,3,3,3,3,3,3,3,3,3,3,3,3,3,3,3,3,3,3,3,3,3,4),(13.6764158254185,
13.7833994164136,13.8918858024763,13.9699117841836,14.0584849658365,14.1469437914998,
14.2353120367115,14.3268683603615,14.4151350371095,14.5033884609907,14.5916499765596,
14.6799409290381,14.7683319477645,14.8567825691239,14.9453625265971,14.967762625911,
15.0563357846373,15.1447945873451,15.2331628096013,15.324719141856,15.4129857957979,
15.5012391969687,15.5895006899479,15.677791619983,15.7661826165984,15.8546332160138,
15.943213151958,15.9656134676384,16.0541866044928,16.1426453849034,16.2310135844665,
16.3225699250789,16.410836555482,16.4990899328407,16.5873514017595,16.6756423075101,
16.7640332796304,16.8524838543977,16.941063765659,16.9634643093658,17.0520374629929,
17.1404962604055,17.2288644771775,17.320420811417,17.4086874594366,17.4969408545324,
17.58520234129,17.6734932649627,17.7618842550379,17.8503348478012,17.9389147769802,
17.9613151510932,18.0498883010376,18.1383470947465,18.2267153077987,18.3182716434264,
18.4065382877099,18.49479167907,18.5830531620966,18.6713440820469,18.7597350684314,
18.8481856575184,18.9367655830698,18.9591659928206,19.0477391407883,19.1361979324781,
19.2245661434715,19.316122479856,19.4043891219944,19.4926425111812,19.5809039920083,
19.6691949097351,19.7575858938721,19.8460364806943,19.9346164039739,19.957016834548,
19.95960113245),.UNSPECIFIED.);
#1434=B_SPLINE_CURVE_WITH_KNOTS('',3,(#41389,#41390,#41391,#41392,#41393,
#41394,#41395,#41396,#41397,#41398,#41399,#41400,#41401,#41402,#41403,#41404,
#41405,#41406,#41407,#41408,#41409,#41410,#41411,#41412,#41413,#41414,#41415,
#41416,#41417,#41418,#41419,#41420,#41421,#41422,#41423,#41424,#41425,#41426,
#41427,#41428,#41429,#41430,#41431,#41432,#41433,#41434,#41435,#41436,#41437,
#41438,#41439,#41440,#41441,#41442,#41443,#41444,#41445,#41446,#41447,#41448,
#41449,#41450,#41451,#41452,#41453,#41454,#41455,#41456,#41457,#41458,#41459,
#41460,#41461,#41462,#41463,#41464,#41465,#41466,#41467,#41468,#41469,#41470,
#41471,#41472,#41473,#41474,#41475,#41476,#41477,#41478,#41479,#41480,#41481,
#41482,#41483,#41484,#41485,#41486,#41487,#41488,#41489,#41490,#41491,#41492,
#41493,#41494,#41495,#41496,#41497,#41498,#41499,#41500,#41501,#41502,#41503,
#41504,#41505,#41506,#41507,#41508,#41509,#41510,#41511,#41512,#41513,#41514,
#41515,#41516,#41517,#41518,#41519,#41520,#41521,#41522,#41523,#41524,#41525,
#41526,#41527,#41528,#41529,#41530,#41531,#41532,#41533,#41534,#41535,#41536,
#41537,#41538,#41539,#41540,#41541,#41542,#41543,#41544,#41545,#41546,#41547,
#41548,#41549,#41550,#41551,#41552,#41553,#41554,#41555,#41556,#41557,#41558,
#41559,#41560,#41561,#41562,#41563,#41564,#41565,#41566,#41567,#41568,#41569,
#41570,#41571,#41572,#41573,#41574,#41575,#41576,#41577,#41578,#41579,#41580,
#41581,#41582,#41583,#41584,#41585,#41586,#41587,#41588,#41589,#41590,#41591,
#41592,#41593,#41594,#41595,#41596,#41597,#41598,#41599,#41600,#41601,#41602,
#41603,#41604,#41605,#41606,#41607,#41608,#41609,#41610,#41611,#41612,#41613,
#41614),.UNSPECIFIED.,.F.,.F.,(4,3,3,3,3,3,3,3,3,3,3,3,3,3,3,3,3,3,3,3,
3,3,3,3,3,3,3,3,3,3,3,3,3,3,3,3,3,3,3,3,3,3,3,3,3,3,3,3,3,3,3,3,3,3,3,3,
3,3,3,3,3,3,3,3,3,3,3,3,3,3,3,3,3,3,3,4),(19.9596011325877,20.0481329717931,
20.1365504859385,20.2248775009963,20.3161262729062,20.404352141197,20.4925649061808,
20.5807859574653,20.6690366855045,20.7573874921075,20.8457982021158,20.9343376898428,
20.9548676762755,21.043440825605,21.1318996186796,21.2202678310788,21.3118241669443,
21.4000908105316,21.4883442011809,21.5766056834827,21.6648966026947,21.753287588325,
21.8417381766471,21.9303181014248,21.9527185180029,22.0412916671691,22.1297504600762,
22.2181186723037,22.3096750082321,22.3979416516396,22.4861950421065,22.574456524223,
22.6627474432473,22.7511384286871,22.839589016817,22.9281689414009,22.9505693597303,
23.0391425091049,23.1276013022237,23.2159695146662,23.3075258505151,23.3957924941428,
23.4840458848314,23.5723073671713,23.6605982864196,23.7489892720849,23.8374398604412,
23.926019785251,23.9484202014577,24.0369933507614,24.125452143808,24.2138203561779,
24.3053766920538,24.3936433356082,24.4818967262232,24.5701582084893,24.6584491276642,
24.7468401132559,24.8352907015382,24.9238706262749,24.9462710431851,25.0348441924774,
25.1233029855122,25.2116711978705,25.3032275337507,25.3914941772924,25.4797475678944,
25.5680090501472,25.6562999693086,25.7446909548863,25.8331415431545,25.9217214678769,
25.9441218849125,26.0521117084359,26.1587324100376,26.2427864394712),
 .UNSPECIFIED.);
#1435=B_SPLINE_CURVE_WITH_KNOTS('',3,(#41616,#41617,#41618,#41619,#41620,
#41621,#41622,#41623,#41624,#41625,#41626,#41627,#41628,#41629,#41630,#41631,
#41632,#41633,#41634,#41635,#41636,#41637,#41638,#41639,#41640,#41641,#41642,
#41643,#41644,#41645,#41646,#41647,#41648,#41649,#41650,#41651,#41652,#41653,
#41654,#41655,#41656,#41657,#41658,#41659,#41660,#41661,#41662,#41663,#41664,
#41665,#41666,#41667,#41668,#41669,#41670,#41671,#41672,#41673,#41674,#41675,
#41676,#41677,#41678,#41679,#41680,#41681,#41682,#41683,#41684,#41685,#41686,
#41687,#41688,#41689,#41690,#41691,#41692,#41693,#41694,#41695,#41696,#41697,
#41698,#41699,#41700,#41701,#41702,#41703,#41704,#41705,#41706,#41707,#41708,
#41709,#41710,#41711,#41712,#41713,#41714,#41715,#41716,#41717,#41718,#41719,
#41720,#41721,#41722,#41723,#41724,#41725,#41726,#41727,#41728,#41729,#41730,
#41731,#41732,#41733,#41734,#41735,#41736,#41737,#41738,#41739,#41740,#41741,
#41742,#41743,#41744,#41745,#41746,#41747,#41748,#41749,#41750,#41751,#41752,
#41753,#41754,#41755,#41756,#41757,#41758,#41759,#41760,#41761,#41762,#41763,
#41764,#41765,#41766,#41767,#41768,#41769,#41770,#41771,#41772,#41773,#41774,
#41775,#41776,#41777,#41778,#41779,#41780,#41781,#41782,#41783,#41784,#41785,
#41786,#41787,#41788,#41789,#41790,#41791,#41792,#41793,#41794,#41795,#41796,
#41797,#41798,#41799,#41800,#41801,#41802,#41803,#41804,#41805,#41806,#41807,
#41808,#41809,#41810,#41811,#41812,#41813,#41814,#41815,#41816,#41817,#41818,
#41819,#41820,#41821,#41822,#41823,#41824,#41825,#41826,#41827,#41828,#41829,
#41830,#41831,#41832,#41833,#41834,#41835,#41836,#41837,#41838,#41839,#41840,
#41841),.UNSPECIFIED.,.F.,.F.,(4,3,3,3,3,3,3,3,3,3,3,3,3,3,3,3,3,3,3,3,
3,3,3,3,3,3,3,3,3,3,3,3,3,3,3,3,3,3,3,3,3,3,3,3,3,3,3,3,3,3,3,3,3,3,3,3,
3,3,3,3,3,3,3,3,3,3,3,3,3,3,3,3,3,3,3,4),(26.2427864396296,26.3305471278199,
26.4182777501481,26.5060001655125,26.5937362218,26.6815653163576,26.7694406835887,
26.8574653064194,26.9419727266399,27.0305458759455,27.1190046689943,27.2073728813658,
27.298929217241,27.387195860797,27.4754492514135,27.5637107336809,27.6520016528573,
27.7403926384499,27.8288432267331,27.9174231514704,27.9398235683673,28.0283967176725,
28.1168555107208,28.2052237230921,28.2967800589675,28.3850467025228,28.4733000931386,
28.561561575405,28.6498524945803,28.7382434801722,28.826694068455,28.9152739931916,
28.9376744100947,29.0262475594023,29.114706352453,29.2030745648264,29.2946309007009,
29.3828975442588,29.4711509348772,29.5594124171467,29.6477033363247,29.7360943219193,
29.824544910205,29.9131248349443,29.9355252518221,30.0240984011285,30.1125571941781,
30.2009254065503,30.2924817424252,30.3807483859818,30.469001776599,30.5572632588673,
30.645554178044,30.7339451636374,30.8223957519215,30.9109756766594,30.9333760935495,
31.021949242856,31.1104080359057,31.1987762482784,31.2903325841532,31.37859922771,
31.4668526183273,31.5551141005953,31.6434050197721,31.7317960053654,31.8202465936495,
31.9088265183877,31.9312269352769,32.0211983969395,32.1110439823456,32.2007831067229,
32.2904186784366,32.3799933630522,32.4695266106531,32.5259717468092),
 .UNSPECIFIED.);
#1436=B_SPLINE_CURVE_WITH_KNOTS('',3,(#41843,#41844,#41845,#41846,#41847,
#41848,#41849,#41850,#41851,#41852,#41853,#41854,#41855,#41856,#41857,#41858,
#41859,#41860,#41861,#41862,#41863,#41864,#41865,#41866,#41867,#41868,#41869,
#41870,#41871,#41872,#41873,#41874,#41875,#41876,#41877,#41878,#41879,#41880,
#41881,#41882,#41883,#41884,#41885,#41886,#41887,#41888,#41889,#41890,#41891,
#41892,#41893,#41894,#41895,#41896,#41897,#41898,#41899,#41900,#41901,#41902,
#41903,#41904,#41905,#41906,#41907,#41908,#41909,#41910,#41911,#41912,#41913,
#41914,#41915,#41916,#41917,#41918,#41919,#41920,#41921,#41922,#41923,#41924,
#41925,#41926,#41927,#41928,#41929,#41930,#41931,#41932,#41933,#41934,#41935,
#41936,#41937,#41938,#41939,#41940,#41941,#41942,#41943,#41944,#41945,#41946,
#41947,#41948,#41949,#41950,#41951,#41952,#41953,#41954,#41955,#41956,#41957,
#41958,#41959,#41960,#41961,#41962,#41963,#41964,#41965,#41966,#41967,#41968,
#41969,#41970,#41971,#41972,#41973,#41974,#41975,#41976,#41977,#41978,#41979,
#41980,#41981,#41982,#41983,#41984,#41985,#41986,#41987,#41988,#41989,#41990,
#41991,#41992,#41993,#41994,#41995,#41996,#41997,#41998,#41999,#42000,#42001,
#42002,#42003,#42004,#42005,#42006,#42007,#42008,#42009,#42010,#42011,#42012,
#42013,#42014,#42015,#42016,#42017,#42018,#42019,#42020,#42021,#42022,#42023,
#42024,#42025,#42026,#42027,#42028,#42029,#42030,#42031,#42032,#42033,#42034,
#42035,#42036,#42037,#42038,#42039,#42040,#42041,#42042,#42043,#42044,#42045,
#42046,#42047,#42048,#42049,#42050,#42051,#42052,#42053,#42054,#42055,#42056,
#42057,#42058,#42059,#42060,#42061,#42062,#42063,#42064,#42065,#42066,#42067,
#42068),.UNSPECIFIED.,.F.,.F.,(4,3,3,3,3,3,3,3,3,3,3,3,3,3,3,3,3,3,3,3,
3,3,3,3,3,3,3,3,3,3,3,3,3,3,3,3,3,3,3,3,3,3,3,3,3,3,3,3,3,3,3,3,3,3,3,3,
3,3,3,3,3,3,3,3,3,3,3,3,3,3,3,3,3,3,3,4),(32.5259717470101,32.6267482545086,
32.7244046859025,32.8267412314534,32.9290777770043,33.0176509263108,33.1061097193606,
33.1944779317332,33.286034267608,33.3743009111648,33.462554301782,33.5508157840503,
33.6391067032275,33.727497688821,33.8159482771052,33.9045282018435,33.9269286187317,
34.0155017680383,34.103960561088,34.1923287734605,34.2838851093353,34.3721517528922,
34.4604051435095,34.5486666257778,34.636957544955,34.7253485305484,34.8137991188327,
34.9023790435709,34.9247794604591,35.0133526097657,35.1018114028155,35.1901796151881,
35.2817359510629,35.3700025946197,35.458255985237,35.5465174675054,35.6348083866826,
35.7231993722761,35.8116499605603,35.9002298852985,35.9226303021865,36.0112034514932,
36.0996622445429,36.1880304569156,36.2795867927904,36.3678534363472,36.4561068269646,
36.544368309233,36.6326592284102,36.7210502140037,36.809500802288,36.8980807270263,
36.9204811439139,37.0090542932204,37.0975130862701,37.1858812986425,37.2774376345174,
37.3657042780741,37.4539576686913,37.5422191509596,37.6305100701367,37.7189010557301,
37.8073516440141,37.8959315687522,37.9183319856413,38.0057567402234,38.0930680815749,
38.1825792030973,38.269738045413,38.3568657274577,38.4439846320742,38.5352777374942,
38.6224901904441,38.7097513439552,38.7971229178579,38.8091570537541),
 .UNSPECIFIED.);
#1437=B_SPLINE_CURVE_WITH_KNOTS('',3,(#42070,#42071,#42072,#42073,#42074,
#42075,#42076,#42077,#42078,#42079,#42080,#42081,#42082,#42083,#42084,#42085,
#42086,#42087,#42088,#42089,#42090,#42091,#42092,#42093,#42094,#42095,#42096,
#42097,#42098,#42099,#42100,#42101,#42102,#42103,#42104,#42105,#42106,#42107,
#42108,#42109,#42110,#42111,#42112,#42113,#42114,#42115,#42116,#42117,#42118,
#42119,#42120,#42121,#42122,#42123,#42124,#42125,#42126,#42127,#42128,#42129,
#42130,#42131,#42132,#42133,#42134,#42135,#42136,#42137,#42138,#42139,#42140,
#42141,#42142,#42143,#42144,#42145,#42146,#42147,#42148,#42149,#42150,#42151,
#42152,#42153,#42154,#42155,#42156,#42157,#42158,#42159,#42160,#42161,#42162,
#42163,#42164,#42165,#42166,#42167,#42168,#42169,#42170,#42171,#42172,#42173,
#42174,#42175,#42176,#42177,#42178,#42179,#42180,#42181,#42182,#42183,#42184,
#42185,#42186,#42187,#42188,#42189,#42190,#42191,#42192,#42193,#42194,#42195,
#42196,#42197,#42198,#42199,#42200,#42201,#42202,#42203,#42204,#42205,#42206,
#42207,#42208,#42209,#42210,#42211,#42212,#42213,#42214,#42215,#42216,#42217,
#42218,#42219,#42220,#42221,#42222,#42223,#42224,#42225,#42226,#42227,#42228,
#42229,#42230,#42231,#42232,#42233,#42234,#42235,#42236,#42237,#42238,#42239,
#42240,#42241,#42242,#42243,#42244,#42245,#42246,#42247,#42248,#42249,#42250,
#42251,#42252,#42253,#42254,#42255,#42256,#42257,#42258,#42259,#42260,#42261,
#42262,#42263,#42264,#42265,#42266,#42267,#42268,#42269,#42270,#42271,#42272,
#42273,#42274,#42275,#42276,#42277,#42278,#42279,#42280,#42281,#42282,#42283,
#42284,#42285,#42286,#42287,#42288,#42289,#42290,#42291,#42292,#42293,#42294,
#42295),.UNSPECIFIED.,.F.,.F.,(4,3,3,3,3,3,3,3,3,3,3,3,3,3,3,3,3,3,3,3,
3,3,3,3,3,3,3,3,3,3,3,3,3,3,3,3,3,3,3,3,3,3,3,3,3,3,3,3,3,3,3,3,3,3,3,3,
3,3,3,3,3,3,3,3,3,3,3,3,3,3,3,3,3,3,3,4),(38.8091570539888,38.9161828273687,
39.0047559766753,39.0932147697253,39.181582982098,39.2731393179728,39.3614059615296,
39.4496593521471,39.5379208344155,39.6262117535927,39.7146027391863,39.8030533274705,
39.8916332522088,39.9140336690961,40.0026068184029,40.0910656114527,40.1794338238255,
40.2709901597002,40.3592568032572,40.4475101938747,40.5357716761431,40.6240625953204,
40.712453580914,40.8009041691985,40.8894840939368,40.9118845108235,41.00045766013,
41.0889164531796,41.177284665552,41.2688410014269,41.3571076449836,41.4453610356008,
41.533622517869,41.6219134370461,41.7103044226395,41.7987550109236,41.8873349356617,
41.9097353525509,41.9983085018575,42.0867672949072,42.1751355072797,42.2666918431545,
42.3549584867113,42.4432118773286,42.5314733595969,42.6197642787741,42.7081552643675,
42.7966058526517,42.8851857773899,42.9075861942783,42.9961593435851,43.0846181366349,
43.1729863490076,43.2645426848824,43.3528093284394,43.4410627190568,43.5293242013252,
43.6176151205024,43.7060061060961,43.7944566943805,43.8830366191189,43.9054370360057,
43.9940101853122,44.0824689783619,44.1708371907343,44.2623935266091,44.3506601701658,
44.438913560783,44.5271750430515,44.6154659622283,44.7038569478217,44.7923075361057,
44.8808874608438,44.9032878777331,45.0337718756005,45.0923423611683),
 .UNSPECIFIED.);
#1438=B_SPLINE_CURVE_WITH_KNOTS('',3,(#42297,#42298,#42299,#42300,#42301,
#42302,#42303,#42304,#42305,#42306,#42307,#42308,#42309,#42310,#42311,#42312,
#42313,#42314,#42315,#42316,#42317,#42318,#42319,#42320,#42321,#42322,#42323,
#42324,#42325,#42326,#42327,#42328,#42329,#42330,#42331,#42332,#42333,#42334,
#42335,#42336,#42337,#42338,#42339,#42340,#42341,#42342,#42343,#42344,#42345,
#42346,#42347,#42348,#42349,#42350,#42351,#42352,#42353,#42354,#42355,#42356,
#42357,#42358,#42359,#42360,#42361,#42362,#42363,#42364,#42365,#42366,#42367,
#42368,#42369,#42370,#42371,#42372,#42373,#42374,#42375,#42376,#42377,#42378,
#42379,#42380,#42381,#42382,#42383,#42384,#42385,#42386,#42387,#42388,#42389,
#42390,#42391,#42392,#42393,#42394,#42395,#42396,#42397,#42398,#42399,#42400,
#42401,#42402,#42403,#42404,#42405,#42406,#42407,#42408,#42409,#42410,#42411,
#42412,#42413,#42414,#42415,#42416,#42417,#42418,#42419,#42420,#42421,#42422,
#42423,#42424,#42425,#42426,#42427,#42428,#42429,#42430,#42431,#42432,#42433,
#42434,#42435,#42436,#42437,#42438,#42439,#42440,#42441,#42442,#42443,#42444,
#42445,#42446,#42447,#42448,#42449,#42450,#42451,#42452,#42453,#42454,#42455,
#42456,#42457,#42458,#42459,#42460,#42461,#42462,#42463,#42464,#42465,#42466,
#42467,#42468,#42469,#42470,#42471,#42472,#42473,#42474,#42475,#42476,#42477,
#42478,#42479,#42480,#42481,#42482,#42483,#42484,#42485,#42486,#42487,#42488,
#42489,#42490,#42491,#42492,#42493,#42494,#42495,#42496,#42497,#42498,#42499,
#42500,#42501,#42502,#42503,#42504,#42505,#42506,#42507,#42508,#42509,#42510,
#42511,#42512,#42513,#42514,#42515,#42516,#42517,#42518,#42519,#42520,#42521,
#42522,#42523,#42524,#42525),.UNSPECIFIED.,.F.,.F.,(4,3,3,3,3,3,3,3,3,3,
3,3,3,3,3,3,3,3,3,3,3,3,3,3,3,3,3,3,3,3,3,3,3,3,3,3,3,3,3,3,3,3,3,3,3,3,
3,3,3,3,3,3,3,3,3,3,3,3,3,3,3,3,3,3,3,3,3,3,3,3,3,3,3,3,3,3,4),(45.0923423614058,
45.1794682863814,45.2696770905163,45.3566731775864,45.4436469087234,45.5306207667714,
45.6176172314561,45.7047067004475,45.7918517845714,45.8791228652891,45.9011387194605,
45.989711868767,46.0781706618167,46.1665388741891,46.258095210064,46.3463618536207,
46.434615244238,46.5228767265062,46.6111676456835,46.6995586312769,46.7880092195609,
46.8765891442992,46.8989895611879,46.9875627104945,47.0760215035442,47.164389715917,
47.2559460517918,47.3442126953487,47.432466085966,47.5207275682341,47.6090184874112,
47.6974094730047,47.785860061289,47.8744399860272,47.8968404029153,47.9854135522218,
48.0738723452715,48.162240557644,48.2537968935189,48.3420635370757,48.4303169276929,
48.5185784099612,48.6068693291381,48.6952603147317,48.7837109030158,48.8722908277539,
48.8946912446427,48.9832643939494,49.0717231869992,49.1600913993721,49.2516477352468,
49.3399143788038,49.4281677694212,49.5164292516896,49.6047201708667,49.6931111564602,
49.7815617447447,49.8701416694831,49.8925420863701,49.9811152356767,50.069574028726,
50.1579422410982,50.2494985769732,50.3377652205299,50.4260186111471,50.5142800934155,
50.6025710125928,50.6909619981861,50.7794125864703,50.8679925112085,50.8903929280975,
50.9841089426365,51.0819636240283,51.175258107441,51.2684075657143,51.3613757125319,
51.3755276682037),.UNSPECIFIED.);
#1439=B_SPLINE_CURVE_WITH_KNOTS('',3,(#42527,#42528,#42529,#42530,#42531,
#42532,#42533,#42534,#42535,#42536,#42537,#42538,#42539,#42540,#42541,#42542,
#42543,#42544,#42545,#42546,#42547,#42548,#42549,#42550,#42551,#42552,#42553,
#42554,#42555,#42556,#42557,#42558,#42559,#42560,#42561,#42562,#42563,#42564,
#42565,#42566,#42567,#42568,#42569,#42570,#42571,#42572,#42573,#42574,#42575,
#42576,#42577,#42578,#42579,#42580,#42581,#42582,#42583,#42584,#42585,#42586,
#42587,#42588,#42589,#42590,#42591,#42592,#42593,#42594,#42595,#42596,#42597,
#42598,#42599,#42600,#42601,#42602,#42603,#42604,#42605,#42606,#42607,#42608,
#42609,#42610,#42611,#42612,#42613,#42614,#42615,#42616,#42617,#42618,#42619,
#42620,#42621,#42622,#42623,#42624,#42625,#42626,#42627,#42628,#42629,#42630,
#42631,#42632,#42633,#42634,#42635,#42636,#42637,#42638,#42639,#42640,#42641,
#42642,#42643,#42644,#42645,#42646,#42647,#42648,#42649,#42650,#42651,#42652,
#42653,#42654,#42655,#42656,#42657,#42658,#42659,#42660,#42661,#42662,#42663,
#42664,#42665,#42666,#42667,#42668,#42669,#42670,#42671,#42672,#42673,#42674,
#42675,#42676,#42677,#42678,#42679,#42680,#42681,#42682,#42683,#42684,#42685,
#42686,#42687,#42688,#42689,#42690,#42691,#42692,#42693,#42694,#42695,#42696,
#42697,#42698,#42699,#42700,#42701,#42702,#42703,#42704,#42705,#42706,#42707,
#42708,#42709,#42710,#42711,#42712,#42713,#42714,#42715,#42716,#42717,#42718,
#42719,#42720,#42721,#42722,#42723,#42724,#42725,#42726,#42727,#42728,#42729,
#42730,#42731,#42732,#42733,#42734,#42735,#42736,#42737,#42738,#42739,#42740,
#42741,#42742,#42743,#42744,#42745,#42746,#42747,#42748,#42749,#42750,#42751,
#42752),.UNSPECIFIED.,.F.,.F.,(4,3,3,3,3,3,3,3,3,3,3,3,3,3,3,3,3,3,3,3,
3,3,3,3,3,3,3,3,3,3,3,3,3,3,3,3,3,3,3,3,3,3,3,3,3,3,3,3,3,3,3,3,3,3,3,3,
3,3,3,3,3,3,3,3,3,3,3,3,3,3,3,3,3,3,3,4),(51.3755276683479,51.4674551182633,
51.5594915131789,51.6517320877935,51.7440828937281,51.8366378040773,51.8882437698249,
51.9768169191314,52.065275712181,52.1536439245534,52.2452002604282,52.3334669039849,
52.421720294602,52.5099817768701,52.598272696047,52.6866636816403,52.7751142699245,
52.8636941946625,52.8860946115523,52.974667760859,53.063126553909,53.1514947662817,
53.2430511021564,53.3313177457134,53.4195711363307,53.5078326185991,53.5961235377762,
53.6845145233698,53.7729651116538,53.8615450363921,53.8839454532797,53.9725186025863,
54.0609773956361,54.1493456080088,54.2409019438836,54.3291685874404,54.4174219780577,
54.5056834603261,54.593974379503,54.6823653650966,54.7708159533807,54.8593958781189,
54.8817962950071,54.9703694443136,55.0588282373631,55.1471964497356,55.2387527856105,
55.3270194291673,55.4152728197845,55.5035343020528,55.5918252212297,55.680216206823,
55.7686667951072,55.8572467198455,55.8796471367346,55.9682202860413,56.0566790790914,
56.1450472914638,56.2366036273385,56.3248702708955,56.4131236615128,56.5013851437812,
56.5896760629585,56.6780670485522,56.7665176368358,56.855097561574,56.877497978462,
56.9648624461651,57.0520884991052,57.1392356291957,57.226326359989,57.3133831580095,
57.4004603167845,57.4875438192554,57.5747123789959,57.6587129753234),
 .UNSPECIFIED.);
#1440=B_SPLINE_CURVE_WITH_KNOTS('',3,(#42754,#42755,#42756,#42757,#42758,
#42759,#42760,#42761,#42762,#42763,#42764,#42765,#42766,#42767,#42768,#42769,
#42770,#42771,#42772,#42773,#42774,#42775,#42776,#42777,#42778,#42779,#42780,
#42781,#42782,#42783,#42784,#42785,#42786,#42787,#42788,#42789,#42790,#42791,
#42792,#42793,#42794,#42795,#42796,#42797,#42798,#42799,#42800,#42801,#42802,
#42803,#42804,#42805,#42806,#42807,#42808,#42809,#42810,#42811,#42812,#42813,
#42814,#42815,#42816,#42817,#42818,#42819,#42820,#42821,#42822,#42823,#42824,
#42825,#42826,#42827,#42828,#42829,#42830,#42831,#42832,#42833,#42834,#42835,
#42836,#42837,#42838,#42839,#42840,#42841,#42842,#42843,#42844,#42845,#42846,
#42847,#42848,#42849,#42850,#42851,#42852,#42853,#42854,#42855,#42856,#42857,
#42858,#42859,#42860,#42861,#42862,#42863,#42864,#42865,#42866,#42867,#42868,
#42869,#42870,#42871,#42872,#42873,#42874,#42875,#42876,#42877,#42878,#42879,
#42880,#42881,#42882,#42883,#42884,#42885,#42886,#42887,#42888,#42889,#42890,
#42891,#42892,#42893,#42894,#42895,#42896,#42897,#42898,#42899,#42900,#42901,
#42902,#42903,#42904,#42905,#42906,#42907,#42908,#42909,#42910,#42911,#42912,
#42913,#42914,#42915,#42916,#42917,#42918,#42919,#42920,#42921,#42922,#42923,
#42924,#42925,#42926,#42927,#42928,#42929,#42930,#42931,#42932,#42933,#42934,
#42935,#42936,#42937,#42938,#42939,#42940,#42941,#42942,#42943,#42944,#42945,
#42946,#42947,#42948,#42949,#42950,#42951,#42952,#42953,#42954,#42955,#42956,
#42957,#42958,#42959,#42960,#42961,#42962,#42963,#42964,#42965,#42966,#42967,
#42968,#42969,#42970,#42971,#42972,#42973,#42974,#42975,#42976,#42977,#42978,
#42979),.UNSPECIFIED.,.F.,.F.,(4,3,3,3,3,3,3,3,3,3,3,3,3,3,3,3,3,3,3,3,
3,3,3,3,3,3,3,3,3,3,3,3,3,3,3,3,3,3,3,3,3,3,3,3,3,3,3,3,3,3,3,3,3,3,3,3,
3,3,3,3,3,3,3,3,3,3,3,3,3,3,3,3,3,3,3,4),(57.6587129755275,57.7806561529807,
57.8753488201894,57.963921969496,58.0523807625458,58.1407489749183,58.2323053107931,
58.32057195435,58.4088253449673,58.4970868272357,58.585377746413,58.6737687320065,
58.7622193202907,58.8507992450289,58.8731996619168,58.9617728112232,59.0502316042727,
59.1385998166451,59.23015615252,59.3184227960766,59.4066761866937,59.4949376689618,
59.5832285881387,59.671619573732,59.7600701620161,59.8486500867541,59.8710505036442,
59.9596236529509,60.0480824460007,60.1364506583733,60.2280069942481,60.316273637805,
60.4045270284224,60.4927885106908,60.581079429868,60.6694704154616,60.7579210037459,
60.8465009284842,60.8689013453716,60.9574744946783,61.0459332877281,61.1343015001007,
61.2258578359755,61.3141244795324,61.4023778701499,61.4906393524183,61.5789302715955,
61.6673212571891,61.7557718454734,61.8443517702117,61.866752187099,61.9553253364055,
62.0437841294551,62.1321523418276,62.2237086777024,62.3119753212591,62.4002287118763,
62.4884901941445,62.5767811133215,62.6651720989148,62.7536226871989,62.842202611937,
62.8646030288264,62.953176178133,63.0416349711828,63.1300031835554,63.2215595194302,
63.3098261629871,63.3980795536044,63.4863410358728,63.57463195505,63.6630229406436,
63.7514735289279,63.8400534536661,63.8624538705538,63.9418982827071),
 .UNSPECIFIED.);
#1441=B_SPLINE_CURVE_WITH_KNOTS('',3,(#42981,#42982,#42983,#42984,#42985,
#42986,#42987,#42988,#42989,#42990,#42991,#42992,#42993,#42994,#42995,#42996,
#42997,#42998,#42999,#43000,#43001,#43002,#43003,#43004,#43005,#43006,#43007,
#43008,#43009,#43010,#43011,#43012,#43013,#43014,#43015,#43016,#43017,#43018,
#43019,#43020,#43021,#43022,#43023,#43024,#43025,#43026,#43027,#43028,#43029,
#43030,#43031,#43032,#43033,#43034,#43035,#43036,#43037,#43038,#43039,#43040,
#43041,#43042,#43043,#43044,#43045,#43046,#43047,#43048,#43049,#43050,#43051,
#43052,#43053,#43054,#43055,#43056,#43057,#43058,#43059,#43060,#43061,#43062,
#43063,#43064,#43065,#43066,#43067,#43068,#43069,#43070,#43071,#43072,#43073,
#43074,#43075,#43076,#43077,#43078,#43079,#43080,#43081,#43082,#43083,#43084,
#43085,#43086,#43087,#43088,#43089,#43090,#43091,#43092,#43093,#43094,#43095,
#43096,#43097,#43098,#43099,#43100,#43101,#43102,#43103,#43104,#43105,#43106,
#43107,#43108,#43109,#43110,#43111,#43112,#43113,#43114,#43115,#43116,#43117,
#43118,#43119,#43120,#43121,#43122,#43123,#43124,#43125,#43126,#43127,#43128,
#43129,#43130,#43131,#43132,#43133,#43134,#43135,#43136,#43137,#43138,#43139,
#43140,#43141,#43142,#43143,#43144,#43145,#43146,#43147,#43148,#43149,#43150,
#43151,#43152,#43153,#43154,#43155,#43156,#43157,#43158,#43159,#43160,#43161,
#43162,#43163,#43164,#43165,#43166,#43167,#43168,#43169,#43170,#43171,#43172,
#43173,#43174,#43175,#43176,#43177,#43178,#43179,#43180,#43181,#43182,#43183,
#43184,#43185,#43186,#43187,#43188,#43189,#43190,#43191,#43192,#43193,#43194,
#43195,#43196,#43197,#43198,#43199,#43200,#43201,#43202,#43203,#43204,#43205,
#43206),.UNSPECIFIED.,.F.,.F.,(4,3,3,3,3,3,3,3,3,3,3,3,3,3,3,3,3,3,3,3,
3,3,3,3,3,3,3,3,3,3,3,3,3,3,3,3,3,3,3,3,3,3,3,3,3,3,3,3,3,3,3,3,3,3,3,3,
3,3,3,3,3,3,3,3,3,3,3,3,3,3,3,3,3,3,3,4),(63.9418982829247,64.0294781425003,
64.1169515893512,64.2043433733613,64.2916830535804,64.3789971694347,64.4663079591173,
64.5536376539925,64.6410595742652,64.7285333074612,64.816140164755,64.8603047122812,
64.9488778615877,65.0373366546372,65.1257048670097,65.2172612028846,65.3055278464413,
65.3937812370584,65.4820427193266,65.5703336385034,65.6587246240968,65.747175212381,
65.8357551371191,65.8581555540086,65.9467287033153,66.0351874963652,66.1235557087377,
66.2151120446125,66.3033786881694,66.3916320787869,66.4798935610554,66.5681844802327,
66.6565754658264,66.7450260541106,66.8336059788487,66.856006395736,66.9445795450427,
67.0330383380923,67.1214065504652,67.21296288634,67.3012295298969,67.3894829205143,
67.4777444027824,67.5660353219593,67.6544263075529,67.7428768958373,67.8314568205756,
67.8538572374634,67.9424303867701,68.0308891798198,68.1192573921924,68.2108137280672,
68.299080371624,68.3873337622413,68.4755952445098,68.5638861636865,68.65227714928,
68.740727737564,68.8293076623022,68.8517080791908,68.9402812284974,69.0287400215473,
69.1171082339198,69.2086645697946,69.2969312133513,69.3851846039687,69.4734460862368,
69.5617370054135,69.6501279910071,69.7385785792912,69.8271585040295,69.8495589209182,
69.9496992033075,70.0495090652108,70.1487062366456,70.2250835896641),
 .UNSPECIFIED.);
#1442=B_SPLINE_CURVE_WITH_KNOTS('',3,(#43208,#43209,#43210,#43211,#43212,
#43213,#43214,#43215,#43216,#43217,#43218,#43219,#43220,#43221,#43222,#43223,
#43224,#43225,#43226,#43227,#43228,#43229,#43230,#43231,#43232,#43233,#43234,
#43235,#43236,#43237,#43238,#43239,#43240,#43241,#43242,#43243,#43244,#43245,
#43246,#43247,#43248,#43249,#43250,#43251,#43252,#43253,#43254,#43255,#43256,
#43257,#43258,#43259,#43260,#43261,#43262,#43263,#43264,#43265,#43266,#43267,
#43268,#43269,#43270,#43271,#43272,#43273,#43274,#43275,#43276,#43277,#43278,
#43279,#43280,#43281,#43282,#43283,#43284,#43285,#43286,#43287,#43288,#43289,
#43290,#43291,#43292,#43293,#43294,#43295,#43296,#43297,#43298,#43299,#43300,
#43301,#43302,#43303,#43304,#43305,#43306,#43307,#43308,#43309,#43310,#43311,
#43312,#43313,#43314,#43315,#43316,#43317,#43318,#43319,#43320,#43321,#43322,
#43323,#43324,#43325,#43326,#43327,#43328,#43329,#43330,#43331,#43332,#43333,
#43334,#43335,#43336,#43337,#43338,#43339,#43340,#43341,#43342,#43343,#43344,
#43345,#43346,#43347,#43348,#43349,#43350,#43351,#43352,#43353,#43354,#43355,
#43356,#43357,#43358,#43359,#43360,#43361,#43362,#43363,#43364,#43365,#43366,
#43367,#43368,#43369,#43370,#43371,#43372,#43373,#43374,#43375,#43376,#43377,
#43378,#43379,#43380,#43381,#43382,#43383,#43384,#43385,#43386,#43387,#43388,
#43389,#43390,#43391,#43392,#43393,#43394,#43395,#43396,#43397,#43398,#43399,
#43400,#43401,#43402,#43403,#43404,#43405,#43406,#43407,#43408,#43409,#43410,
#43411,#43412,#43413,#43414,#43415,#43416,#43417,#43418,#43419,#43420,#43421,
#43422,#43423,#43424,#43425,#43426,#43427,#43428,#43429,#43430,#43431,#43432,
#43433),.UNSPECIFIED.,.F.,.F.,(4,3,3,3,3,3,3,3,3,3,3,3,3,3,3,3,3,3,3,3,
3,3,3,3,3,3,3,3,3,3,3,3,3,3,3,3,3,3,3,3,3,3,3,3,3,3,3,3,3,3,3,3,3,3,3,3,
3,3,3,3,3,3,3,3,3,3,3,3,3,3,3,3,3,3,3,4),(70.2250835898867,70.3140257139893,
70.4029773741118,70.4919588141696,70.5810544107307,70.6702073895624,70.7595248544884,
70.8474097626456,70.9359829119522,71.0244417050017,71.1128099173742,71.2043662532491,
71.2926328968058,71.380886287423,71.4691477696913,71.5574386888683,71.6458296744617,
71.734280262746,71.8228601874841,71.845260604373,71.9338337536797,72.0222925467294,
72.1106607591019,72.2022170949767,72.2904837385336,72.378737129151,72.4669986114194,
72.5552895305965,72.6436805161901,72.7321311044744,72.8207110292126,72.8431114461004,
72.931684595407,73.0201433884568,73.1085116008291,73.2000679367039,73.2883345802607,
73.3765879708781,73.4648494531464,73.5531403723234,73.6415313579169,73.7299819462011,
73.8185618709393,73.8409622878278,73.9295354371343,74.0179942301839,74.1063624425564,
74.1979187784313,74.2861854219881,74.3744388126054,74.4627002948738,74.550991214051,
74.6393821996444,74.7278327879286,74.8164127126668,74.8388131295552,74.9273862788618,
75.0158450719114,75.1042132842842,75.195769620159,75.2840362637158,75.3722896543332,
75.4605511366013,75.5488420557784,75.6372330413719,75.7256836296563,75.8142635543946,
75.8366639712826,75.9250774885633,76.0133803059622,76.1015940720834,76.1897403602781,
76.2778480053841,76.3659320489736,76.4540370202493,76.5082688970663),
 .UNSPECIFIED.);
#1443=B_SPLINE_CURVE_WITH_KNOTS('',3,(#43435,#43436,#43437,#43438,#43439,
#43440,#43441,#43442,#43443,#43444,#43445,#43446,#43447,#43448,#43449,#43450,
#43451,#43452,#43453,#43454,#43455,#43456,#43457,#43458,#43459,#43460,#43461,
#43462,#43463,#43464,#43465,#43466,#43467,#43468,#43469,#43470,#43471,#43472,
#43473,#43474,#43475,#43476,#43477,#43478,#43479,#43480,#43481,#43482,#43483,
#43484,#43485,#43486,#43487,#43488,#43489,#43490,#43491,#43492,#43493,#43494,
#43495,#43496,#43497,#43498,#43499,#43500,#43501,#43502,#43503,#43504,#43505,
#43506,#43507,#43508,#43509,#43510,#43511,#43512,#43513,#43514,#43515,#43516,
#43517,#43518,#43519,#43520,#43521,#43522,#43523,#43524,#43525,#43526,#43527,
#43528,#43529,#43530,#43531,#43532,#43533,#43534,#43535,#43536,#43537,#43538,
#43539,#43540,#43541,#43542,#43543,#43544,#43545,#43546,#43547,#43548,#43549,
#43550,#43551,#43552,#43553,#43554,#43555,#43556,#43557,#43558,#43559,#43560,
#43561,#43562,#43563,#43564,#43565,#43566,#43567,#43568,#43569,#43570,#43571,
#43572,#43573,#43574,#43575,#43576,#43577,#43578,#43579,#43580,#43581,#43582,
#43583,#43584,#43585,#43586,#43587,#43588,#43589,#43590,#43591,#43592,#43593,
#43594,#43595,#43596,#43597,#43598,#43599,#43600,#43601,#43602,#43603,#43604,
#43605,#43606,#43607,#43608,#43609,#43610,#43611,#43612,#43613,#43614,#43615,
#43616,#43617,#43618,#43619,#43620,#43621,#43622,#43623,#43624,#43625,#43626,
#43627,#43628,#43629,#43630,#43631,#43632,#43633,#43634,#43635,#43636,#43637,
#43638,#43639,#43640,#43641,#43642,#43643,#43644,#43645,#43646,#43647,#43648,
#43649,#43650,#43651,#43652,#43653,#43654,#43655,#43656,#43657,#43658,#43659,
#43660),.UNSPECIFIED.,.F.,.F.,(4,3,3,3,3,3,3,3,3,3,3,3,3,3,3,3,3,3,3,3,
3,3,3,3,3,3,3,3,3,3,3,3,3,3,3,3,3,3,3,3,3,3,3,3,3,3,3,3,3,3,3,3,3,3,3,3,
3,3,3,3,3,3,3,3,3,3,3,3,3,3,3,3,3,3,3,4),(76.5082688972673,76.6116784352087,
76.7157763021011,76.8206168958636,76.83451481301,76.9230879623167,77.0115467553667,
77.0999149677394,77.1914713036142,77.2797379471712,77.3679913377887,77.4562528200573,
77.5445437392345,77.6329347248282,77.7213853131125,77.8099652378508,77.8323656547374,
77.9209388040438,78.0093975970933,78.0977658094656,78.1893221453405,78.2775887888971,
78.3658421795142,78.4541036617823,78.5423945809592,78.6307855665524,78.7192361548364,
78.8078160795743,78.8302164964648,78.9187896457715,79.0072484388213,79.095616651194,
79.1871729870687,79.2754396306256,79.3636930212431,79.4519545035115,79.5402454226887,
79.6286364082823,79.7170869965666,79.8056669213049,79.8280673381922,79.9166404874989,
80.0050992805487,80.0934674929213,80.1850238287961,80.273290472353,80.3615438629704,
80.4498053452388,80.5380962644162,80.6264872500097,80.714937838294,80.8035177630323,
80.8259181799196,80.9144913292261,81.0029501222757,81.0913183346482,81.182874670523,
81.2711413140798,81.359394704697,81.4476561869652,81.5359471061422,81.6243380917357,
81.7127886800199,81.801368604758,81.823769021647,81.9119038818887,81.9999246913006,
82.0878557266216,82.1758055362963,82.2636390313494,82.3514605650463,82.4392919270503,
82.5273324962926,82.6152945515581,82.7034023713968,82.7914542040193),
 .UNSPECIFIED.);
#1444=B_SPLINE_CURVE_WITH_KNOTS('',3,(#43662,#43663,#43664,#43665,#43666,
#43667,#43668,#43669,#43670,#43671,#43672,#43673,#43674,#43675,#43676,#43677,
#43678,#43679,#43680,#43681,#43682,#43683,#43684,#43685,#43686,#43687,#43688,
#43689,#43690,#43691,#43692,#43693,#43694,#43695,#43696,#43697,#43698,#43699,
#43700,#43701,#43702,#43703,#43704,#43705,#43706,#43707,#43708,#43709,#43710,
#43711,#43712,#43713,#43714,#43715,#43716,#43717,#43718,#43719,#43720,#43721,
#43722,#43723,#43724,#43725,#43726,#43727,#43728,#43729,#43730,#43731,#43732,
#43733,#43734,#43735,#43736,#43737,#43738,#43739,#43740,#43741,#43742,#43743,
#43744,#43745,#43746,#43747,#43748,#43749,#43750,#43751,#43752,#43753,#43754,
#43755,#43756,#43757,#43758,#43759,#43760,#43761,#43762,#43763,#43764,#43765,
#43766,#43767,#43768,#43769,#43770,#43771,#43772,#43773,#43774,#43775,#43776,
#43777,#43778,#43779,#43780,#43781,#43782,#43783,#43784,#43785,#43786,#43787,
#43788,#43789,#43790,#43791,#43792,#43793,#43794,#43795,#43796,#43797,#43798,
#43799,#43800,#43801,#43802,#43803,#43804,#43805,#43806,#43807,#43808,#43809,
#43810,#43811,#43812,#43813,#43814,#43815,#43816,#43817,#43818,#43819,#43820,
#43821,#43822,#43823,#43824,#43825,#43826,#43827,#43828,#43829,#43830,#43831,
#43832,#43833,#43834,#43835,#43836,#43837,#43838,#43839,#43840,#43841,#43842,
#43843,#43844,#43845,#43846,#43847,#43848,#43849,#43850,#43851,#43852,#43853,
#43854,#43855,#43856,#43857,#43858,#43859,#43860,#43861,#43862,#43863,#43864,
#43865,#43866,#43867,#43868,#43869,#43870,#43871,#43872,#43873,#43874,#43875,
#43876,#43877,#43878,#43879,#43880,#43881,#43882,#43883,#43884,#43885,#43886,
#43887,#43888,#43889,#43890),.UNSPECIFIED.,.F.,.F.,(4,3,3,3,3,3,3,3,3,3,
3,3,3,3,3,3,3,3,3,3,3,3,3,3,3,3,3,3,3,3,3,3,3,3,3,3,3,3,3,3,3,3,3,3,3,3,
3,3,3,3,3,3,3,3,3,3,3,3,3,3,3,3,3,3,3,3,3,3,3,3,3,3,3,3,3,3,4),(82.7914542042459,
82.8216198633744,82.910193012681,82.9986518057306,83.0870200181033,83.1785763539781,
83.2668429975349,83.3550963881522,83.4433578704206,83.5316487895977,83.6200397751912,
83.7084903634754,83.7970702882137,83.8194707051018,83.9080438544085,83.9965026474585,
84.0848708598313,84.1764271957061,84.2646938392631,84.3529472298806,84.4412087121492,
84.5294996313266,84.6178906169202,84.7063412052046,84.794921129943,84.8173215468292,
84.9058946961358,84.9943534891854,85.082721701558,85.1742780374328,85.2625446809896,
85.3507980716068,85.4390595538751,85.5273504730522,85.6157414586456,85.7041920469298,
85.792771971668,85.8151723885566,85.9037455378633,85.9922043309131,86.0805725432857,
86.1721288791605,86.2603955227174,86.3486489133348,86.4369103956032,86.5252013147804,
86.613592300374,86.7020428886583,86.7906228133966,86.813023230284,86.9015963795905,
86.9900551726401,87.0784233850126,87.1699797208875,87.2582463644442,87.3464997550614,
87.4347612373296,87.5230521565066,87.6114431421,87.699893730384,87.7884736551221,
87.8108740720114,87.8994472213181,87.9879060143678,88.0762742267405,88.1678305626153,
88.2560972061722,88.3443505967895,88.4326120790578,88.5209029982349,88.6092939838285,
88.6977445721128,88.7863244968511,88.8087249137388,88.9216441128936,89.0325337049006,
89.0746395112596),.UNSPECIFIED.);
#1445=B_SPLINE_CURVE_WITH_KNOTS('',3,(#43892,#43893,#43894,#43895,#43896,
#43897,#43898,#43899,#43900,#43901,#43902,#43903,#43904,#43905,#43906,#43907,
#43908,#43909,#43910,#43911,#43912,#43913,#43914,#43915,#43916,#43917,#43918,
#43919,#43920,#43921,#43922,#43923,#43924,#43925,#43926,#43927,#43928,#43929,
#43930,#43931,#43932,#43933,#43934,#43935,#43936,#43937,#43938,#43939,#43940,
#43941,#43942,#43943,#43944,#43945,#43946,#43947,#43948,#43949,#43950,#43951,
#43952,#43953,#43954,#43955,#43956,#43957,#43958,#43959,#43960,#43961,#43962,
#43963,#43964,#43965,#43966,#43967,#43968,#43969,#43970,#43971,#43972,#43973,
#43974,#43975,#43976,#43977,#43978,#43979,#43980,#43981,#43982,#43983,#43984,
#43985,#43986,#43987,#43988,#43989,#43990,#43991,#43992,#43993,#43994,#43995,
#43996,#43997,#43998,#43999,#44000,#44001,#44002,#44003,#44004,#44005,#44006,
#44007,#44008,#44009,#44010,#44011,#44012,#44013,#44014,#44015,#44016,#44017,
#44018,#44019,#44020,#44021,#44022,#44023,#44024,#44025,#44026,#44027,#44028,
#44029,#44030,#44031,#44032,#44033,#44034,#44035,#44036,#44037,#44038,#44039,
#44040,#44041,#44042,#44043,#44044,#44045,#44046,#44047,#44048,#44049,#44050,
#44051,#44052,#44053,#44054,#44055,#44056,#44057,#44058,#44059,#44060,#44061,
#44062,#44063,#44064,#44065,#44066,#44067,#44068,#44069,#44070,#44071,#44072,
#44073,#44074,#44075,#44076,#44077,#44078,#44079,#44080,#44081,#44082,#44083,
#44084,#44085,#44086,#44087,#44088,#44089,#44090,#44091,#44092,#44093,#44094,
#44095,#44096,#44097,#44098,#44099,#44100,#44101,#44102,#44103,#44104,#44105,
#44106,#44107,#44108,#44109,#44110,#44111,#44112,#44113,#44114,#44115,#44116,
#44117,#44118,#44119,#44120),.UNSPECIFIED.,.F.,.F.,(4,3,3,3,3,3,3,3,3,3,
3,3,3,3,3,3,3,3,3,3,3,3,3,3,3,3,3,3,3,3,3,3,3,3,3,3,3,3,3,3,3,3,3,3,3,3,
3,3,3,3,3,3,3,3,3,3,3,3,3,3,3,3,3,3,3,3,3,3,3,3,3,3,3,3,3,3,4),(89.0746395114255,
89.1661315419306,89.2535335418103,89.3409155597642,89.4282997621432,89.5157083129216,
89.6032130314673,89.6907742923472,89.7784657067371,89.8065757554662,89.895148904773,
89.9836076978229,90.0719759101956,90.1635322460703,90.2517988896274,90.3400522802448,
90.428313762513,90.5166046816903,90.604995667284,90.6934462555685,90.7820261803069,
90.8044265971937,90.8929997465002,90.9814585395498,91.0698267519223,91.1613830877972,
91.249649731354,91.3379031219712,91.4261646042394,91.5144555234168,91.6028465090102,
91.6912970972945,91.7798770220327,91.8022774389211,91.8908505882277,91.9793093812776,
92.0676775936504,92.1592339295251,92.247500573082,92.3357539636995,92.4240154459681,
92.5123063651456,92.6006973507392,92.6891479390233,92.7777278637613,92.8001282806484,
92.8887014299549,92.9771602230045,93.0655284353775,93.1570847712523,93.2453514148092,
93.3336048054265,93.4218662876948,93.5101572068716,93.5985481924652,93.6869987807492,
93.7755787054873,93.7979791223758,93.8865522716825,93.9750110647324,94.0633792771048,
94.1549356129796,94.2432022565365,94.3314556471538,94.4197171294219,94.5080080485987,
94.5963990341921,94.6848496224764,94.7734295472146,94.7958299641032,94.8867065999349,
94.9774468352194,95.0725413310658,95.1630320672434,95.2534488825731,95.3437980500459,
95.3578248186051),.UNSPECIFIED.);
#1446=B_SPLINE_CURVE_WITH_KNOTS('',3,(#44122,#44123,#44124,#44125,#44126,
#44127,#44128,#44129,#44130,#44131,#44132,#44133,#44134,#44135,#44136,#44137,
#44138,#44139,#44140,#44141,#44142,#44143,#44144,#44145,#44146,#44147,#44148,
#44149,#44150,#44151,#44152,#44153,#44154,#44155,#44156,#44157,#44158,#44159,
#44160,#44161,#44162,#44163,#44164,#44165,#44166,#44167,#44168,#44169,#44170,
#44171,#44172,#44173,#44174,#44175,#44176,#44177,#44178,#44179,#44180,#44181,
#44182,#44183,#44184,#44185,#44186,#44187,#44188,#44189,#44190,#44191,#44192,
#44193,#44194,#44195,#44196,#44197,#44198,#44199,#44200,#44201,#44202,#44203,
#44204,#44205,#44206,#44207,#44208,#44209,#44210,#44211,#44212,#44213,#44214,
#44215,#44216,#44217,#44218,#44219,#44220,#44221,#44222,#44223,#44224,#44225,
#44226,#44227,#44228,#44229,#44230,#44231,#44232,#44233,#44234,#44235,#44236,
#44237,#44238,#44239,#44240,#44241,#44242,#44243,#44244,#44245,#44246,#44247,
#44248,#44249,#44250,#44251,#44252,#44253,#44254,#44255,#44256,#44257,#44258,
#44259,#44260,#44261,#44262,#44263,#44264,#44265,#44266,#44267,#44268,#44269,
#44270,#44271,#44272,#44273,#44274,#44275,#44276,#44277,#44278,#44279,#44280,
#44281,#44282,#44283,#44284,#44285,#44286,#44287,#44288,#44289,#44290,#44291,
#44292,#44293,#44294,#44295,#44296,#44297,#44298,#44299,#44300,#44301,#44302,
#44303,#44304,#44305,#44306,#44307,#44308,#44309,#44310,#44311,#44312,#44313,
#44314,#44315,#44316,#44317,#44318,#44319,#44320,#44321,#44322,#44323,#44324,
#44325,#44326,#44327,#44328,#44329,#44330,#44331,#44332,#44333,#44334,#44335,
#44336,#44337,#44338,#44339,#44340,#44341,#44342,#44343,#44344,#44345,#44346,
#44347),.UNSPECIFIED.,.F.,.F.,(4,3,3,3,3,3,3,3,3,3,3,3,3,3,3,3,3,3,3,3,
3,3,3,3,3,3,3,3,3,3,3,3,3,3,3,3,3,3,3,3,3,3,3,3,3,3,3,3,3,3,3,3,3,3,3,3,
3,3,3,3,3,3,3,3,3,3,3,3,3,3,3,3,3,3,3,4),(95.3578248187554,95.4530925370813,
95.5487521534953,95.6446140067219,95.7407816715538,95.7936808058306,95.8822539551371,
95.9707127481868,96.0590809605592,96.1506372964341,96.2389039399908,96.3271573306081,
96.4154188128763,96.5037097320534,96.5921007176468,96.680551305931,96.7691312306691,
96.791531647558,96.8801047968644,96.968563589914,97.0569318022864,97.1484881381613,
97.2367547817179,97.325008172335,97.4132696546032,97.5015605737801,97.5899515593734,
97.6784021476575,97.7669820723955,97.7893824892855,97.8779556385931,97.9664144316439,
98.0547826440175,98.1463389798919,98.2346056234498,98.3228590140681,98.4111204963375,
98.4994114155156,98.5878024011101,98.6762529893954,98.7648329141346,98.7872333310129,
98.8758064803179,98.9642652733661,99.0526334857372,99.1441898216126,99.2324564651679,
99.3207098557838,99.4089713380506,99.4972622572263,99.5856532428184,99.6741038311011,
99.762683755838,99.7850841727403,99.8736573220461,99.962116115095,100.050484327467,
100.142040663342,100.230307306898,100.318560697514,100.406822179782,100.495113098958,
100.58350408455,100.671954672834,100.760534597571,100.782935014468,100.870225958326,
100.957403438561,101.044482974272,101.131508277622,101.218501858615,101.305486194025,
101.392527562315,101.479596613056,101.566780277413,101.641010125573),
 .UNSPECIFIED.);
#1447=B_SPLINE_CURVE_WITH_KNOTS('',3,(#44349,#44350,#44351,#44352,#44353,
#44354,#44355,#44356,#44357,#44358,#44359,#44360,#44361,#44362,#44363,#44364,
#44365,#44366,#44367,#44368,#44369,#44370,#44371,#44372,#44373,#44374,#44375,
#44376,#44377,#44378,#44379,#44380,#44381,#44382,#44383,#44384,#44385,#44386,
#44387,#44388,#44389,#44390,#44391,#44392,#44393,#44394,#44395,#44396,#44397,
#44398,#44399,#44400,#44401,#44402,#44403,#44404,#44405,#44406,#44407,#44408,
#44409,#44410,#44411,#44412,#44413,#44414,#44415,#44416,#44417,#44418,#44419,
#44420,#44421,#44422,#44423,#44424,#44425,#44426,#44427,#44428,#44429,#44430,
#44431,#44432,#44433,#44434,#44435,#44436,#44437,#44438,#44439,#44440,#44441,
#44442,#44443,#44444,#44445,#44446,#44447,#44448,#44449,#44450,#44451,#44452,
#44453,#44454,#44455,#44456,#44457,#44458,#44459,#44460,#44461,#44462,#44463,
#44464,#44465,#44466,#44467,#44468,#44469,#44470,#44471,#44472,#44473,#44474,
#44475,#44476,#44477,#44478,#44479,#44480,#44481,#44482,#44483,#44484,#44485,
#44486,#44487,#44488,#44489,#44490,#44491,#44492,#44493,#44494,#44495,#44496,
#44497,#44498,#44499,#44500,#44501,#44502,#44503,#44504,#44505,#44506,#44507,
#44508,#44509,#44510,#44511,#44512,#44513,#44514,#44515,#44516,#44517,#44518,
#44519,#44520,#44521,#44522,#44523,#44524,#44525,#44526,#44527,#44528,#44529,
#44530,#44531,#44532,#44533,#44534,#44535,#44536,#44537,#44538,#44539,#44540,
#44541,#44542,#44543,#44544,#44545,#44546,#44547,#44548,#44549,#44550,#44551,
#44552,#44553,#44554,#44555,#44556,#44557,#44558,#44559,#44560,#44561,#44562,
#44563,#44564,#44565,#44566,#44567,#44568,#44569,#44570,#44571,#44572,#44573,
#44574),.UNSPECIFIED.,.F.,.F.,(4,3,3,3,3,3,3,3,3,3,3,3,3,3,3,3,3,3,3,3,
3,3,3,3,3,3,3,3,3,3,3,3,3,3,3,3,3,3,3,3,3,3,3,3,3,3,3,3,3,3,3,3,3,3,3,3,
3,3,3,3,3,3,3,3,3,3,3,3,3,3,3,3,3,3,3,4),(101.641010125785,101.780785856195,
101.869359005486,101.957817798521,102.046186010879,102.137742346759,102.226008990301,
102.314262380904,102.402523863157,102.49081478232,102.579205767899,102.667656356169,
102.756236280894,102.778636697922,102.867209847227,102.955668640276,103.044036852647,
103.135593188522,103.223859832077,103.312113222692,103.400374704959,103.488665624134,
103.577056609725,103.665507198006,103.754087122742,103.77648753965,103.865060689027,
103.953519482148,104.041887694592,104.13344403044,104.221710674068,104.309964064756,
104.398225547095,104.486516466342,104.574907452005,104.663358040359,104.751937965165,
104.774338381377,104.86291153053,104.951370323427,105.039738535647,105.131294871579,
105.219561514985,105.307814905453,105.396076387572,105.484367306602,105.57275829205,
105.661208880191,105.749788804788,105.772189223105,105.860762372451,105.949221165538,
106.037589377947,106.129145713808,106.217412357397,106.305665748046,106.393927230345,
106.48221814955,106.57060913517,106.659059723479,106.74763964824,106.770040064832,
106.85861321471,106.947072008333,107.03544022128,107.12699655694,107.215263201072,
107.303516592264,107.391778075105,107.480068994853,107.568459981011,107.656910569858,
107.745490495149,107.767890906559,107.913755939669,107.924195432964),
 .UNSPECIFIED.);
#1448=B_SPLINE_CURVE_WITH_KNOTS('',3,(#44576,#44577,#44578,#44579,#44580,
#44581,#44582,#44583,#44584,#44585,#44586,#44587,#44588,#44589,#44590,#44591,
#44592,#44593,#44594,#44595,#44596,#44597,#44598,#44599,#44600,#44601,#44602,
#44603,#44604,#44605,#44606,#44607,#44608,#44609,#44610,#44611,#44612,#44613,
#44614,#44615,#44616,#44617,#44618,#44619,#44620,#44621,#44622,#44623,#44624,
#44625,#44626,#44627,#44628,#44629,#44630,#44631,#44632,#44633,#44634,#44635,
#44636,#44637,#44638,#44639,#44640,#44641,#44642,#44643,#44644,#44645,#44646,
#44647,#44648,#44649,#44650,#44651,#44652,#44653,#44654,#44655,#44656,#44657,
#44658,#44659,#44660,#44661,#44662,#44663,#44664,#44665,#44666,#44667,#44668,
#44669,#44670,#44671,#44672,#44673,#44674,#44675,#44676,#44677,#44678,#44679,
#44680,#44681,#44682,#44683,#44684,#44685,#44686,#44687,#44688,#44689,#44690,
#44691,#44692,#44693,#44694,#44695,#44696,#44697,#44698,#44699,#44700,#44701,
#44702,#44703,#44704,#44705,#44706,#44707,#44708,#44709,#44710,#44711,#44712,
#44713,#44714,#44715,#44716,#44717,#44718,#44719,#44720,#44721,#44722,#44723,
#44724,#44725,#44726,#44727,#44728,#44729,#44730,#44731,#44732,#44733,#44734,
#44735,#44736,#44737,#44738,#44739,#44740,#44741,#44742,#44743,#44744,#44745,
#44746,#44747,#44748,#44749,#44750,#44751,#44752,#44753,#44754,#44755,#44756,
#44757,#44758,#44759,#44760,#44761,#44762,#44763,#44764,#44765,#44766,#44767,
#44768,#44769,#44770,#44771,#44772,#44773,#44774,#44775,#44776,#44777,#44778,
#44779,#44780,#44781,#44782,#44783,#44784,#44785,#44786,#44787,#44788,#44789,
#44790,#44791,#44792,#44793,#44794,#44795,#44796,#44797,#44798,#44799,#44800,
#44801),.UNSPECIFIED.,.F.,.F.,(4,3,3,3,3,3,3,3,3,3,3,3,3,3,3,3,3,3,3,3,
3,3,3,3,3,3,3,3,3,3,3,3,3,3,3,3,3,3,3,3,3,3,3,3,3,3,3,3,3,3,3,3,3,3,3,3,
3,3,3,3,3,3,3,3,3,3,3,3,3,3,3,3,3,3,3,4),(107.92419543315,108.01134635584,
108.098408190689,108.185408317907,108.272376689573,108.359335804232,108.44630814868,
108.533368394491,108.620475838792,108.70771891813,108.765741748287,108.854314898402,
108.942773692249,109.031141905407,109.122698240983,109.21096488529,109.299218276644,
109.387479759634,109.475770679517,109.564161665791,109.65261225474,109.741192180117,
109.763592590014,109.852165743744,109.940624541239,110.028992758074,110.120549092283,
110.208815740317,110.29706913541,110.385330622146,110.473621545779,110.562012535788,
110.650463128471,110.739043057546,110.761443431742,110.85001656763,110.938475347259,
111.026843546225,111.11839988713,111.206666517397,111.294919894789,111.383181363912,
111.471472270038,111.559863242783,111.648313818323,111.736893730565,111.759294273469,
111.847867433928,111.936326238037,112.024694461365,112.116250793094,112.204517447281,
112.292770848391,112.381032341004,112.469323270367,112.557714265861,112.646164863892,
112.734744798077,112.757145115197,112.845718297108,112.93417712298,113.022545368351,
113.114101691923,113.202368368707,113.290621792579,113.378883308092,113.467174260469,
113.555565279028,113.64401590018,113.732595857391,113.754995956924,113.850302064542,
113.945297709924,114.040103513436,114.134621615787,114.207380739913),
 .UNSPECIFIED.);
#1449=B_SPLINE_CURVE_WITH_KNOTS('',3,(#44803,#44804,#44805,#44806,#44807,
#44808,#44809,#44810,#44811,#44812,#44813,#44814,#44815,#44816,#44817,#44818,
#44819,#44820,#44821,#44822,#44823,#44824,#44825,#44826,#44827,#44828,#44829,
#44830,#44831,#44832,#44833,#44834,#44835,#44836,#44837,#44838,#44839,#44840,
#44841,#44842,#44843,#44844,#44845,#44846,#44847,#44848,#44849,#44850,#44851,
#44852,#44853,#44854,#44855,#44856,#44857,#44858,#44859,#44860,#44861,#44862,
#44863,#44864,#44865,#44866,#44867,#44868,#44869,#44870,#44871,#44872,#44873,
#44874,#44875,#44876,#44877,#44878,#44879,#44880,#44881,#44882,#44883,#44884,
#44885,#44886,#44887,#44888,#44889,#44890,#44891,#44892,#44893,#44894,#44895,
#44896,#44897,#44898,#44899,#44900,#44901,#44902,#44903,#44904,#44905,#44906,
#44907,#44908,#44909,#44910,#44911,#44912,#44913,#44914,#44915,#44916,#44917,
#44918,#44919,#44920,#44921,#44922,#44923,#44924,#44925,#44926,#44927,#44928,
#44929,#44930,#44931,#44932,#44933,#44934,#44935,#44936,#44937,#44938,#44939,
#44940,#44941,#44942,#44943,#44944,#44945,#44946,#44947,#44948,#44949,#44950,
#44951,#44952,#44953,#44954,#44955,#44956,#44957,#44958,#44959,#44960,#44961,
#44962,#44963,#44964,#44965,#44966,#44967,#44968,#44969,#44970,#44971,#44972,
#44973,#44974,#44975,#44976,#44977,#44978,#44979,#44980,#44981,#44982,#44983,
#44984,#44985,#44986,#44987,#44988,#44989,#44990,#44991,#44992,#44993,#44994,
#44995,#44996,#44997,#44998,#44999,#45000,#45001,#45002,#45003,#45004,#45005,
#45006,#45007,#45008,#45009,#45010,#45011,#45012,#45013,#45014,#45015,#45016,
#45017,#45018,#45019,#45020,#45021,#45022,#45023,#45024,#45025,#45026,#45027,
#45028),.UNSPECIFIED.,.F.,.F.,(4,3,3,3,3,3,3,3,3,3,3,3,3,3,3,3,3,3,3,3,
3,3,3,3,3,3,3,3,3,3,3,3,3,3,3,3,3,3,3,3,3,3,3,3,3,3,3,3,3,3,3,3,3,3,3,3,
3,3,3,3,3,3,3,3,3,3,3,3,3,3,3,3,3,3,3,4),(114.207380740144,114.29822902319,
114.389148151898,114.480233973373,114.571404209436,114.662772777588,114.752846798651,
114.841420080294,114.929879004949,115.018247348053,115.109803634594,115.198070405915,
115.286323922988,115.374585530273,115.462876572899,115.551267679009,115.639718386248,
115.728298426754,115.750697640379,115.83927101322,115.92773003184,116.016098471528,
116.10765472285,116.195921596597,116.284175218065,116.372436931593,116.460728082187,
116.549119298247,116.637570116725,116.726150269473,116.748548482106,116.837120560223,
116.925578280648,117.013945420227,117.105502158178,117.193767735238,117.282020063494,
117.370280488661,117.458570357127,117.546960306742,117.635409866374,117.723988781068,
117.746399323834,117.834973920296,117.923434154979,118.011803801864,118.103359597326,
118.191627648883,118.27988243536,118.368145299902,118.456437586308,118.544829910087,
118.63328182126,118.721863036437,118.744250165561,118.832824666255,118.921284829279,
119.009654428358,119.101210250725,119.189478313511,119.277733132867,119.365996051797,
119.454288413975,119.542680844513,119.631132880622,119.719714246125,119.742101007288,
119.829657712105,119.917073105115,120.004407658741,120.091683759538,120.17892373707,
120.266174310352,120.353429477391,120.44074933614,120.490566047323),
 .UNSPECIFIED.);
#1450=B_SPLINE_CURVE_WITH_KNOTS('',3,(#45030,#45031,#45032,#45033,#45034,
#45035,#45036,#45037,#45038,#45039,#45040,#45041,#45042,#45043,#45044,#45045,
#45046,#45047,#45048,#45049,#45050,#45051,#45052,#45053,#45054,#45055,#45056,
#45057,#45058,#45059,#45060,#45061,#45062,#45063,#45064,#45065,#45066,#45067,
#45068,#45069,#45070,#45071,#45072,#45073,#45074,#45075,#45076,#45077,#45078,
#45079,#45080,#45081,#45082,#45083,#45084,#45085,#45086,#45087,#45088,#45089,
#45090,#45091,#45092,#45093,#45094,#45095,#45096,#45097,#45098,#45099,#45100,
#45101,#45102,#45103,#45104,#45105,#45106,#45107,#45108,#45109,#45110,#45111,
#45112,#45113,#45114,#45115,#45116,#45117,#45118,#45119,#45120,#45121,#45122,
#45123,#45124,#45125,#45126,#45127,#45128,#45129,#45130,#45131,#45132,#45133,
#45134,#45135,#45136,#45137,#45138,#45139,#45140,#45141,#45142,#45143,#45144,
#45145,#45146,#45147,#45148,#45149,#45150,#45151,#45152,#45153,#45154,#45155,
#45156,#45157,#45158,#45159,#45160,#45161,#45162,#45163,#45164,#45165,#45166,
#45167,#45168,#45169,#45170,#45171,#45172,#45173,#45174,#45175,#45176,#45177,
#45178,#45179,#45180,#45181,#45182,#45183,#45184,#45185,#45186,#45187,#45188,
#45189,#45190,#45191,#45192,#45193,#45194,#45195,#45196,#45197,#45198,#45199,
#45200,#45201,#45202,#45203,#45204,#45205,#45206,#45207,#45208,#45209,#45210,
#45211,#45212,#45213,#45214,#45215,#45216),.UNSPECIFIED.,.F.,.F.,(4,3,3,
3,3,3,3,3,3,3,3,3,3,3,3,3,3,3,3,3,3,3,3,3,3,3,3,3,3,3,3,3,3,3,3,3,3,3,3,
3,3,3,3,3,3,3,3,3,3,3,3,3,3,3,3,3,3,3,3,3,3,3,4),(120.490566047475,120.603855612386,
120.71971094167,120.739951849016,120.828540004253,120.917013763895,121.005396886632,
121.096947612146,121.185228934143,121.273496892886,121.361772817757,121.450078038697,
121.538483046463,121.626947510997,121.71554099275,121.737802690743,121.826381914761,
121.914846948535,122.003221558057,122.094775554858,122.183048940626,122.271309188573,
122.359577635319,122.447875618222,122.536273777125,122.624731611222,122.71331883065,
122.735653532471,122.824148713268,122.912529337165,123.000819272197,123.092404909948,
123.180593494166,123.268769036965,123.356952964635,123.44516670444,123.533481453563,
123.621856260651,123.710361654286,123.733504374198,123.822227114771,123.910835247245,
123.999352372869,124.090852728251,124.179266286799,124.26766559985,124.356071855323,
124.444506240839,124.533038041216,124.621628064168,124.710344348404,124.731355215925,
124.81905048528,124.90663353371,124.994129052871,125.081564029985,125.168967928638,
125.256362918329,125.343771156934,125.431265942597,125.518807433168,125.606481900134,
125.663325063941),.UNSPECIFIED.);
#1451=B_SPLINE_CURVE_WITH_KNOTS('',3,(#45220,#45221,#45222,#45223,#45224,
#45225,#45226,#45227),.UNSPECIFIED.,.F.,.F.,(4,1,1,1,1,4),(-127.724907741108,
-126.72705689938,-125.729206057653,-124.731355215925,-123.733504374198,
-123.473272362321),.UNSPECIFIED.);
#1452=B_SPLINE_CURVE_WITH_KNOTS('',3,(#45229,#45230,#45231,#45232,#45233,
#45234,#45235,#45236,#45237,#45238,#45239,#45240,#45241,#45242,#45243,#45244,
#45245,#45246,#45247,#45248,#45249,#45250,#45251,#45252,#45253,#45254,#45255,
#45256,#45257,#45258,#45259,#45260,#45261,#45262,#45263,#45264,#45265,#45266,
#45267,#45268,#45269,#45270,#45271,#45272,#45273,#45274,#45275,#45276,#45277,
#45278,#45279,#45280,#45281,#45282,#45283,#45284,#45285,#45286,#45287,#45288,
#45289,#45290,#45291,#45292,#45293,#45294,#45295,#45296,#45297,#45298,#45299,
#45300,#45301,#45302,#45303,#45304,#45305,#45306,#45307,#45308,#45309,#45310,
#45311,#45312,#45313,#45314,#45315,#45316,#45317,#45318,#45319,#45320,#45321,
#45322,#45323,#45324,#45325,#45326,#45327,#45328,#45329,#45330,#45331,#45332,
#45333,#45334,#45335,#45336,#45337,#45338,#45339,#45340,#45341,#45342,#45343,
#45344,#45345,#45346,#45347,#45348,#45349,#45350,#45351,#45352,#45353,#45354,
#45355,#45356,#45357,#45358,#45359,#45360,#45361,#45362,#45363,#45364,#45365,
#45366,#45367,#45368,#45369,#45370,#45371,#45372,#45373,#45374,#45375,#45376,
#45377,#45378,#45379,#45380,#45381,#45382,#45383,#45384,#45385,#45386,#45387,
#45388,#45389,#45390,#45391,#45392,#45393,#45394,#45395,#45396,#45397,#45398,
#45399,#45400,#45401,#45402,#45403,#45404,#45405,#45406,#45407,#45408,#45409,
#45410,#45411,#45412,#45413,#45414,#45415,#45416,#45417,#45418,#45419,#45420,
#45421,#45422,#45423,#45424,#45425,#45426,#45427,#45428,#45429,#45430,#45431,
#45432,#45433,#45434,#45435,#45436,#45437,#45438,#45439,#45440,#45441,#45442,
#45443,#45444,#45445,#45446,#45447,#45448,#45449,#45450,#45451,#45452,#45453,
#45454),.UNSPECIFIED.,.F.,.F.,(4,3,3,3,3,3,3,3,3,3,3,3,3,3,3,3,3,3,3,3,
3,3,3,3,3,3,3,3,3,3,3,3,3,3,3,3,3,3,3,3,3,3,3,3,3,3,3,3,3,3,3,3,3,3,3,3,
3,3,3,3,3,3,3,3,3,3,3,3,3,3,3,3,3,3,3,4),(-123.473269876606,-123.38591924059,
-123.298617101219,-123.211338154408,-123.124060152026,-123.036760850702,
-122.949367056308,-122.861919316573,-122.774338602659,-122.735653532471,
-122.647073127485,-122.558607139165,-122.470231800566,-122.378678161838,
-122.290404612489,-122.202144410105,-122.113876218018,-122.025578698975,
-121.9371813111,-121.848724428107,-121.760138415471,-121.737802690743,-121.649216030073,
-121.560743479549,-121.472361281677,-121.380810102595,-121.292528992542,
-121.204260982044,-121.115984741777,-121.027678941658,-120.939272967411,
-120.850807309327,-120.762212311637,-120.739951849016,-120.6513874492,-120.562937519873,
-120.474578274038,-120.383018615694,-120.294761138282,-120.206516971966,
-120.118264762376,-120.029983154502,-119.941601490546,-119.853160241319,
-119.764589609245,-119.742101007288,-119.65352642391,-119.565066194115,
-119.47669654411,-119.385140746791,-119.29687267282,-119.208617856976,-119.120354956251,
-119.032062626978,-118.943670250929,-118.855218281961,-118.766637001566,
-118.744250165561,-118.65567573012,-118.567215625718,-118.478846078501,
-118.387290234168,-118.299022205494,-118.210767413502,-118.122504515054,
-118.034212166333,-117.945819738524,-117.857367698867,-117.768786320475,
-117.746399323834,-117.655350362726,-117.564439993407,-117.470851137412,
-117.380195982519,-117.285140275973,-117.190084569427),.UNSPECIFIED.);
#1453=B_SPLINE_CURVE_WITH_KNOTS('',3,(#45456,#45457,#45458,#45459,#45460,
#45461,#45462,#45463,#45464,#45465,#45466,#45467,#45468,#45469,#45470,#45471,
#45472,#45473,#45474,#45475,#45476,#45477,#45478,#45479,#45480,#45481,#45482,
#45483,#45484,#45485,#45486,#45487,#45488,#45489,#45490,#45491,#45492,#45493,
#45494,#45495,#45496,#45497,#45498,#45499,#45500,#45501,#45502,#45503,#45504,
#45505,#45506,#45507,#45508,#45509,#45510,#45511,#45512,#45513,#45514,#45515,
#45516,#45517,#45518,#45519,#45520,#45521,#45522,#45523,#45524,#45525,#45526,
#45527,#45528,#45529,#45530,#45531,#45532,#45533,#45534,#45535,#45536,#45537,
#45538,#45539,#45540,#45541,#45542,#45543,#45544,#45545,#45546,#45547,#45548,
#45549,#45550,#45551,#45552,#45553,#45554,#45555,#45556,#45557,#45558,#45559,
#45560,#45561,#45562,#45563,#45564,#45565,#45566,#45567,#45568,#45569,#45570,
#45571,#45572,#45573,#45574,#45575,#45576,#45577,#45578,#45579,#45580,#45581,
#45582,#45583,#45584,#45585,#45586,#45587,#45588,#45589,#45590,#45591,#45592,
#45593,#45594,#45595,#45596,#45597,#45598,#45599,#45600,#45601,#45602,#45603,
#45604,#45605,#45606,#45607,#45608,#45609,#45610,#45611,#45612,#45613,#45614,
#45615,#45616,#45617,#45618,#45619,#45620,#45621,#45622,#45623,#45624,#45625,
#45626,#45627,#45628,#45629,#45630,#45631,#45632,#45633,#45634,#45635,#45636,
#45637,#45638,#45639,#45640,#45641,#45642,#45643,#45644,#45645,#45646,#45647,
#45648,#45649,#45650,#45651,#45652,#45653,#45654,#45655,#45656,#45657,#45658,
#45659,#45660,#45661,#45662,#45663,#45664,#45665,#45666,#45667,#45668,#45669,
#45670,#45671,#45672,#45673,#45674,#45675,#45676,#45677,#45678,#45679,#45680,
#45681),.UNSPECIFIED.,.F.,.F.,(4,3,3,3,3,3,3,3,3,3,3,3,3,3,3,3,3,3,3,3,
3,3,3,3,3,3,3,3,3,3,3,3,3,3,3,3,3,3,3,3,3,3,3,3,3,3,3,3,3,3,3,3,3,3,3,3,
3,3,3,3,3,3,3,3,3,3,3,3,3,3,3,3,3,3,3,4),(-117.190084569288,-117.095110346029,
-116.99976205911,-116.904221663067,-116.808380876812,-116.748548482106,
-116.659975105794,-116.571516084384,-116.483147642584,-116.391591392309,
-116.30332451815,-116.215070896898,-116.126809184213,-116.038518035092,
-115.950126821426,-115.861676005884,-115.773095856839,-115.750697640379,
-115.662124375681,-115.573665464735,-115.485297132119,-115.393740840436,
-115.305474071525,-115.217220553873,-115.128958943021,-115.04066789384,
-114.952276776786,-114.863826056029,-114.775245998352,-114.752846798651,
-114.664273762505,-114.57581508424,-114.487446988128,-114.395890609228,
-114.307624084878,-114.219370814354,-114.131109452938,-114.042818655246,
-113.954427791465,-113.865977325332,-113.777397522303,-113.754995956924,
-113.666422775285,-113.577963949636,-113.489595704438,-113.398039380783,
-113.309772704049,-113.221519280182,-113.133257764627,-113.044966812163,
-112.956575793451,-112.868125172106,-112.779545214647,-112.757145115197,
-112.668571956472,-112.580113153765,-112.491744931509,-112.400188599254,
-112.311921945313,-112.223668544144,-112.135407051166,-112.047116121132,
-111.958725124518,-111.870274525103,-111.78169458916,-111.759294273469,
-111.672016516612,-111.584852262681,-111.497786145448,-111.410774318335,
-111.323794262059,-111.236823490763,-111.149796935836,-111.062742663134,
-110.975577012017,-110.906899262451),.UNSPECIFIED.);
#1454=B_SPLINE_CURVE_WITH_KNOTS('',3,(#45683,#45684,#45685,#45686,#45687,
#45688,#45689,#45690,#45691,#45692,#45693,#45694,#45695,#45696,#45697,#45698,
#45699,#45700,#45701,#45702,#45703,#45704,#45705,#45706,#45707,#45708,#45709,
#45710,#45711,#45712,#45713,#45714,#45715,#45716,#45717,#45718,#45719,#45720,
#45721,#45722,#45723,#45724,#45725,#45726,#45727,#45728,#45729,#45730,#45731,
#45732,#45733,#45734,#45735,#45736,#45737,#45738,#45739,#45740,#45741,#45742,
#45743,#45744,#45745,#45746,#45747,#45748,#45749,#45750,#45751,#45752,#45753,
#45754,#45755,#45756,#45757,#45758,#45759,#45760,#45761,#45762,#45763,#45764,
#45765,#45766,#45767,#45768,#45769,#45770,#45771,#45772,#45773,#45774,#45775,
#45776,#45777,#45778,#45779,#45780,#45781,#45782,#45783,#45784,#45785,#45786,
#45787,#45788,#45789,#45790,#45791,#45792,#45793,#45794,#45795,#45796,#45797,
#45798,#45799,#45800,#45801,#45802,#45803,#45804,#45805,#45806,#45807,#45808,
#45809,#45810,#45811,#45812,#45813,#45814,#45815,#45816,#45817,#45818,#45819,
#45820,#45821,#45822,#45823,#45824,#45825,#45826,#45827,#45828,#45829,#45830,
#45831,#45832,#45833,#45834,#45835,#45836,#45837,#45838,#45839,#45840,#45841,
#45842,#45843,#45844,#45845,#45846,#45847,#45848,#45849,#45850,#45851,#45852,
#45853,#45854,#45855,#45856,#45857,#45858,#45859,#45860,#45861,#45862,#45863,
#45864,#45865,#45866,#45867,#45868,#45869,#45870,#45871,#45872,#45873,#45874,
#45875,#45876,#45877,#45878,#45879,#45880,#45881,#45882,#45883,#45884,#45885,
#45886,#45887,#45888,#45889,#45890,#45891,#45892,#45893,#45894,#45895,#45896,
#45897,#45898,#45899,#45900,#45901,#45902,#45903,#45904,#45905),
 .UNSPECIFIED.,.F.,.F.,(4,3,3,3,3,3,3,3,3,3,3,3,3,3,3,3,3,3,3,3,3,3,3,3,
3,3,3,3,3,3,3,3,3,3,3,3,3,3,3,3,3,3,3,3,3,3,3,3,3,3,3,3,3,3,3,3,3,3,3,3,
3,3,3,3,3,3,3,3,3,3,3,3,3,3,4),(-110.906899262247,-110.761443431742,-110.672870278115,
-110.584411480703,-110.496043263931,-110.404486929691,-110.316220281672,
-110.227966886576,-110.139705399819,-110.051414476147,-109.963023486072,
-109.874572893308,-109.78599296413,-109.763592590014,-109.67501944007,-109.586560646362,
-109.498192433311,-109.406636097683,-109.3183694534,-109.23011606204,-109.141854579015,
-109.053563659065,-108.965172672681,-108.876722083595,-108.788142158044,
-108.765741748287,-108.677168600319,-108.588709808628,-108.500341597634,
-108.40878526125,-108.320518619111,-108.232265229923,-108.144003749096,
-108.055712831368,-107.967321847231,-107.878871260408,-107.790291337127,
-107.767890906559,-107.679317756701,-107.590858963093,-107.502490750157,
-107.410934414492,-107.322667770362,-107.23441437917,-107.146152896324,
-107.057861976568,-106.969470990397,-106.881020401535,-106.792440476223,
-106.770040064832,-106.681466915503,-106.593008122429,-106.50463991003,
-106.413083574164,-106.324816930577,-106.236563539929,-106.148302057627,
-106.060011138416,-105.971620152786,-105.883169564464,-105.794589639687,
-105.772189223105,-105.683616073939,-105.595157281031,-105.506789068803,
-105.415232732875,-105.326966089467,-105.238712699,-105.150451216883,-105.062160297859,
-104.973769312418,-104.885318724288,-104.796738799704,-104.774338381377,
-104.623713955068),.UNSPECIFIED.);
#1455=B_SPLINE_CURVE_WITH_KNOTS('',3,(#45907,#45908,#45909,#45910,#45911,
#45912,#45913,#45914,#45915,#45916,#45917,#45918,#45919,#45920,#45921,#45922,
#45923,#45924,#45925,#45926,#45927,#45928,#45929,#45930,#45931,#45932,#45933,
#45934,#45935,#45936,#45937,#45938,#45939,#45940,#45941,#45942,#45943,#45944,
#45945,#45946,#45947,#45948,#45949,#45950,#45951,#45952,#45953,#45954,#45955,
#45956,#45957,#45958,#45959,#45960,#45961,#45962,#45963,#45964,#45965,#45966,
#45967,#45968,#45969,#45970,#45971,#45972,#45973,#45974,#45975,#45976,#45977,
#45978,#45979,#45980,#45981,#45982,#45983,#45984,#45985,#45986,#45987,#45988,
#45989,#45990,#45991,#45992,#45993,#45994,#45995,#45996,#45997,#45998,#45999,
#46000,#46001,#46002,#46003,#46004,#46005,#46006,#46007,#46008,#46009,#46010,
#46011,#46012,#46013,#46014,#46015,#46016,#46017,#46018,#46019,#46020,#46021,
#46022,#46023,#46024,#46025,#46026,#46027,#46028,#46029,#46030,#46031,#46032,
#46033,#46034,#46035,#46036,#46037,#46038,#46039,#46040,#46041,#46042,#46043,
#46044,#46045,#46046,#46047,#46048,#46049,#46050,#46051,#46052,#46053,#46054,
#46055,#46056,#46057,#46058,#46059,#46060,#46061,#46062,#46063,#46064,#46065,
#46066,#46067,#46068,#46069,#46070,#46071,#46072,#46073,#46074,#46075,#46076,
#46077,#46078,#46079,#46080,#46081,#46082,#46083,#46084,#46085,#46086,#46087,
#46088,#46089,#46090,#46091,#46092,#46093,#46094,#46095,#46096,#46097,#46098,
#46099,#46100,#46101,#46102,#46103,#46104,#46105,#46106,#46107,#46108,#46109,
#46110,#46111,#46112,#46113,#46114,#46115,#46116,#46117,#46118,#46119,#46120,
#46121,#46122,#46123,#46124,#46125,#46126,#46127,#46128,#46129,#46130,#46131,
#46132),.UNSPECIFIED.,.F.,.F.,(4,3,3,3,3,3,3,3,3,3,3,3,3,3,3,3,3,3,3,3,
3,3,3,3,3,3,3,3,3,3,3,3,3,3,3,3,3,3,3,3,3,3,3,3,3,3,3,3,3,3,3,3,3,3,3,3,
3,3,3,3,3,3,3,3,3,3,3,3,3,3,3,3,3,3,3,4),(-104.623713954873,-104.536549056533,
-104.449474776175,-104.362464266208,-104.275486898148,-104.188520177306,
-104.101541622016,-104.014475919247,-103.927364282644,-103.840115392771,
-103.77648753965,-103.687914390346,-103.599455597299,-103.511087384929,
-103.419531049053,-103.331264405498,-103.243011014883,-103.154749532617,
-103.066458613441,-102.978067627849,-102.889617039567,-102.80103711483,
-102.778636697922,-102.69006354863,-102.601604755595,-102.513236543237,
-102.421680207357,-102.333413563815,-102.245160173213,-102.156898690961,
-102.0686077718,-101.980216786222,-101.891766197954,-101.803186273231,-101.780785856195,
-101.69221270688,-101.603753913822,-101.515385701442,-101.42382936557,-101.335562722005,
-101.247309331379,-101.159047849102,-101.070756929917,-100.982365944315,
-100.893915356022,-100.805335431276,-100.782935014468,-100.694361865162,
-100.605903072113,-100.517534859742,-100.425978523867,-100.337711880311,
-100.249458489695,-100.161197007427,-100.072906088251,-99.9845151026583,
-99.8960645143748,-99.8074845896374,-99.7850841727403,-99.6965110234348,
-99.6080522303865,-99.5196840180148,-99.4281276821396,-99.3398610385841,
-99.251607647968,-99.1633461657009,-99.0750552465254,-98.9866642609333,
-98.8982136726508,-98.809633747914,-98.7872333310129,-98.6916230320358,
-98.5963332393344,-98.501241351583,-98.4064500985313,-98.340528648016),
 .UNSPECIFIED.);
#1456=B_SPLINE_CURVE_WITH_KNOTS('',3,(#46134,#46135,#46136,#46137,#46138,
#46139,#46140,#46141,#46142,#46143,#46144,#46145,#46146,#46147,#46148,#46149,
#46150,#46151,#46152,#46153,#46154,#46155,#46156,#46157,#46158,#46159,#46160,
#46161,#46162,#46163,#46164,#46165,#46166,#46167,#46168,#46169,#46170,#46171,
#46172,#46173,#46174,#46175,#46176,#46177,#46178,#46179,#46180,#46181,#46182,
#46183,#46184,#46185,#46186,#46187,#46188,#46189,#46190,#46191,#46192,#46193,
#46194,#46195,#46196,#46197,#46198,#46199,#46200,#46201,#46202,#46203,#46204,
#46205,#46206,#46207,#46208,#46209,#46210,#46211,#46212,#46213,#46214,#46215,
#46216,#46217,#46218,#46219,#46220,#46221,#46222,#46223,#46224,#46225,#46226,
#46227,#46228,#46229,#46230,#46231,#46232,#46233,#46234,#46235,#46236,#46237,
#46238,#46239,#46240,#46241,#46242,#46243,#46244,#46245,#46246,#46247,#46248,
#46249,#46250,#46251,#46252,#46253,#46254,#46255,#46256,#46257,#46258,#46259,
#46260,#46261,#46262,#46263,#46264,#46265,#46266,#46267,#46268,#46269,#46270,
#46271,#46272,#46273,#46274,#46275,#46276,#46277,#46278,#46279,#46280,#46281,
#46282,#46283,#46284,#46285,#46286,#46287,#46288,#46289,#46290,#46291,#46292,
#46293,#46294,#46295,#46296,#46297,#46298,#46299,#46300,#46301,#46302,#46303,
#46304,#46305,#46306,#46307,#46308,#46309,#46310,#46311,#46312,#46313,#46314,
#46315,#46316,#46317,#46318,#46319,#46320,#46321,#46322,#46323,#46324,#46325,
#46326,#46327,#46328,#46329,#46330,#46331,#46332,#46333,#46334,#46335,#46336,
#46337,#46338,#46339,#46340,#46341,#46342,#46343,#46344,#46345,#46346,#46347,
#46348,#46349,#46350,#46351,#46352,#46353,#46354,#46355,#46356,#46357,#46358,
#46359),.UNSPECIFIED.,.F.,.F.,(4,3,3,3,3,3,3,3,3,3,3,3,3,3,3,3,3,3,3,3,
3,3,3,3,3,3,3,3,3,3,3,3,3,3,3,3,3,3,3,3,3,3,3,3,3,3,3,3,3,3,3,3,3,3,3,3,
3,3,3,3,3,3,3,3,3,3,3,3,3,3,3,3,3,3,3,4),(-98.3405286478881,-98.2498497411809,
-98.1591056839463,-98.0666748852811,-97.9756879240618,-97.8825352066736,
-97.7893824892855,-97.7008093399791,-97.6123505469294,-97.5239823345569,
-97.432425998682,-97.3441593551254,-97.2559059645082,-97.1676444822402,
-97.0793535630634,-96.99096257747,-96.9025119891859,-96.8139320644476,-96.791531647558,
-96.7029584982515,-96.6144997052018,-96.526131492829,-96.4345751569543,
-96.3463085133976,-96.2580551227804,-96.1697936405121,-96.0815027213353,
-95.9931117357419,-95.9046611474578,-95.8160812227196,-95.7936808058307,
-95.705107656524,-95.6166488634743,-95.5282806511014,-95.4367243152267,
-95.3484576716697,-95.2602042810523,-95.1719427987839,-95.0836518796068,
-94.9952608940133,-94.9068103057289,-94.8182303809906,-94.7958299641032,
-94.7072568147966,-94.618798021747,-94.5304298093744,-94.4388734734996,
-94.3506068299428,-94.2623534393254,-94.1740919570567,-94.0858010378792,
-93.9974100522856,-93.9089594640012,-93.820379539263,-93.7979791223758,
-93.7094059730693,-93.6209471800196,-93.5325789676472,-93.4410226317723,
-93.3527559882155,-93.2645025975981,-93.1762411153299,-93.0879501961525,
-92.9995592105589,-92.911108622275,-92.8225286975367,-92.8001282806485,
-92.7125191503955,-92.6250518999664,-92.5376658860685,-92.4503387614408,
-92.3630482356725,-92.2757489183866,-92.1884454166725,-92.1010806652874,
-92.0573433407085),.UNSPECIFIED.);
#1457=B_SPLINE_CURVE_WITH_KNOTS('',3,(#46361,#46362,#46363,#46364,#46365,
#46366,#46367,#46368,#46369,#46370,#46371,#46372,#46373,#46374,#46375,#46376,
#46377,#46378,#46379,#46380,#46381,#46382,#46383,#46384,#46385,#46386,#46387,
#46388,#46389,#46390,#46391,#46392,#46393,#46394,#46395,#46396,#46397,#46398,
#46399,#46400,#46401,#46402,#46403,#46404,#46405,#46406,#46407,#46408,#46409,
#46410,#46411,#46412,#46413,#46414,#46415,#46416,#46417,#46418,#46419,#46420,
#46421,#46422,#46423,#46424,#46425,#46426,#46427,#46428,#46429,#46430,#46431,
#46432,#46433,#46434,#46435,#46436,#46437,#46438,#46439,#46440,#46441,#46442,
#46443,#46444,#46445,#46446,#46447,#46448,#46449,#46450,#46451,#46452,#46453,
#46454,#46455,#46456,#46457,#46458,#46459,#46460,#46461,#46462,#46463,#46464,
#46465,#46466,#46467,#46468,#46469,#46470,#46471,#46472,#46473,#46474,#46475,
#46476,#46477,#46478,#46479,#46480,#46481,#46482,#46483,#46484,#46485,#46486,
#46487,#46488,#46489,#46490,#46491,#46492,#46493,#46494,#46495,#46496,#46497,
#46498,#46499,#46500,#46501,#46502,#46503,#46504,#46505,#46506,#46507,#46508,
#46509,#46510,#46511,#46512,#46513,#46514,#46515,#46516,#46517,#46518,#46519,
#46520,#46521,#46522,#46523,#46524,#46525,#46526,#46527,#46528,#46529,#46530,
#46531,#46532,#46533,#46534,#46535,#46536,#46537,#46538,#46539,#46540,#46541,
#46542,#46543,#46544,#46545,#46546,#46547,#46548,#46549,#46550,#46551,#46552,
#46553,#46554,#46555,#46556,#46557,#46558,#46559,#46560,#46561,#46562,#46563,
#46564,#46565,#46566,#46567,#46568,#46569,#46570,#46571,#46572,#46573,#46574,
#46575,#46576,#46577,#46578,#46579,#46580,#46581,#46582,#46583,#46584,#46585,
#46586,#46587,#46588,#46589),.UNSPECIFIED.,.F.,.F.,(4,3,3,3,3,3,3,3,3,3,
3,3,3,3,3,3,3,3,3,3,3,3,3,3,3,3,3,3,3,3,3,3,3,3,3,3,3,3,3,3,3,3,3,3,3,3,
3,3,3,3,3,3,3,3,3,3,3,3,3,3,3,3,3,3,3,3,3,3,3,3,3,3,3,3,3,3,4),(-92.057343340495,
-91.9449587259192,-91.8301949929713,-91.8022774389211,-91.7137042896145,
-91.6252454965649,-91.5368772841923,-91.4453209483174,-91.3570543047606,
-91.2688009141433,-91.180539431875,-91.0922485126981,-91.0038575271046,
-90.9154069388204,-90.8268270140822,-90.8044265971936,-90.7158534478869,
-90.627394654837,-90.5390264424644,-90.4474701065896,-90.3592034630327,
-90.2709500724152,-90.1826885901467,-90.0943976709694,-90.0060066853758,
-89.9175560970915,-89.8289761723532,-89.8065757554662,-89.7180026061597,
-89.6295438131101,-89.5411756007375,-89.4496192648627,-89.361352621306,
-89.2730992306887,-89.1848377484205,-89.0965468292434,-89.00815584365,-88.9197052553658,
-88.8311253306277,-88.8087249137388,-88.7201517644322,-88.6316929713824,
-88.5433247590098,-88.451768423135,-88.3635017795781,-88.2752483889608,
-88.1869869066924,-88.0986959875153,-88.0103050019217,-87.9218544136375,
-87.8332744888993,-87.8108740720114,-87.7223009227048,-87.633842129655,
-87.5454739172825,-87.4539175814076,-87.3656509378508,-87.2773975472334,
-87.1891360649651,-87.1008451457881,-87.0124541601946,-86.9240035719103,
-86.8354236471721,-86.813023230284,-86.7244500809775,-86.6359912879278,
-86.5476230755552,-86.4560667396804,-86.3678000961236,-86.2795467055064,
-86.1912852232381,-86.102994304061,-86.0146033184676,-85.9261527301834,
-85.8375728054453,-85.8151723885566,-85.7741580335289),.UNSPECIFIED.);
#1458=B_SPLINE_CURVE_WITH_KNOTS('',3,(#46591,#46592,#46593,#46594,#46595,
#46596,#46597,#46598,#46599,#46600,#46601,#46602,#46603,#46604,#46605,#46606,
#46607,#46608,#46609,#46610,#46611,#46612,#46613,#46614,#46615,#46616,#46617,
#46618,#46619,#46620,#46621,#46622,#46623,#46624,#46625,#46626,#46627,#46628,
#46629,#46630,#46631,#46632,#46633,#46634,#46635,#46636,#46637,#46638,#46639,
#46640,#46641,#46642,#46643,#46644,#46645,#46646,#46647,#46648,#46649,#46650,
#46651,#46652,#46653,#46654,#46655,#46656,#46657,#46658,#46659,#46660,#46661,
#46662,#46663,#46664,#46665,#46666,#46667,#46668,#46669,#46670,#46671,#46672,
#46673,#46674,#46675,#46676,#46677,#46678,#46679,#46680,#46681,#46682,#46683,
#46684,#46685,#46686,#46687,#46688,#46689,#46690,#46691,#46692,#46693,#46694,
#46695,#46696,#46697,#46698,#46699,#46700,#46701,#46702,#46703,#46704,#46705,
#46706,#46707,#46708,#46709,#46710,#46711,#46712,#46713,#46714,#46715,#46716,
#46717,#46718,#46719,#46720,#46721,#46722,#46723,#46724,#46725,#46726,#46727,
#46728,#46729,#46730,#46731,#46732,#46733,#46734,#46735,#46736,#46737,#46738,
#46739,#46740,#46741,#46742,#46743,#46744,#46745,#46746,#46747,#46748,#46749,
#46750,#46751,#46752,#46753,#46754,#46755,#46756,#46757,#46758,#46759,#46760,
#46761,#46762,#46763,#46764,#46765,#46766,#46767,#46768,#46769,#46770,#46771,
#46772,#46773,#46774,#46775,#46776,#46777,#46778,#46779,#46780,#46781,#46782,
#46783,#46784,#46785,#46786,#46787,#46788,#46789,#46790,#46791,#46792,#46793,
#46794,#46795,#46796,#46797,#46798,#46799,#46800,#46801,#46802,#46803,#46804,
#46805,#46806,#46807,#46808,#46809,#46810,#46811,#46812,#46813,#46814,#46815,
#46816),.UNSPECIFIED.,.F.,.F.,(4,3,3,3,3,3,3,3,3,3,3,3,3,3,3,3,3,3,3,3,
3,3,3,3,3,3,3,3,3,3,3,3,3,3,3,3,3,3,3,3,3,3,3,3,3,3,3,3,3,3,3,3,3,3,3,3,
3,3,3,3,3,3,3,3,3,3,3,3,3,3,3,3,3,3,3,4),(-85.7741580333869,-85.6861685578636,
-85.5982909458262,-85.5105007898011,-85.4227708640778,-85.3350723553463,
-85.247383339102,-85.1596819028892,-85.0718905841978,-84.9840538824836,
-84.8960730339901,-84.8173215468292,-84.7287483975225,-84.6402896044727,
-84.5519213921003,-84.4603650562255,-84.3720984126686,-84.2838450220513,
-84.1955835397829,-84.1072926206058,-84.0189016350122,-83.930451046728,
-83.8418711219897,-83.8194707051018,-83.7308975557953,-83.6424387627455,
-83.5540705503729,-83.4625142144981,-83.3742475709413,-83.285994180324,
-83.1977326980555,-83.1094417788783,-83.0210507932848,-82.9326002050006,
-82.8440202802623,-82.8216198633744,-82.7330467140678,-82.644587921018,
-82.556219708645,-82.4646633727702,-82.3763967292134,-82.288143338596,-82.1998818563276,
-82.1115909371499,-82.0231999515564,-81.9347493632724,-81.846169438534,
-81.823769021647,-81.7351958723405,-81.6467370792908,-81.5583688669186,
-81.4668125310437,-81.3785458874869,-81.2902924968697,-81.2020310146015,
-81.1137400954241,-81.0253491098307,-80.9368985215465,-80.8483185968085,
-80.8259181799196,-80.7373450306132,-80.6488862375634,-80.5605180251908,
-80.468961689316,-80.3806950457592,-80.2924416551418,-80.2041801728737,
-80.115889253696,-80.0274982681023,-79.9390476798177,-79.8504677550797,
-79.8280673381922,-79.7244964726417,-79.6214093916813,-79.5191863692498,
-79.4909727265609),.UNSPECIFIED.);
#1459=B_SPLINE_CURVE_WITH_KNOTS('',3,(#46818,#46819,#46820,#46821,#46822,
#46823,#46824,#46825,#46826,#46827,#46828,#46829,#46830,#46831,#46832,#46833,
#46834,#46835,#46836,#46837,#46838,#46839,#46840,#46841,#46842,#46843,#46844,
#46845,#46846,#46847,#46848,#46849,#46850,#46851,#46852,#46853,#46854,#46855,
#46856,#46857,#46858,#46859,#46860,#46861,#46862,#46863,#46864,#46865,#46866,
#46867,#46868,#46869,#46870,#46871,#46872,#46873,#46874,#46875,#46876,#46877,
#46878,#46879,#46880,#46881,#46882,#46883,#46884,#46885,#46886,#46887,#46888,
#46889,#46890,#46891,#46892,#46893,#46894,#46895,#46896,#46897,#46898,#46899,
#46900,#46901,#46902,#46903,#46904,#46905,#46906,#46907,#46908,#46909,#46910,
#46911,#46912,#46913,#46914,#46915,#46916,#46917,#46918,#46919,#46920,#46921,
#46922,#46923,#46924,#46925,#46926,#46927,#46928,#46929,#46930,#46931,#46932,
#46933,#46934,#46935,#46936,#46937,#46938,#46939,#46940,#46941,#46942,#46943,
#46944,#46945,#46946,#46947,#46948,#46949,#46950,#46951,#46952,#46953,#46954,
#46955,#46956,#46957,#46958,#46959,#46960,#46961,#46962,#46963,#46964,#46965,
#46966,#46967,#46968,#46969,#46970,#46971,#46972,#46973,#46974,#46975,#46976,
#46977,#46978,#46979,#46980,#46981,#46982,#46983,#46984,#46985,#46986,#46987,
#46988,#46989,#46990,#46991,#46992,#46993,#46994,#46995,#46996,#46997,#46998,
#46999,#47000,#47001,#47002,#47003,#47004,#47005,#47006,#47007,#47008,#47009,
#47010,#47011,#47012,#47013,#47014,#47015,#47016,#47017,#47018,#47019,#47020,
#47021,#47022,#47023,#47024,#47025,#47026,#47027,#47028,#47029,#47030,#47031,
#47032,#47033,#47034,#47035,#47036,#47037,#47038,#47039,#47040,#47041,#47042,
#47043),.UNSPECIFIED.,.F.,.F.,(4,3,3,3,3,3,3,3,3,3,3,3,3,3,3,3,3,3,3,3,
3,3,3,3,3,3,3,3,3,3,3,3,3,3,3,3,3,3,3,3,3,3,3,3,3,3,3,3,3,3,3,3,3,3,3,3,
3,3,3,3,3,3,3,3,3,3,3,3,3,3,3,3,3,3,3,4),(-79.4909727263493,-79.4027030535825,
-79.3144454917003,-79.2261787933954,-79.1378817098842,-79.0494784849834,
-78.9610151902706,-78.8724102190024,-78.8302164964648,-78.7416433471584,
-78.6531845541089,-78.5648163417366,-78.4732600058617,-78.3849933623051,
-78.296739971688,-78.2084784894198,-78.1201875702428,-78.0317965846497,
-77.9433459963656,-77.8547660716276,-77.8323656547374,-77.7437925054306,
-77.6553337123805,-77.5669655000076,-77.4754091641329,-77.3871425205758,
-77.2988891299583,-77.2106276476894,-77.1223367285122,-77.0339457429185,
-76.945495154634,-76.8569152298955,-76.83451481301,-76.7459416637034,-76.6574828706539,
-76.5691146582814,-76.4775583224066,-76.3892916788497,-76.3010382882324,
-76.2127768059642,-76.1244858867866,-76.0360949011931,-75.9476443129089,
-75.8590643881708,-75.8366639712826,-75.7480908219762,-75.6596320289267,
-75.571263816554,-75.4797074806792,-75.3914408371224,-75.3031874465053,
-75.2149259642374,-75.1266350450602,-75.0382440594668,-74.9497934711824,
-74.8612135464444,-74.8388131295552,-74.7502399802486,-74.6617811871987,
-74.573412974826,-74.4818566389512,-74.3935899953943,-74.3053366047771,
-74.2170751225086,-74.1287842033319,-74.0403932177383,-73.9519426294544,
-73.8633627047159,-73.8409622878278,-73.751861812671,-73.6628783053689,
-73.573990958071,-73.4824400733457,-73.3936855521488,-73.3007364856592,
-73.2077874191697),.UNSPECIFIED.);
#1460=B_SPLINE_CURVE_WITH_KNOTS('',3,(#47045,#47046,#47047,#47048,#47049,
#47050,#47051,#47052,#47053,#47054,#47055,#47056,#47057,#47058,#47059,#47060,
#47061,#47062,#47063,#47064,#47065,#47066,#47067,#47068,#47069,#47070,#47071,
#47072,#47073,#47074,#47075,#47076,#47077,#47078,#47079,#47080,#47081,#47082,
#47083,#47084,#47085,#47086,#47087,#47088,#47089,#47090,#47091,#47092,#47093,
#47094,#47095,#47096,#47097,#47098,#47099,#47100,#47101,#47102,#47103,#47104,
#47105,#47106,#47107,#47108,#47109,#47110,#47111,#47112,#47113,#47114,#47115,
#47116,#47117,#47118,#47119,#47120,#47121,#47122,#47123,#47124,#47125,#47126,
#47127,#47128,#47129,#47130,#47131,#47132,#47133,#47134,#47135,#47136,#47137,
#47138,#47139,#47140,#47141,#47142,#47143,#47144,#47145,#47146,#47147,#47148,
#47149,#47150,#47151,#47152,#47153,#47154,#47155,#47156,#47157,#47158,#47159,
#47160,#47161,#47162,#47163,#47164,#47165,#47166,#47167,#47168,#47169,#47170,
#47171,#47172,#47173,#47174,#47175,#47176,#47177,#47178,#47179,#47180,#47181,
#47182,#47183,#47184,#47185,#47186,#47187,#47188,#47189,#47190,#47191,#47192,
#47193,#47194,#47195,#47196,#47197,#47198,#47199,#47200,#47201,#47202,#47203,
#47204,#47205,#47206,#47207,#47208,#47209,#47210,#47211,#47212,#47213,#47214,
#47215,#47216,#47217,#47218,#47219,#47220,#47221,#47222,#47223,#47224,#47225,
#47226,#47227,#47228,#47229,#47230,#47231,#47232,#47233,#47234,#47235,#47236,
#47237,#47238,#47239,#47240,#47241,#47242,#47243,#47244,#47245,#47246,#47247,
#47248,#47249,#47250,#47251,#47252,#47253,#47254,#47255,#47256,#47257,#47258,
#47259,#47260,#47261,#47262,#47263,#47264,#47265,#47266,#47267,#47268,#47269,
#47270),.UNSPECIFIED.,.F.,.F.,(4,3,3,3,3,3,3,3,3,3,3,3,3,3,3,3,3,3,3,3,
3,3,3,3,3,3,3,3,3,3,3,3,3,3,3,3,3,3,3,3,3,3,3,3,3,3,3,3,3,3,3,3,3,3,3,3,
3,3,3,3,3,3,3,3,3,3,3,3,3,3,3,3,3,3,3,4),(-73.2077874189448,-73.107736006707,
-73.0072421038471,-72.9061731673785,-72.8431114461004,-72.7545382967941,
-72.6660795037445,-72.5777112913722,-72.4861549554973,-72.3978883119406,
-72.3096349213235,-72.2213734390554,-72.1330825198784,-72.0446915342851,
-71.9562409460012,-71.8676610212632,-71.845260604373,-71.7566874550661,
-71.668228662016,-71.5798604496431,-71.4883041137684,-71.4000374702112,
-71.3117840795936,-71.2235225973249,-71.1352316781473,-71.0468406925535,
-70.9583901042689,-70.8698101795304,-70.8474097626456,-70.7588366133391,
-70.6703778202896,-70.5820096079171,-70.4904532720422,-70.4021866284856,
-70.3139332378684,-70.2256717556002,-70.1373808364232,-70.0489898508298,
-69.9605392625457,-69.8719593378077,-69.8495589209182,-69.7609857716116,
-69.6725269785619,-69.5841587661894,-69.4926024303146,-69.4043357867578,
-69.3160823961405,-69.2278209138722,-69.1395299946951,-69.0511390091016,
-68.9626884208175,-68.8741084960793,-68.8517080791908,-68.7631349298841,
-68.6746761368343,-68.5863079244616,-68.4947515885868,-68.4064849450298,
-68.3182315544124,-68.229970072144,-68.1416791529668,-68.0532881673732,
-67.9648375790888,-67.8762576543504,-67.8538572374634,-67.766148257947,
-67.6785529256838,-67.5910465431623,-67.5036029660178,-67.4161918075192,
-67.3287908976867,-67.2413780793301,-67.153881432156,-67.0663392072975,
-66.978667484412,-66.9246021121963),.UNSPECIFIED.);
#1461=B_SPLINE_CURVE_WITH_KNOTS('',3,(#47272,#47273,#47274,#47275,#47276,
#47277,#47278,#47279,#47280,#47281,#47282,#47283,#47284,#47285,#47286,#47287,
#47288,#47289,#47290,#47291,#47292,#47293,#47294,#47295,#47296,#47297,#47298,
#47299,#47300,#47301,#47302,#47303,#47304,#47305,#47306,#47307,#47308,#47309,
#47310,#47311,#47312,#47313,#47314,#47315,#47316,#47317,#47318,#47319,#47320,
#47321,#47322,#47323,#47324,#47325,#47326,#47327,#47328,#47329,#47330,#47331,
#47332,#47333,#47334,#47335,#47336,#47337,#47338,#47339,#47340,#47341,#47342,
#47343,#47344,#47345,#47346,#47347,#47348,#47349,#47350,#47351,#47352,#47353,
#47354,#47355,#47356,#47357,#47358,#47359,#47360,#47361,#47362,#47363,#47364,
#47365,#47366,#47367,#47368,#47369,#47370,#47371,#47372,#47373,#47374,#47375,
#47376,#47377,#47378,#47379,#47380,#47381,#47382,#47383,#47384,#47385,#47386,
#47387,#47388,#47389,#47390,#47391,#47392,#47393,#47394,#47395,#47396,#47397,
#47398,#47399,#47400,#47401,#47402,#47403,#47404,#47405,#47406,#47407,#47408,
#47409,#47410,#47411,#47412,#47413,#47414,#47415,#47416,#47417,#47418,#47419,
#47420,#47421,#47422,#47423,#47424,#47425,#47426,#47427,#47428,#47429,#47430,
#47431,#47432,#47433,#47434,#47435,#47436,#47437,#47438,#47439,#47440,#47441,
#47442,#47443,#47444,#47445,#47446,#47447,#47448,#47449,#47450,#47451,#47452,
#47453,#47454,#47455,#47456,#47457,#47458,#47459,#47460,#47461,#47462,#47463,
#47464,#47465,#47466,#47467,#47468,#47469,#47470,#47471,#47472,#47473,#47474,
#47475,#47476,#47477,#47478,#47479,#47480,#47481,#47482,#47483,#47484,#47485,
#47486,#47487,#47488,#47489,#47490,#47491,#47492,#47493,#47494,#47495,#47496,
#47497),.UNSPECIFIED.,.F.,.F.,(4,3,3,3,3,3,3,3,3,3,3,3,3,3,3,3,3,3,3,3,
3,3,3,3,3,3,3,3,3,3,3,3,3,3,3,3,3,3,3,3,3,3,3,3,3,3,3,3,3,3,3,3,3,3,3,3,
3,3,3,3,3,3,3,3,3,3,3,3,3,3,3,3,3,3,3,4),(-66.9246021119902,-66.856006395736,
-66.7674332464294,-66.6789744533797,-66.5906062410072,-66.4990499051323,
-66.4107832615755,-66.3225298709582,-66.2342683886898,-66.1459774695125,
-66.057586483919,-65.9691358956348,-65.8805559708966,-65.8581555540086,
-65.769582404702,-65.6811236116524,-65.5927553992799,-65.5011990634051,
-65.4129324198483,-65.324679029231,-65.2364175469627,-65.1481266277855,
-65.0597356421921,-64.9712850539079,-64.8827051291697,-64.8603047122812,
-64.7717315629746,-64.6832727699248,-64.5949045575522,-64.5033482216774,
-64.4150815781205,-64.3268281875032,-64.2385667052348,-64.1502757860576,
-64.0618848004641,-63.9734342121798,-63.8848542874416,-63.8624538705538,
-63.7738807212472,-63.6854219281975,-63.5970537158249,-63.5054973799501,
-63.4172307363932,-63.3289773457759,-63.2407158635076,-63.1524249443304,
-63.0640339587369,-62.9755833704527,-62.8870034457144,-62.8646030288264,
-62.7760298795198,-62.68757108647,-62.5992028740974,-62.5076465382226,-62.4193798946658,
-62.3311265040484,-62.2428650217801,-62.1545741026029,-62.0661831170094,
-61.9777325287252,-61.889152603987,-61.866752187099,-61.7781790377924,-61.6897202447427,
-61.6013520323702,-61.5097956964953,-61.4215290529385,-61.3332756623212,
-61.245014180053,-61.156723260876,-61.0683322752826,-60.9798816869985,-60.8913017622603,
-60.8689013453716,-60.7496264044044,-60.6414168048105),.UNSPECIFIED.);
#1462=B_SPLINE_CURVE_WITH_KNOTS('',3,(#47499,#47500,#47501,#47502,#47503,
#47504,#47505,#47506,#47507,#47508,#47509,#47510,#47511,#47512,#47513,#47514,
#47515,#47516,#47517,#47518,#47519,#47520,#47521,#47522,#47523,#47524,#47525,
#47526,#47527,#47528,#47529,#47530,#47531,#47532,#47533,#47534,#47535,#47536,
#47537,#47538,#47539,#47540,#47541,#47542,#47543,#47544,#47545,#47546,#47547,
#47548,#47549,#47550,#47551,#47552,#47553,#47554,#47555,#47556,#47557,#47558,
#47559,#47560,#47561,#47562,#47563,#47564,#47565,#47566,#47567,#47568,#47569,
#47570,#47571,#47572,#47573,#47574,#47575,#47576,#47577,#47578,#47579,#47580,
#47581,#47582,#47583,#47584,#47585,#47586,#47587,#47588,#47589,#47590,#47591,
#47592,#47593,#47594,#47595,#47596,#47597,#47598,#47599,#47600,#47601,#47602,
#47603,#47604,#47605,#47606,#47607,#47608,#47609,#47610,#47611,#47612,#47613,
#47614,#47615,#47616,#47617,#47618,#47619,#47620,#47621,#47622,#47623,#47624,
#47625,#47626,#47627,#47628,#47629,#47630,#47631,#47632,#47633,#47634,#47635,
#47636,#47637,#47638,#47639,#47640,#47641,#47642,#47643,#47644,#47645,#47646,
#47647,#47648,#47649,#47650,#47651,#47652,#47653,#47654,#47655,#47656,#47657,
#47658,#47659,#47660,#47661,#47662,#47663,#47664,#47665,#47666,#47667,#47668,
#47669,#47670,#47671,#47672,#47673,#47674,#47675,#47676,#47677,#47678,#47679,
#47680,#47681,#47682,#47683,#47684,#47685,#47686,#47687,#47688,#47689,#47690,
#47691,#47692,#47693,#47694,#47695,#47696,#47697,#47698,#47699,#47700,#47701,
#47702,#47703,#47704,#47705,#47706,#47707,#47708,#47709,#47710,#47711,#47712,
#47713,#47714,#47715,#47716,#47717,#47718,#47719,#47720,#47721,#47722,#47723,
#47724),.UNSPECIFIED.,.F.,.F.,(4,3,3,3,3,3,3,3,3,3,3,3,3,3,3,3,3,3,3,3,
3,3,3,3,3,3,3,3,3,3,3,3,3,3,3,3,3,3,3,3,3,3,3,3,3,3,3,3,3,3,3,3,3,3,3,3,
3,3,3,3,3,3,3,3,3,3,3,3,3,3,3,3,3,3,3,4),(-60.6414168046243,-60.5541977116721,
-60.4670437573164,-60.3799239858169,-60.2928160029574,-60.2056974285119,
-60.1184916827307,-60.0312413215284,-59.9438501868131,-59.8710505036442,
-59.7824773543376,-59.6940185612878,-59.6056503489152,-59.5140940130404,
-59.4258273694834,-59.3375739788659,-59.2493124965977,-59.1610215774201,
-59.0726305918265,-58.9841800035421,-58.8956000788037,-58.8731996619168,
-58.7846265126102,-58.6961677195606,-58.6077995071879,-58.5162431713131,
-58.4279765277562,-58.3397231371388,-58.2514616548706,-58.1631707356933,
-58.0747797500998,-57.9863291618153,-57.8977492370771,-57.8753488201894,
-57.7867756708828,-57.6983168778331,-57.6099486654601,-57.5183923295854,
-57.4301256860287,-57.3418722954114,-57.253610813143,-57.165319893966,-57.0769289083726,
-56.9884783200883,-56.89989839535,-56.877497978462,-56.7889248291553,-56.7004660361056,
-56.6120978237326,-56.5205414878579,-56.432274844301,-56.3440214536834,
-56.2557599714151,-56.167469052238,-56.0790780666444,-55.9906274783599,
-55.9020475536216,-55.8796471367345,-55.7910739874279,-55.7026151943781,
-55.6142469820053,-55.5226906461305,-55.4344240025736,-55.3461706119562,
-55.2579091296879,-55.1696182105113,-55.0812272249179,-54.9927766366333,
-54.904196711895,-54.8817962950071,-54.7896385149843,-54.697634462087,-54.6058196949304,
-54.5141167775388,-54.4225461234993,-54.358231497631),.UNSPECIFIED.);
#1463=B_SPLINE_CURVE_WITH_KNOTS('',3,(#47726,#47727,#47728,#47729,#47730,
#47731,#47732,#47733,#47734,#47735,#47736,#47737,#47738,#47739,#47740,#47741,
#47742,#47743,#47744,#47745,#47746,#47747,#47748,#47749,#47750,#47751,#47752,
#47753,#47754,#47755,#47756,#47757,#47758,#47759,#47760,#47761,#47762,#47763,
#47764,#47765,#47766,#47767,#47768,#47769,#47770,#47771,#47772,#47773,#47774,
#47775,#47776,#47777,#47778,#47779,#47780,#47781,#47782,#47783,#47784,#47785,
#47786,#47787,#47788,#47789,#47790,#47791,#47792,#47793,#47794,#47795,#47796,
#47797,#47798,#47799,#47800,#47801,#47802,#47803,#47804,#47805,#47806,#47807,
#47808,#47809,#47810,#47811,#47812,#47813,#47814,#47815,#47816,#47817,#47818,
#47819,#47820,#47821,#47822,#47823,#47824,#47825,#47826,#47827,#47828,#47829,
#47830,#47831,#47832,#47833,#47834,#47835,#47836,#47837,#47838,#47839,#47840,
#47841,#47842,#47843,#47844,#47845,#47846,#47847,#47848,#47849,#47850,#47851,
#47852,#47853,#47854,#47855,#47856,#47857,#47858,#47859,#47860,#47861,#47862,
#47863,#47864,#47865,#47866,#47867,#47868,#47869,#47870,#47871,#47872,#47873,
#47874,#47875,#47876,#47877,#47878,#47879,#47880,#47881,#47882,#47883,#47884,
#47885,#47886,#47887,#47888,#47889,#47890,#47891,#47892,#47893,#47894,#47895,
#47896,#47897,#47898,#47899,#47900,#47901,#47902,#47903,#47904,#47905,#47906,
#47907,#47908,#47909,#47910,#47911,#47912,#47913,#47914,#47915,#47916,#47917,
#47918,#47919,#47920,#47921,#47922,#47923,#47924,#47925,#47926,#47927,#47928,
#47929,#47930,#47931,#47932,#47933,#47934,#47935,#47936,#47937,#47938,#47939,
#47940,#47941,#47942,#47943,#47944,#47945,#47946,#47947,#47948,#47949,#47950,
#47951),.UNSPECIFIED.,.F.,.F.,(4,3,3,3,3,3,3,3,3,3,3,3,3,3,3,3,3,3,3,3,
3,3,3,3,3,3,3,3,3,3,3,3,3,3,3,3,3,3,3,3,3,3,3,3,3,3,3,3,3,3,3,3,3,3,3,3,
3,3,3,3,3,3,3,3,3,3,3,3,3,3,3,3,3,3,3,4),(-54.3582314975039,-54.264791755642,
-54.1695801800514,-54.0757075390254,-53.9798264961525,-53.8839454532797,
-53.795372303973,-53.7069135109231,-53.6185452985502,-53.5269889626755,
-53.4387223191185,-53.3504689285011,-53.2622074462326,-53.1739165270553,
-53.0855255414617,-52.9970749531774,-52.9084950284391,-52.8860946115523,
-52.7975214622459,-52.7090626691963,-52.6206944568239,-52.529138120949,
-52.4408714773923,-52.3526180867751,-52.264356604507,-52.1760656853299,
-52.0876746997365,-51.9992241114524,-51.9106441867144,-51.8882437698249,
-51.7996706205183,-51.7112118274685,-51.6228436150958,-51.531287279221,
-51.4430206356642,-51.3547672450468,-51.2665057627784,-51.1782148436012,
-51.0898238580077,-51.0013732697234,-50.9127933449851,-50.8903929280975,
-50.8018197787909,-50.7133609857411,-50.6249927733685,-50.5334364374937,
-50.4451697939368,-50.3569164033195,-50.2686549210512,-50.1803640018741,
-50.0919730162806,-50.0035224279963,-49.9149425032581,-49.8925420863701,
-49.8039689370635,-49.7155101440137,-49.6271419316411,-49.5355855957663,
-49.4473189522095,-49.3590655615921,-49.2708040793238,-49.1825131601465,
-49.094122174553,-49.0056715862686,-48.9170916615304,-48.8946912446427,
-48.8074317150175,-48.7158835244647,-48.628840891428,-48.5418520352336,
-48.4548944238696,-48.3679455587889,-48.280947766268,-48.1939214043626,
-48.1068026622925,-48.0750461905954),.UNSPECIFIED.);
#1464=B_SPLINE_CURVE_WITH_KNOTS('',3,(#47953,#47954,#47955,#47956,#47957,
#47958,#47959,#47960,#47961,#47962,#47963,#47964,#47965,#47966,#47967,#47968,
#47969,#47970,#47971,#47972,#47973,#47974,#47975,#47976,#47977,#47978,#47979,
#47980,#47981,#47982,#47983,#47984,#47985,#47986,#47987,#47988,#47989,#47990,
#47991,#47992,#47993,#47994,#47995,#47996,#47997,#47998,#47999,#48000,#48001,
#48002,#48003,#48004,#48005,#48006,#48007,#48008,#48009,#48010,#48011,#48012,
#48013,#48014,#48015,#48016,#48017,#48018,#48019,#48020,#48021,#48022,#48023,
#48024,#48025,#48026,#48027,#48028,#48029,#48030,#48031,#48032,#48033,#48034,
#48035,#48036,#48037,#48038,#48039,#48040,#48041,#48042,#48043,#48044,#48045,
#48046,#48047,#48048,#48049,#48050,#48051,#48052,#48053,#48054,#48055,#48056,
#48057,#48058,#48059,#48060,#48061,#48062,#48063,#48064,#48065,#48066,#48067,
#48068,#48069,#48070,#48071,#48072,#48073,#48074,#48075,#48076,#48077,#48078,
#48079,#48080,#48081,#48082,#48083,#48084,#48085,#48086,#48087,#48088,#48089,
#48090,#48091,#48092,#48093,#48094,#48095,#48096,#48097,#48098,#48099,#48100,
#48101,#48102,#48103,#48104,#48105,#48106,#48107,#48108,#48109,#48110,#48111,
#48112,#48113,#48114,#48115,#48116,#48117,#48118,#48119,#48120,#48121,#48122,
#48123,#48124,#48125,#48126,#48127,#48128,#48129,#48130,#48131,#48132,#48133,
#48134,#48135,#48136,#48137,#48138,#48139,#48140,#48141,#48142,#48143,#48144,
#48145,#48146,#48147,#48148,#48149,#48150,#48151,#48152,#48153,#48154,#48155,
#48156,#48157,#48158,#48159,#48160,#48161,#48162,#48163,#48164,#48165,#48166,
#48167,#48168,#48169,#48170,#48171,#48172,#48173,#48174,#48175,#48176,#48177,
#48178),.UNSPECIFIED.,.F.,.F.,(4,3,3,3,3,3,3,3,3,3,3,3,3,3,3,3,3,3,3,3,
3,3,3,3,3,3,3,3,3,3,3,3,3,3,3,3,3,3,3,3,3,3,3,3,3,3,3,3,3,3,3,3,3,3,3,3,
3,3,3,3,3,3,3,3,3,3,3,3,3,3,3,3,3,3,3,4),(-48.0750461904514,-47.9402553841227,
-47.8968404029153,-47.8082672536088,-47.7198084605591,-47.6314402481864,
-47.5398839123116,-47.4516172687548,-47.3633638781374,-47.2751023958691,
-47.1868114766918,-47.0984204910982,-47.0099699028139,-46.9213899780757,
-46.8989895611879,-46.8104164118817,-46.7219576188323,-46.63358940646,-46.5420330705851,
-46.4537664270286,-46.3655130364117,-46.2772515541438,-46.188960634967,
-46.1005696493739,-46.01211906109,-45.9235391363522,-45.9011387194605,-45.8125655701538,
-45.7241067771039,-45.6357385647311,-45.5441822288564,-45.4559155852994,
-45.3676621946819,-45.2794007124134,-45.191109793236,-45.1027188076424,
-45.014268219358,-44.9256882946196,-44.9032878777331,-44.8147147284265,
-44.7262559353768,-44.6378877230042,-44.5463313871294,-44.4580647435726,
-44.3698113529553,-44.281549870687,-44.1932589515098,-44.1048679659163,
-44.0164173776321,-43.9278374528939,-43.9054370360057,-43.8168638866991,
-43.7284050936493,-43.6400368812767,-43.5484805454019,-43.460213901845,
-43.3719605112277,-43.2836990289593,-43.1954081097822,-43.1070171241887,
-43.0185665359043,-42.9299866111661,-42.9075861942783,-42.8190130449717,
-42.7305542519221,-42.6421860395496,-42.5506297036748,-42.462363060118,
-42.3741096695007,-42.2858481872324,-42.1975572680554,-42.109166282462,
-42.0207156941779,-41.9321357694396,-41.9097353525509,-41.7918608832718),
 .UNSPECIFIED.);
#1465=B_SPLINE_CURVE_WITH_KNOTS('',3,(#48180,#48181,#48182,#48183,#48184,
#48185,#48186,#48187,#48188,#48189,#48190,#48191,#48192,#48193,#48194,#48195,
#48196,#48197,#48198,#48199,#48200,#48201,#48202,#48203,#48204,#48205,#48206,
#48207,#48208,#48209,#48210,#48211,#48212,#48213,#48214,#48215,#48216,#48217,
#48218,#48219,#48220,#48221,#48222,#48223,#48224,#48225,#48226,#48227,#48228,
#48229,#48230,#48231,#48232,#48233,#48234,#48235,#48236,#48237,#48238,#48239,
#48240,#48241,#48242,#48243,#48244,#48245,#48246,#48247,#48248,#48249,#48250,
#48251,#48252,#48253,#48254,#48255,#48256,#48257,#48258,#48259,#48260,#48261,
#48262,#48263,#48264,#48265,#48266,#48267,#48268,#48269,#48270,#48271,#48272,
#48273,#48274,#48275,#48276,#48277,#48278,#48279,#48280,#48281,#48282,#48283,
#48284,#48285,#48286,#48287,#48288,#48289,#48290,#48291,#48292,#48293,#48294,
#48295,#48296,#48297,#48298,#48299,#48300,#48301,#48302,#48303,#48304,#48305,
#48306,#48307,#48308,#48309,#48310,#48311,#48312,#48313,#48314,#48315,#48316,
#48317,#48318,#48319,#48320,#48321,#48322,#48323,#48324,#48325,#48326,#48327,
#48328,#48329,#48330,#48331,#48332,#48333,#48334,#48335,#48336,#48337,#48338,
#48339,#48340,#48341,#48342,#48343,#48344,#48345,#48346,#48347,#48348,#48349,
#48350,#48351,#48352,#48353,#48354,#48355,#48356,#48357,#48358,#48359,#48360,
#48361,#48362,#48363,#48364,#48365,#48366,#48367,#48368,#48369,#48370,#48371,
#48372,#48373,#48374,#48375,#48376,#48377,#48378,#48379,#48380,#48381,#48382,
#48383,#48384,#48385,#48386,#48387,#48388,#48389,#48390,#48391,#48392,#48393,
#48394,#48395,#48396,#48397,#48398,#48399,#48400,#48401,#48402,#48403,#48404,
#48405),.UNSPECIFIED.,.F.,.F.,(4,3,3,3,3,3,3,3,3,3,3,3,3,3,3,3,3,3,3,3,
3,3,3,3,3,3,3,3,3,3,3,3,3,3,3,3,3,3,3,3,3,3,3,3,3,3,3,3,3,3,3,3,3,3,3,3,
3,3,3,3,3,3,3,3,3,3,3,3,3,3,3,3,3,3,3,4),(-41.7918608830424,-41.7045602140835,
-41.6173582378056,-41.5291740219328,-41.4420878042718,-41.3550194179906,
-41.2679464495758,-41.1789309648877,-41.0917343408291,-41.0018094258263,
-40.9118845108235,-40.8233113615169,-40.734852568467,-40.6464843560945,
-40.5549280202197,-40.4666613766628,-40.3784079860455,-40.2901465037771,
-40.2018555846003,-40.1134645990068,-40.0250140107226,-39.9364340859844,
-39.9140336690961,-39.8254605197895,-39.7370017267396,-39.648633514367,
-39.5570771784922,-39.4688105349354,-39.380557144318,-39.2922956620497,
-39.2040047428726,-39.1156137572792,-39.0271631689949,-38.9385832442568,
-38.9161828273687,-38.827609678062,-38.7391508850121,-38.6507826726396,
-38.5592263367648,-38.4709596932079,-38.3827063025904,-38.2944448203221,
-38.2061539011448,-38.1177629155512,-38.0293123272669,-37.9407324025286,
-37.9183319856413,-37.8297588363348,-37.7413000432852,-37.6529318309124,
-37.5613754950376,-37.473108851481,-37.3848554608637,-37.2965939785956,
-37.2083030594185,-37.1199120738252,-37.0314614855414,-36.9428815608032,
-36.9204811439139,-36.8319079946071,-36.7434492015572,-36.655080989184,
-36.5635246533093,-36.4752580097524,-36.387004619135,-36.2987431368667,
-36.2104522176887,-36.122061232095,-36.0336106438104,-35.9450307190722,
-35.9226303021865,-35.8250780891462,-35.7279166626066,-35.6310133554249,
-35.53449733819,-35.5086755762787),.UNSPECIFIED.);
#1466=B_SPLINE_CURVE_WITH_KNOTS('',3,(#48407,#48408,#48409,#48410,#48411,
#48412,#48413,#48414,#48415,#48416,#48417,#48418,#48419,#48420,#48421,#48422,
#48423,#48424,#48425,#48426,#48427,#48428,#48429,#48430,#48431,#48432,#48433,
#48434,#48435,#48436,#48437,#48438,#48439,#48440,#48441,#48442,#48443,#48444,
#48445,#48446,#48447,#48448,#48449,#48450,#48451,#48452,#48453,#48454,#48455,
#48456,#48457,#48458,#48459,#48460,#48461,#48462,#48463,#48464,#48465,#48466,
#48467,#48468,#48469,#48470,#48471,#48472,#48473,#48474,#48475,#48476,#48477,
#48478,#48479,#48480,#48481,#48482,#48483,#48484,#48485,#48486,#48487,#48488,
#48489,#48490,#48491,#48492,#48493,#48494,#48495,#48496,#48497,#48498,#48499,
#48500,#48501,#48502,#48503,#48504,#48505,#48506,#48507,#48508,#48509,#48510,
#48511,#48512,#48513,#48514,#48515,#48516,#48517,#48518,#48519,#48520,#48521,
#48522,#48523,#48524,#48525,#48526,#48527,#48528,#48529,#48530,#48531,#48532,
#48533,#48534,#48535,#48536,#48537,#48538,#48539,#48540,#48541,#48542,#48543,
#48544,#48545,#48546,#48547,#48548,#48549,#48550,#48551,#48552,#48553,#48554,
#48555,#48556,#48557,#48558,#48559,#48560,#48561,#48562,#48563,#48564,#48565,
#48566,#48567,#48568,#48569,#48570,#48571,#48572,#48573,#48574,#48575,#48576,
#48577,#48578,#48579,#48580,#48581,#48582,#48583,#48584,#48585,#48586,#48587,
#48588,#48589,#48590,#48591,#48592,#48593,#48594,#48595,#48596,#48597,#48598,
#48599,#48600,#48601,#48602,#48603,#48604,#48605,#48606,#48607,#48608,#48609,
#48610,#48611,#48612,#48613,#48614,#48615,#48616,#48617,#48618,#48619,#48620,
#48621,#48622,#48623,#48624,#48625,#48626,#48627,#48628,#48629,#48630,#48631,
#48632),.UNSPECIFIED.,.F.,.F.,(4,3,3,3,3,3,3,3,3,3,3,3,3,3,3,3,3,3,3,3,
3,3,3,3,3,3,3,3,3,3,3,3,3,3,3,3,3,3,3,3,3,3,3,3,3,3,3,3,3,3,3,3,3,3,3,3,
3,3,3,3,3,3,3,3,3,3,3,3,3,3,3,3,3,3,3,4),(-35.5086755760922,-35.4188811405786,
-35.3290503078016,-35.2391644975997,-35.1491420297501,-35.0590430664914,
-34.9687826180062,-34.9247794604591,-34.8362063111524,-34.7477475181026,
-34.65937930573,-34.5678229698552,-34.4795563262983,-34.3913029356809,-34.3030414534123,
-34.214750534235,-34.1263595486414,-34.0379089603574,-33.949329035619,-33.9269286187317,
-33.8383554694252,-33.7498966763755,-33.6615284640029,-33.5699721281281,
-33.4817054845714,-33.3934520939542,-33.3051906116858,-33.216899692509,
-33.1285087069156,-33.0400581186316,-32.9514781938935,-32.9290777770043,
-32.8405046276976,-32.7520458346479,-32.6636776222752,-32.5721212864004,
-32.4838546428434,-32.3956012522258,-32.3073397699572,-32.2190488507805,
-32.1306578651869,-32.0422072769025,-31.953627352164,-31.9312269352769,
-31.8426537859705,-31.7541949929209,-31.6658267805485,-31.5742704446736,
-31.4860038011169,-31.3977504104998,-31.3094889282317,-31.2211980090548,
-31.1328070234614,-31.0443564351774,-30.9557765104394,-30.9333760935495,
-30.8448029442431,-30.7563441511937,-30.667975938821,-30.5764196029462,
-30.4881529593893,-30.3998995687722,-30.3116380865043,-30.2233471673271,
-30.1349561817338,-30.0465055934498,-29.9579256687117,-29.9355252518221,
-29.8467708789584,-29.7589851521654,-29.6712833639532,-29.5836434327169,
-29.4941051417658,-29.4065070806612,-29.3159986747869,-29.2254902689126),
 .UNSPECIFIED.);
#1467=B_SPLINE_CURVE_WITH_KNOTS('',3,(#48634,#48635,#48636,#48637,#48638,
#48639,#48640,#48641,#48642,#48643,#48644,#48645,#48646,#48647,#48648,#48649,
#48650,#48651,#48652,#48653,#48654,#48655,#48656,#48657,#48658,#48659,#48660,
#48661,#48662,#48663,#48664,#48665,#48666,#48667,#48668,#48669,#48670,#48671,
#48672,#48673,#48674,#48675,#48676,#48677,#48678,#48679,#48680,#48681,#48682,
#48683,#48684,#48685,#48686,#48687,#48688,#48689,#48690,#48691,#48692,#48693,
#48694,#48695,#48696,#48697,#48698,#48699,#48700,#48701,#48702,#48703,#48704,
#48705,#48706,#48707,#48708,#48709,#48710,#48711,#48712,#48713,#48714,#48715,
#48716,#48717,#48718,#48719,#48720,#48721,#48722,#48723,#48724,#48725,#48726,
#48727,#48728,#48729,#48730,#48731,#48732,#48733,#48734,#48735,#48736,#48737,
#48738,#48739,#48740,#48741,#48742,#48743,#48744,#48745,#48746,#48747,#48748,
#48749,#48750,#48751,#48752,#48753,#48754,#48755,#48756,#48757,#48758,#48759,
#48760,#48761,#48762,#48763,#48764,#48765,#48766,#48767,#48768,#48769,#48770,
#48771,#48772,#48773,#48774,#48775,#48776,#48777,#48778,#48779,#48780,#48781,
#48782,#48783,#48784,#48785,#48786,#48787,#48788,#48789,#48790,#48791,#48792,
#48793,#48794,#48795,#48796,#48797,#48798,#48799,#48800,#48801,#48802,#48803,
#48804,#48805,#48806,#48807,#48808,#48809,#48810,#48811,#48812,#48813,#48814,
#48815,#48816,#48817,#48818,#48819,#48820,#48821,#48822,#48823,#48824,#48825,
#48826,#48827,#48828,#48829,#48830,#48831,#48832,#48833,#48834,#48835,#48836,
#48837,#48838,#48839,#48840,#48841,#48842,#48843,#48844,#48845,#48846,#48847,
#48848,#48849,#48850,#48851,#48852,#48853,#48854,#48855,#48856,#48857,#48858,
#48859,#48860,#48861,#48862),.UNSPECIFIED.,.F.,.F.,(4,3,3,3,3,3,3,3,3,3,
3,3,3,3,3,3,3,3,3,3,3,3,3,3,3,3,3,3,3,3,3,3,3,3,3,3,3,3,3,3,3,3,3,3,3,3,
3,3,3,3,3,3,3,3,3,3,3,3,3,3,3,3,3,3,3,3,3,3,3,3,3,3,3,3,3,3,4),(-29.2254902687766,
-29.1178017627057,-29.0085141589372,-28.9376744100947,-28.8491012607896,
-28.7606424677413,-28.6722742553701,-28.5807179194948,-28.4924512759394,
-28.4041978853234,-28.3159364030565,-28.2276454838808,-28.1392544982887,
-28.0508039100057,-27.9622239852688,-27.9398235683673,-27.8512504190617,
-27.7627916260131,-27.6744234136415,-27.5828670777663,-27.4946004342106,
-27.4063470435944,-27.3180855613272,-27.2297946421512,-27.1414036565588,
-27.0529530682758,-26.9643731435387,-26.9419727266399,-26.8533995773247,
-26.7649407842662,-26.676572571885,-26.5850162360134,-26.4967495924479,
-26.408496201822,-26.320234719545,-26.2319438003593,-26.1435528147574,-26.0551022264647,
-25.9665223017182,-25.9441218849125,-25.8555487356216,-25.7670899425876,
-25.6787217302307,-25.58716539435,-25.4988987508086,-25.4106453602066,-25.3223838779536,
-25.2340929587915,-25.1457019732128,-25.0572513849433,-24.9686714602193,
-24.9462710431851,-24.85769789388,-24.7692391008319,-24.680870888461,-24.5893145525856,
-24.5010479090309,-24.4127945184159,-24.3245330361501,-24.2362421169756,
-24.1478511313848,-24.0594005431034,-23.9708206183682,-23.9484202014577,
-23.8598470520801,-23.771388258959,-23.683020046515,-23.5914637106669,-23.5031970670388,
-23.4149436763502,-23.326682194011,-23.2383912747634,-23.1500002891001,
-23.0615497007464,-22.9729697759399,-22.9505693597303,-22.942304961733),
 .UNSPECIFIED.);
#1468=B_SPLINE_CURVE_WITH_KNOTS('',3,(#48864,#48865,#48866,#48867,#48868,
#48869,#48870,#48871,#48872,#48873,#48874,#48875,#48876,#48877,#48878,#48879,
#48880,#48881,#48882,#48883,#48884,#48885,#48886,#48887,#48888,#48889,#48890,
#48891,#48892,#48893,#48894,#48895,#48896,#48897,#48898,#48899,#48900,#48901,
#48902,#48903,#48904,#48905,#48906,#48907,#48908,#48909,#48910,#48911,#48912,
#48913,#48914,#48915,#48916,#48917,#48918,#48919,#48920,#48921,#48922,#48923,
#48924,#48925,#48926,#48927,#48928,#48929,#48930,#48931,#48932,#48933,#48934,
#48935,#48936,#48937,#48938,#48939,#48940,#48941,#48942,#48943,#48944,#48945,
#48946,#48947,#48948,#48949,#48950,#48951,#48952,#48953,#48954,#48955,#48956,
#48957,#48958,#48959,#48960,#48961,#48962,#48963,#48964,#48965,#48966,#48967,
#48968,#48969,#48970,#48971,#48972,#48973,#48974,#48975,#48976,#48977,#48978,
#48979,#48980,#48981,#48982,#48983,#48984,#48985,#48986,#48987,#48988,#48989,
#48990,#48991,#48992,#48993,#48994,#48995,#48996,#48997,#48998,#48999,#49000,
#49001,#49002,#49003,#49004,#49005,#49006,#49007,#49008,#49009,#49010,#49011,
#49012,#49013,#49014,#49015,#49016,#49017,#49018,#49019,#49020,#49021,#49022,
#49023,#49024,#49025,#49026,#49027,#49028,#49029,#49030,#49031,#49032,#49033,
#49034,#49035,#49036,#49037,#49038,#49039,#49040,#49041,#49042,#49043,#49044,
#49045,#49046,#49047,#49048,#49049,#49050,#49051,#49052,#49053,#49054,#49055,
#49056,#49057,#49058,#49059,#49060,#49061,#49062,#49063,#49064,#49065,#49066,
#49067,#49068,#49069,#49070,#49071,#49072,#49073,#49074,#49075,#49076,#49077,
#49078,#49079,#49080,#49081,#49082,#49083,#49084,#49085,#49086,#49087,#49088,
#49089),.UNSPECIFIED.,.F.,.F.,(4,3,3,3,3,3,3,3,3,3,3,3,3,3,3,3,3,3,3,3,
3,3,3,3,3,3,3,3,3,3,3,3,3,3,3,3,3,3,3,3,3,3,3,3,3,3,3,3,3,3,3,3,3,3,3,3,
3,3,3,3,3,3,3,3,3,3,3,3,3,3,3,3,3,3,3,4),(-22.9423049614834,-22.8538617632608,
-22.7655327557495,-22.6772940078544,-22.586722071623,-22.4985834260939,
-22.4104575188324,-22.3223228662375,-22.2299217791788,-22.1416543081962,
-22.0533253302847,-21.9648699208204,-21.9527185180029,-21.864145368657,
-21.7756865755694,-21.6873183631602,-21.5957620272996,-21.5074953837099,
-21.4192419930611,-21.3309805107628,-21.2426895915571,-21.1542986059373,
-21.065848017628,-20.9772680928667,-20.9548676762754,-20.8662945263978,
-20.7778357327747,-20.6894675198275,-20.5979111841676,-20.5096445400355,
-20.4213911488439,-20.3331296660026,-20.2448387462547,-20.1564477600963,
-20.0679971712501,-19.9794172459584,-19.957016834548,-19.8684436866929,
-19.7799848950942,-19.6916166841704,-19.6000603477517,-19.5117937056287,
-19.4235403164372,-19.3352788355856,-19.246987917814,-19.1585969336029,
-19.0701463466892,-18.9815664232938,-18.9591659928206,-18.8705928427052,
-18.7821340488582,-18.6937658357001,-18.6022095001243,-18.5139428558168,
-18.425689464463,-18.337427981473,-18.2491370615898,-18.1607460753165,-18.0722954863675,
-17.9837155609903,-17.9613151510932,-17.8727419973658,-17.7842831998724,
-17.6959149830392,-17.60435864883,-17.5160920007977,-17.4278386057074,-17.3395771189731,
-17.2512861953413,-17.1628952053342,-17.0744446126548,-16.9858646835816,
-16.9634643093658,-16.856206513481,-16.7502366022154,-16.6591196547223),
 .UNSPECIFIED.);
#1469=B_SPLINE_CURVE_WITH_KNOTS('',3,(#49091,#49092,#49093,#49094,#49095,
#49096,#49097,#49098,#49099,#49100,#49101,#49102,#49103,#49104,#49105,#49106,
#49107,#49108,#49109,#49110,#49111,#49112,#49113,#49114,#49115,#49116,#49117,
#49118,#49119,#49120,#49121,#49122,#49123,#49124,#49125,#49126,#49127,#49128,
#49129,#49130,#49131,#49132,#49133,#49134,#49135,#49136,#49137,#49138,#49139,
#49140,#49141,#49142,#49143,#49144,#49145,#49146,#49147,#49148,#49149,#49150,
#49151,#49152,#49153,#49154,#49155,#49156,#49157,#49158,#49159,#49160,#49161,
#49162,#49163,#49164,#49165,#49166,#49167,#49168,#49169,#49170,#49171,#49172,
#49173,#49174,#49175,#49176,#49177,#49178,#49179,#49180,#49181,#49182,#49183,
#49184,#49185,#49186,#49187,#49188,#49189,#49190,#49191,#49192,#49193,#49194,
#49195,#49196,#49197,#49198,#49199,#49200,#49201,#49202,#49203,#49204,#49205,
#49206,#49207,#49208,#49209,#49210,#49211,#49212,#49213,#49214,#49215,#49216,
#49217,#49218,#49219,#49220,#49221,#49222,#49223,#49224,#49225,#49226,#49227,
#49228,#49229,#49230,#49231,#49232,#49233,#49234,#49235,#49236,#49237,#49238,
#49239,#49240,#49241,#49242,#49243,#49244,#49245,#49246,#49247,#49248,#49249,
#49250,#49251,#49252,#49253,#49254,#49255,#49256,#49257,#49258,#49259,#49260,
#49261,#49262,#49263,#49264,#49265,#49266,#49267,#49268,#49269,#49270,#49271,
#49272,#49273,#49274,#49275,#49276,#49277,#49278,#49279,#49280,#49281,#49282,
#49283,#49284,#49285,#49286,#49287,#49288,#49289,#49290,#49291,#49292,#49293,
#49294,#49295,#49296,#49297,#49298,#49299,#49300,#49301,#49302,#49303,#49304,
#49305,#49306,#49307,#49308,#49309,#49310,#49311,#49312,#49313,#49314,#49315,
#49316),.UNSPECIFIED.,.F.,.F.,(4,3,3,3,3,3,3,3,3,3,3,3,3,3,3,3,3,3,3,3,
3,3,3,3,3,3,3,3,3,3,3,3,3,3,3,3,3,3,3,3,3,3,3,3,3,3,3,3,3,3,3,3,3,3,3,3,
3,3,3,3,3,3,3,3,3,3,3,3,3,3,3,3,3,3,3,4),(-16.6591196545534,-16.5712935284758,
-16.4834950042179,-16.3957022954975,-16.3078936252478,-16.2199901013344,
-16.1320383660111,-16.0439386197209,-15.9656134676384,-15.8770403071815,
-15.7885815030742,-15.700213279748,-15.6086569480184,-15.520390293833,-15.4321368927246,
-15.3438754001135,-15.2555844707522,-15.1671934752597,-15.0787428772304,
-14.9901629430461,-14.967762625911,-14.8791894440136,-14.7907306181554,
-14.7023623727974,-14.6108060492207,-14.5225393724502,-14.4342859485921,
-14.3460244330919,-14.257733480728,-14.1693424621828,-14.0808918410441,
-13.992311883847,-13.9699117841836,-13.8813387560594,-13.7928800842836,
-13.7045119931345,-13.6129556117997,-13.5246890885827,-13.4364358177753,
-13.3481744546603,-13.2598836538524,-13.1714927848746,-13.0830423123262,
-12.9944625011488,-12.9720609424562,-12.8834876608346,-12.7950287362,-12.7066603931155,
-12.6151041065671,-12.5268373352663,-12.4385838182129,-12.350322210946,
-12.2620311683396,-12.1736400622478,-12.0851893550264,-11.9966093145385,
-11.9742101007288,-11.8856367279759,-11.7971777094444,-11.7088092698459,
-11.6172530184903,-11.5289861448337,-11.4407325234554,-11.3524708100167,
-11.2641796595118,-11.1757884435396,-11.0873376251498,-10.9987574724895,
-10.9763592590014,-10.8865298425373,-10.7968247825165,-10.7072244088575,
-10.6177240485907,-10.5282826535782,-10.4388779894314,-10.3759343473738),
 .UNSPECIFIED.);
#1470=B_SPLINE_CURVE_WITH_KNOTS('',3,(#49317,#49318,#49319,#49320,#49321,
#49322,#49323,#49324,#49325,#49326,#49327,#49328,#49329,#49330,#49331,#49332,
#49333,#49334,#49335,#49336,#49337,#49338,#49339,#49340,#49341,#49342,#49343,
#49344,#49345,#49346,#49347,#49348,#49349,#49350,#49351,#49352,#49353,#49354,
#49355,#49356,#49357,#49358,#49359,#49360,#49361,#49362,#49363,#49364,#49365,
#49366,#49367,#49368,#49369,#49370,#49371,#49372,#49373,#49374,#49375,#49376,
#49377,#49378,#49379,#49380,#49381,#49382,#49383,#49384,#49385,#49386,#49387,
#49388,#49389,#49390,#49391,#49392,#49393,#49394,#49395,#49396,#49397,#49398,
#49399,#49400,#49401,#49402,#49403,#49404,#49405,#49406,#49407,#49408,#49409,
#49410,#49411,#49412,#49413,#49414,#49415,#49416,#49417,#49418,#49419,#49420,
#49421,#49422,#49423,#49424,#49425,#49426,#49427,#49428,#49429,#49430,#49431,
#49432,#49433,#49434,#49435,#49436,#49437,#49438,#49439,#49440,#49441,#49442,
#49443,#49444,#49445,#49446,#49447,#49448,#49449,#49450,#49451,#49452,#49453,
#49454,#49455,#49456,#49457,#49458,#49459,#49460,#49461,#49462,#49463,#49464,
#49465,#49466,#49467,#49468,#49469,#49470,#49471,#49472,#49473,#49474,#49475,
#49476,#49477,#49478,#49479,#49480,#49481,#49482,#49483,#49484,#49485,#49486,
#49487,#49488,#49489,#49490,#49491,#49492,#49493,#49494,#49495,#49496,#49497,
#49498,#49499,#49500,#49501,#49502,#49503,#49504,#49505,#49506,#49507,#49508,
#49509,#49510,#49511,#49512,#49513,#49514,#49515,#49516,#49517,#49518,#49519,
#49520,#49521,#49522,#49523,#49524,#49525,#49526,#49527,#49528,#49529,#49530,
#49531,#49532,#49533,#49534,#49535,#49536,#49537,#49538,#49539,#49540,#49541,
#49542),.UNSPECIFIED.,.F.,.F.,(4,3,3,3,3,3,3,3,3,3,3,3,3,3,3,3,3,3,3,3,
3,3,3,3,3,3,3,3,3,3,3,3,3,3,3,3,3,3,3,3,3,3,3,3,3,3,3,3,3,3,3,3,3,3,3,3,
3,3,3,3,3,3,3,3,3,3,3,3,3,3,3,3,3,3,3,4),(-10.3759343471667,-10.2765778646935,
-10.1785460227179,-10.078527219996,-9.97850841727403,-9.88993382098927,
-9.80147358648194,-9.71310393977095,-9.62154814424291,-9.53328009285517,
-9.44502530654547,-9.356762442169,-9.26847015592512,-9.18007783230482,-9.0916259212877,
-9.00304470626163,-8.98065757554662,-8.89208307541407,-8.80362291295577,
-8.7152533144443,-8.62369749186617,-8.53542942965111,-8.44717461086563,
-8.35891169250639,-8.27061933089823,-8.18222690092591,-8.09377486537985,
-8.0051935004333,-7.98280673381922,-7.89424283763284,-7.80579331569487,
-7.71743438141468,-7.62587457024933,-7.53761716398574,-7.44937297991607,
-7.36112066369019,-7.27283886025113,-7.18445687012472,-7.0960152181745,
-7.00744407462594,-6.98495589209182,-6.89636773805667,-6.80789397960917,
-6.71951085805653,-6.62796013209501,-6.53967881125381,-6.45141085365402,
-6.36313492991273,-6.27482971008726,-6.18642470340815,-6.09796023994667,
-6.00936675923615,-5.98710505036441,-5.89852582996034,-5.81006079982164,
-5.72168619395215,-5.63013219578775,-5.54185881368928,-5.45359856941143,
-5.36533012633129,-5.27703214708557,-5.18863399181092,-5.10017616132864,
-5.01158894546892,-4.98925420863701,-4.90186357593316,-4.8145865543858,
-4.72435686514095,-4.63723281771054,-4.55013980149263,-4.46305541288891,
-4.37595725988714,-4.28877946463819,-4.20155379976352,-4.11421368393324,
-4.09274904042707),.UNSPECIFIED.);
#1471=B_SPLINE_CURVE_WITH_KNOTS('',3,(#49545,#49546,#49547,#49548,#49549,
#49550,#49551,#49552,#49553,#49554,#49555,#49556,#49557,#49558,#49559,#49560,
#49561,#49562,#49563,#49564,#49565,#49566,#49567,#49568,#49569,#49570,#49571,
#49572,#49573,#49574,#49575,#49576,#49577,#49578,#49579,#49580,#49581,#49582,
#49583,#49584,#49585,#49586,#49587,#49588,#49589,#49590,#49591,#49592,#49593,
#49594,#49595,#49596,#49597,#49598,#49599,#49600,#49601,#49602,#49603,#49604,
#49605,#49606,#49607,#49608,#49609,#49610,#49611,#49612,#49613,#49614,#49615,
#49616,#49617,#49618,#49619,#49620,#49621,#49622,#49623,#49624,#49625,#49626,
#49627,#49628,#49629,#49630,#49631,#49632,#49633,#49634,#49635,#49636,#49637,
#49638,#49639,#49640,#49641,#49642,#49643,#49644,#49645,#49646,#49647,#49648,
#49649,#49650,#49651,#49652,#49653,#49654,#49655,#49656,#49657,#49658,#49659,
#49660,#49661,#49662,#49663,#49664,#49665,#49666,#49667,#49668,#49669,#49670,
#49671,#49672,#49673,#49674,#49675,#49676,#49677,#49678,#49679,#49680,#49681,
#49682,#49683,#49684,#49685,#49686,#49687,#49688,#49689,#49690,#49691,#49692,
#49693,#49694,#49695,#49696,#49697,#49698,#49699,#49700,#49701,#49702,#49703,
#49704,#49705,#49706),.UNSPECIFIED.,.F.,.F.,(4,2,2,2,2,2,2,2,2,2,2,2,2,
2,2,2,2,2,2,2,2,2,2,2,2,2,2,2,2,2,2,2,2,2,2,2,2,2,2,2,2,2,2,2,2,2,2,2,2,
2,2,2,2,2,2,2,2,2,2,2,2,2,2,2,2,2,2,2,2,2,2,2,2,2,2,2,2,2,2,2,4),(0.00572882946113452,
0.0858386630726596,0.128530379570816,0.137096238848039,0.141978642636408,
0.146211956682032,0.151420454865605,0.159390663536531,0.202369071154075,
0.284374251605654,0.291998189895998,0.297842832080111,0.30076460715983,
0.300782700221492,0.300801156447523,0.300819988452636,0.300839209400581,
0.300858833374834,0.300878875067341,0.300899349764534,0.300920273768506,
0.30094166412418,0.300963538183928,0.300985914819345,0.301008813921572,
0.303334801482,0.306215030609676,0.311717802906198,0.34956040350371,0.406195092989925,
0.433847186656547,0.451856562766573,0.458370988167906,0.462800764011346,
0.467118672123479,0.473289241546835,0.484640963324567,0.547060728319788,
0.608701862231486,0.618469998357093,0.622076456951003,0.624532691107509,
0.626740828914197,0.629788136753773,0.63754739348344,0.69974886415569,0.747007760150307,
0.764006113963808,0.776517543366181,0.782137357791307,0.786367015930682,
0.79090932885459,0.798106135295086,0.820064585285403,0.918326337184996,
0.932306484492328,0.94155550709373,0.945064879357327,0.947486494283003,
0.949713163098311,0.952816722292652,0.9609201408115,1.01180389452782,1.05675228723629,
1.09396577086912,1.10220036045524,1.10698869991128,1.11119611958505,1.11644450890454,
1.12461079772995,1.17366338651836,1.20360532452736,1.25913975687919,1.26508690319042,
1.2680420026153,1.27017188826653,1.27290945616808,1.27769552544157,1.29786694630185,
1.36971036920056,1.36986813415593),.UNSPECIFIED.);
#1472=B_SPLINE_CURVE_WITH_KNOTS('',3,(#49710,#49711,#49712,#49713,#49714,
#49715,#49716,#49717,#49718,#49719,#49720,#49721,#49722,#49723,#49724,#49725,
#49726,#49727,#49728,#49729,#49730,#49731,#49732,#49733,#49734,#49735,#49736,
#49737,#49738,#49739,#49740),.UNSPECIFIED.,.F.,.F.,(4,3,3,3,3,3,3,3,3,3,
4),(135.088484104672,135.18316969008,135.277709840149,135.372951171501,
135.46726055986,135.561508187356,135.655716424704,135.751697441269,135.845921119761,
135.942780805363,136.039640490965),.UNSPECIFIED.);
#1473=B_SPLINE_CURVE_WITH_KNOTS('',3,(#49741,#49742,#49743,#49744,#49745,
#49746,#49747,#49748,#49749,#49750,#49751,#49752,#49753,#49754,#49755,#49756,
#49757,#49758,#49759,#49760,#49761,#49762,#49763,#49764,#49765,#49766,#49767,
#49768,#49769,#49770,#49771,#49772,#49773,#49774,#49775,#49776,#49777,#49778,
#49779,#49780,#49781,#49782,#49783,#49784,#49785,#49786,#49787,#49788,#49789,
#49790,#49791,#49792,#49793,#49794,#49795,#49796,#49797,#49798,#49799,#49800,
#49801,#49802,#49803,#49804,#49805,#49806,#49807,#49808,#49809,#49810,#49811,
#49812,#49813),.UNSPECIFIED.,.F.,.F.,(4,3,3,3,3,3,3,3,3,3,3,3,3,3,3,3,3,
3,3,3,3,3,3,3,4),(133.042160362488,133.046087965783,133.139181123038,133.232150309801,
133.325023106835,133.41783094323,133.510605411329,133.603371293728,133.69615335931,
133.789036617055,133.881973115032,133.97506575282,134.043938807511,134.136312444951,
134.228560254826,134.320710715063,134.41279766222,134.504852253225,134.596900055539,
134.688966624987,134.781142826853,134.873375725362,134.965777975913,135.041789649238,
135.088484104361),.UNSPECIFIED.);
#1474=B_SPLINE_CURVE_WITH_KNOTS('',3,(#50338,#50339,#50340,#50341,#50342,
#50343,#50344,#50345,#50346,#50347,#50348,#50349,#50350,#50351,#50352,#50353,
#50354,#50355,#50356,#50357,#50358,#50359,#50360,#50361,#50362,#50363,#50364,
#50365,#50366,#50367,#50368,#50369,#50370,#50371,#50372,#50373,#50374,#50375,
#50376,#50377,#50378,#50379,#50380,#50381,#50382,#50383,#50384,#50385,#50386,
#50387,#50388,#50389,#50390,#50391,#50392,#50393,#50394,#50395,#50396,#50397,
#50398,#50399,#50400,#50401,#50402,#50403,#50404,#50405,#50406,#50407,#50408,
#50409,#50410,#50411,#50412,#50413,#50414,#50415,#50416,#50417,#50418,#50419,
#50420,#50421,#50422,#50423,#50424,#50425,#50426,#50427,#50428,#50429,#50430,
#50431,#50432,#50433,#50434),.UNSPECIFIED.,.F.,.F.,(4,3,3,3,3,3,3,3,3,3,
3,3,3,3,3,3,3,3,3,3,3,3,3,3,3,3,3,3,3,3,3,3,4),(0.,0.0258260740408245,0.0620924490441423,
0.0993874343281711,0.1366824196122,0.147698904723131,0.154011882090748,
0.189860980974716,0.225553852485871,0.260975001327923,0.278622120241529,
0.288544671238274,0.295091750966326,0.299504106250136,0.334017275552874,
0.368084614094821,0.402151952636769,0.423542327420144,0.431067342396322,
0.436302863184041,0.441119634191273,0.474541969017029,0.508522660804976,
0.54221649566577,0.567489177353895,0.575255797857681,0.608314732463416,
0.642335536640254,0.657701460359135,0.662771582070671,0.694603710062296,
0.725562408530676,0.744397949170667),.UNSPECIFIED.);
#1475=B_SPLINE_CURVE_WITH_KNOTS('',3,(#50435,#50436,#50437,#50438,#50439,
#50440,#50441,#50442,#50443,#50444,#50445,#50446,#50447,#50448,#50449,#50450,
#50451,#50452,#50453,#50454,#50455,#50456,#50457,#50458,#50459,#50460,#50461,
#50462,#50463,#50464,#50465,#50466,#50467,#50468,#50469,#50470,#50471,#50472,
#50473,#50474,#50475,#50476,#50477,#50478,#50479,#50480,#50481,#50482,#50483,
#50484,#50485,#50486,#50487,#50488,#50489,#50490,#50491,#50492,#50493,#50494,
#50495,#50496,#50497,#50498,#50499,#50500,#50501,#50502,#50503,#50504,#50505,
#50506,#50507,#50508,#50509,#50510,#50511,#50512,#50513,#50514,#50515,#50516,
#50517,#50518,#50519,#50520,#50521,#50522,#50523,#50524,#50525,#50526,#50527,
#50528),.UNSPECIFIED.,.F.,.F.,(4,3,3,3,3,3,3,3,3,3,3,3,3,3,3,3,3,3,3,3,
3,3,3,3,3,3,3,3,3,3,3,4),(0.,0.02133074521375,0.0521058403411437,0.0836372654726391,
0.115777344688116,0.125964402355647,0.130783277975323,0.163735803941014,
0.196688329906704,0.230204779895922,0.2470278046079,0.259364835821699,0.264033725823834,
0.298484782009355,0.332689762691114,0.364788977591745,0.388319089517656,
0.39509149622043,0.401763599284906,0.435343669494579,0.46974042676872,0.504994131658741,
0.534528711252189,0.540952849586392,0.546662686863921,0.582645576684806,
0.61886768806574,0.635179337184303,0.644573291322463,0.681413951419206,
0.717770742894507,0.741270768406323),.UNSPECIFIED.);
#1476=B_SPLINE_CURVE_WITH_KNOTS('',3,(#51054,#51055,#51056,#51057,#51058,
#51059,#51060,#51061,#51062,#51063,#51064,#51065,#51066,#51067,#51068,#51069,
#51070,#51071,#51072,#51073,#51074,#51075,#51076,#51077,#51078,#51079,#51080,
#51081,#51082,#51083,#51084,#51085,#51086,#51087,#51088,#51089,#51090,#51091,
#51092,#51093,#51094,#51095,#51096,#51097,#51098,#51099,#51100,#51101,#51102,
#51103,#51104,#51105,#51106,#51107,#51108,#51109,#51110,#51111,#51112,#51113,
#51114,#51115,#51116,#51117,#51118,#51119,#51120,#51121,#51122,#51123,#51124,
#51125,#51126,#51127,#51128,#51129,#51130,#51131,#51132,#51133,#51134,#51135,
#51136,#51137,#51138,#51139,#51140,#51141,#51142,#51143,#51144,#51145,#51146,
#51147),.UNSPECIFIED.,.F.,.F.,(4,3,3,3,3,3,3,3,3,3,3,3,3,3,3,3,3,3,3,3,
3,3,3,3,3,3,3,3,3,3,3,4),(0.,0.0213307452137482,0.0521058429544939,0.0836372697852673,
0.115777349637711,0.125964407042121,0.130783279244603,0.163312913916928,
0.196758848298764,0.2302047826806,0.247027807044509,0.259364835465739,0.264033725682642,
0.298484781608584,0.332689762447923,0.364788977591868,0.388319089517784,
0.395091496414565,0.401763599093259,0.435752013864845,0.469740428636431,
0.504994134467813,0.534528713710151,0.540952860096086,0.546662689054415,
0.582787099736608,0.618867691358632,0.635179341901767,0.644573290300076,
0.681413950020179,0.717770738127119,0.741270768406402),.UNSPECIFIED.);
#1477=B_SPLINE_CURVE_WITH_KNOTS('',3,(#51148,#51149,#51150,#51151),
 .UNSPECIFIED.,.F.,.F.,(4,4),(0.,0.0148373890450924),.UNSPECIFIED.);
#1478=B_SPLINE_CURVE_WITH_KNOTS('',3,(#51152,#51153,#51154,#51155,#51156,
#51157,#51158,#51159,#51160,#51161,#51162,#51163,#51164,#51165,#51166,#51167,
#51168,#51169,#51170,#51171,#51172,#51173,#51174,#51175,#51176,#51177,#51178,
#51179,#51180,#51181,#51182,#51183,#51184,#51185,#51186,#51187,#51188,#51189,
#51190,#51191,#51192,#51193,#51194,#51195,#51196,#51197,#51198,#51199,#51200,
#51201,#51202,#51203,#51204,#51205,#51206,#51207,#51208,#51209,#51210,#51211,
#51212,#51213,#51214,#51215,#51216,#51217,#51218,#51219,#51220,#51221,#51222,
#51223,#51224,#51225,#51226,#51227,#51228,#51229,#51230,#51231,#51232,#51233,
#51234,#51235,#51236,#51237,#51238,#51239,#51240,#51241,#51242,#51243,#51244,
#51245,#51246,#51247,#51248),.UNSPECIFIED.,.F.,.F.,(4,3,3,3,3,3,3,3,3,3,
3,3,3,3,3,3,3,3,3,3,3,3,3,3,3,3,3,3,3,3,3,3,4),(0.,0.0258260740408234,0.0622921374233043,
0.0987582008057851,0.136682419784644,0.147698905558292,0.154011882323251,
0.189890297854231,0.2256941807755,0.260975004111818,0.278622122677423,0.288544677172356,
0.295091839955112,0.299504264726676,0.334017433622103,0.368084693129378,
0.402151952636654,0.423542327420026,0.431067342051171,0.436302864295339,
0.441119634363373,0.474541971383567,0.508522662666217,0.542216494901936,
0.567489176685521,0.575255797837762,0.608314730465952,0.642335535142118,
0.657701457701357,0.662771579392012,0.694603703469968,0.725562396845423,
0.744397949170615),.UNSPECIFIED.);
#1479=B_SPLINE_CURVE_WITH_KNOTS('',3,(#51266,#51267,#51268,#51269),
 .UNSPECIFIED.,.F.,.F.,(4,4),(-0.453207372117249,-0.354837975954888),
 .UNSPECIFIED.);
#1480=B_SPLINE_CURVE_WITH_KNOTS('',3,(#51466,#51467,#51468,#51469,#51470,
#51471,#51472,#51473),.UNSPECIFIED.,.F.,.F.,(4,2,2,4),(2.26932848662342,
2.45137478361407,2.63342108060473,2.80969614393453),.UNSPECIFIED.);
#1481=B_SPLINE_CURVE_WITH_KNOTS('',3,(#51474,#51475,#51476,#51477,#51478,
#51479,#51480,#51481),.UNSPECIFIED.,.F.,.F.,(4,2,2,4),(1.72896082931231,
1.90523589264212,2.08728218963277,2.26932848662342),.UNSPECIFIED.);
#1482=VERTEX_POINT('',#5530);
#1483=VERTEX_POINT('',#5531);
#1484=VERTEX_POINT('',#5536);
#1485=VERTEX_POINT('',#5538);
#1486=VERTEX_POINT('',#5540);
#1487=VERTEX_POINT('',#5542);
#1488=VERTEX_POINT('',#5544);
#1489=VERTEX_POINT('',#5548);
#1490=VERTEX_POINT('',#5550);
#1491=VERTEX_POINT('',#5552);
#1492=VERTEX_POINT('',#5554);
#1493=VERTEX_POINT('',#5558);
#1494=VERTEX_POINT('',#5560);
#1495=VERTEX_POINT('',#5562);
#1496=VERTEX_POINT('',#5564);
#1497=VERTEX_POINT('',#5566);
#1498=VERTEX_POINT('',#5568);
#1499=VERTEX_POINT('',#5570);
#1500=VERTEX_POINT('',#5573);
#1501=VERTEX_POINT('',#5576);
#1502=VERTEX_POINT('',#5580);
#1503=VERTEX_POINT('',#5582);
#1504=VERTEX_POINT('',#5584);
#1505=VERTEX_POINT('',#5586);
#1506=VERTEX_POINT('',#5588);
#1507=VERTEX_POINT('',#5591);
#1508=VERTEX_POINT('',#5594);
#1509=VERTEX_POINT('',#5610);
#1510=VERTEX_POINT('',#5614);
#1511=VERTEX_POINT('',#5616);
#1512=VERTEX_POINT('',#5620);
#1513=VERTEX_POINT('',#5621);
#1514=VERTEX_POINT('',#5623);
#1515=VERTEX_POINT('',#5625);
#1516=VERTEX_POINT('',#5629);
#1517=VERTEX_POINT('',#5631);
#1518=VERTEX_POINT('',#5635);
#1519=VERTEX_POINT('',#5637);
#1520=VERTEX_POINT('',#5641);
#1521=VERTEX_POINT('',#5643);
#1522=VERTEX_POINT('',#5647);
#1523=VERTEX_POINT('',#5649);
#1524=VERTEX_POINT('',#5653);
#1525=VERTEX_POINT('',#5655);
#1526=VERTEX_POINT('',#5659);
#1527=VERTEX_POINT('',#5661);
#1528=VERTEX_POINT('',#5668);
#1529=VERTEX_POINT('',#5669);
#1530=VERTEX_POINT('',#5671);
#1531=VERTEX_POINT('',#5673);
#1532=VERTEX_POINT('',#5680);
#1533=VERTEX_POINT('',#5682);
#1534=VERTEX_POINT('',#5686);
#1535=VERTEX_POINT('',#5688);
#1536=VERTEX_POINT('',#5692);
#1537=VERTEX_POINT('',#5694);
#1538=VERTEX_POINT('',#5698);
#1539=VERTEX_POINT('',#5700);
#1540=VERTEX_POINT('',#5704);
#1541=VERTEX_POINT('',#5706);
#1542=VERTEX_POINT('',#5710);
#1543=VERTEX_POINT('',#5712);
#1544=VERTEX_POINT('',#5716);
#1545=VERTEX_POINT('',#5718);
#1546=VERTEX_POINT('',#5728);
#1547=VERTEX_POINT('',#5729);
#1548=VERTEX_POINT('',#5731);
#1549=VERTEX_POINT('',#5763);
#1550=VERTEX_POINT('',#5860);
#1551=VERTEX_POINT('',#5861);
#1552=VERTEX_POINT('',#6294);
#1553=VERTEX_POINT('',#6295);
#1554=VERTEX_POINT('',#6704);
#1555=VERTEX_POINT('',#6705);
#1556=VERTEX_POINT('',#6943);
#1557=VERTEX_POINT('',#7181);
#1558=VERTEX_POINT('',#7182);
#1559=VERTEX_POINT('',#7184);
#1560=VERTEX_POINT('',#7716);
#1561=VERTEX_POINT('',#7717);
#1562=VERTEX_POINT('',#8148);
#1563=VERTEX_POINT('',#8149);
#1564=VERTEX_POINT('',#8371);
#1565=VERTEX_POINT('',#8597);
#1566=VERTEX_POINT('',#8598);
#1567=VERTEX_POINT('',#8600);
#1568=VERTEX_POINT('',#8829);
#1569=VERTEX_POINT('',#9057);
#1570=VERTEX_POINT('',#9058);
#1571=VERTEX_POINT('',#9060);
#1572=VERTEX_POINT('',#9516);
#1573=VERTEX_POINT('',#9517);
#1574=VERTEX_POINT('',#9944);
#1575=VERTEX_POINT('',#9945);
#1576=VERTEX_POINT('',#10161);
#1577=VERTEX_POINT('',#10387);
#1578=VERTEX_POINT('',#10388);
#1579=VERTEX_POINT('',#10390);
#1580=VERTEX_POINT('',#10838);
#1581=VERTEX_POINT('',#10839);
#1582=VERTEX_POINT('',#11294);
#1583=VERTEX_POINT('',#11295);
#1584=VERTEX_POINT('',#11517);
#1585=VERTEX_POINT('',#11751);
#1586=VERTEX_POINT('',#11752);
#1587=VERTEX_POINT('',#11754);
#1588=VERTEX_POINT('',#12290);
#1589=VERTEX_POINT('',#12291);
#1590=VERTEX_POINT('',#12293);
#1591=VERTEX_POINT('',#12298);
#1592=VERTEX_POINT('',#12495);
#1593=VERTEX_POINT('',#12747);
#1594=VERTEX_POINT('',#12748);
#1595=VERTEX_POINT('',#12757);
#1596=VERTEX_POINT('',#12759);
#1597=VERTEX_POINT('',#12766);
#1598=VERTEX_POINT('',#12768);
#1599=VERTEX_POINT('',#12775);
#1600=VERTEX_POINT('',#12777);
#1601=VERTEX_POINT('',#12784);
#1602=VERTEX_POINT('',#12786);
#1603=VERTEX_POINT('',#12793);
#1604=VERTEX_POINT('',#12795);
#1605=VERTEX_POINT('',#12802);
#1606=VERTEX_POINT('',#12804);
#1607=VERTEX_POINT('',#12811);
#1608=VERTEX_POINT('',#12813);
#1609=VERTEX_POINT('',#12820);
#1610=VERTEX_POINT('',#12822);
#1611=VERTEX_POINT('',#12827);
#1612=VERTEX_POINT('',#12829);
#1613=VERTEX_POINT('',#12838);
#1614=VERTEX_POINT('',#12840);
#1615=VERTEX_POINT('',#12847);
#1616=VERTEX_POINT('',#12849);
#1617=VERTEX_POINT('',#12858);
#1618=VERTEX_POINT('',#12860);
#1619=VERTEX_POINT('',#12869);
#1620=VERTEX_POINT('',#12871);
#1621=VERTEX_POINT('',#12882);
#1622=VERTEX_POINT('',#12887);
#1623=VERTEX_POINT('',#12892);
#1624=VERTEX_POINT('',#12901);
#1625=VERTEX_POINT('',#12964);
#1626=VERTEX_POINT('',#12971);
#1627=VERTEX_POINT('',#12983);
#1628=VERTEX_POINT('',#12988);
#1629=VERTEX_POINT('',#12993);
#1630=VERTEX_POINT('',#12995);
#1631=VERTEX_POINT('',#13084);
#1632=VERTEX_POINT('',#13091);
#1633=VERTEX_POINT('',#13294);
#1634=VERTEX_POINT('',#13305);
#1635=VERTEX_POINT('',#13532);
#1636=VERTEX_POINT('',#13544);
#1637=VERTEX_POINT('',#13771);
#1638=VERTEX_POINT('',#13998);
#1639=VERTEX_POINT('',#14010);
#1640=VERTEX_POINT('',#14237);
#1641=VERTEX_POINT('',#14464);
#1642=VERTEX_POINT('',#14475);
#1643=VERTEX_POINT('',#14705);
#1644=VERTEX_POINT('',#14716);
#1645=VERTEX_POINT('',#14727);
#1646=VERTEX_POINT('',#14951);
#1647=VERTEX_POINT('',#14962);
#1648=VERTEX_POINT('',#15189);
#1649=VERTEX_POINT('',#15198);
#1650=VERTEX_POINT('',#15200);
#1651=VERTEX_POINT('',#15388);
#1652=VERTEX_POINT('',#15399);
#1653=VERTEX_POINT('',#15626);
#1654=VERTEX_POINT('',#15853);
#1655=VERTEX_POINT('',#15864);
#1656=VERTEX_POINT('',#16094);
#1657=VERTEX_POINT('',#16324);
#1658=VERTEX_POINT('',#16335);
#1659=VERTEX_POINT('',#16562);
#1660=VERTEX_POINT('',#16573);
#1661=VERTEX_POINT('',#16585);
#1662=VERTEX_POINT('',#16812);
#1663=VERTEX_POINT('',#16823);
#1664=VERTEX_POINT('',#17050);
#1665=VERTEX_POINT('',#17277);
#1666=VERTEX_POINT('',#18724);
#1667=VERTEX_POINT('',#25102);
#1668=VERTEX_POINT('',#25103);
#1669=VERTEX_POINT('',#25105);
#1670=VERTEX_POINT('',#25111);
#1671=VERTEX_POINT('',#25118);
#1672=VERTEX_POINT('',#25119);
#1673=VERTEX_POINT('',#25121);
#1674=VERTEX_POINT('',#25136);
#1675=VERTEX_POINT('',#25339);
#1676=VERTEX_POINT('',#25340);
#1677=VERTEX_POINT('',#25342);
#1678=VERTEX_POINT('',#25541);
#1679=VERTEX_POINT('',#25761);
#1680=VERTEX_POINT('',#25762);
#1681=VERTEX_POINT('',#25764);
#1682=VERTEX_POINT('',#25800);
#1683=VERTEX_POINT('',#25834);
#1684=VERTEX_POINT('',#25835);
#1685=VERTEX_POINT('',#25837);
#1686=VERTEX_POINT('',#25851);
#1687=VERTEX_POINT('',#26042);
#1688=VERTEX_POINT('',#26133);
#1689=VERTEX_POINT('',#26134);
#1690=VERTEX_POINT('',#26136);
#1691=VERTEX_POINT('',#26481);
#1692=VERTEX_POINT('',#26482);
#1693=VERTEX_POINT('',#26484);
#1694=VERTEX_POINT('',#26836);
#1695=VERTEX_POINT('',#26837);
#1696=VERTEX_POINT('',#26839);
#1697=VERTEX_POINT('',#27185);
#1698=VERTEX_POINT('',#27228);
#1699=VERTEX_POINT('',#27241);
#1700=VERTEX_POINT('',#27246);
#1701=VERTEX_POINT('',#27419);
#1702=VERTEX_POINT('',#27421);
#1703=VERTEX_POINT('',#27559);
#1704=VERTEX_POINT('',#28047);
#1705=VERTEX_POINT('',#28048);
#1706=VERTEX_POINT('',#28050);
#1707=VERTEX_POINT('',#28052);
#1708=VERTEX_POINT('',#28054);
#1709=VERTEX_POINT('',#28056);
#1710=VERTEX_POINT('',#28060);
#1711=VERTEX_POINT('',#28062);
#1712=VERTEX_POINT('',#28066);
#1713=VERTEX_POINT('',#28070);
#1714=VERTEX_POINT('',#28074);
#1715=VERTEX_POINT('',#28078);
#1716=VERTEX_POINT('',#28086);
#1717=VERTEX_POINT('',#28088);
#1718=VERTEX_POINT('',#28092);
#1719=VERTEX_POINT('',#28094);
#1720=VERTEX_POINT('',#28098);
#1721=VERTEX_POINT('',#28103);
#1722=VERTEX_POINT('',#28106);
#1723=VERTEX_POINT('',#28113);
#1724=VERTEX_POINT('',#28114);
#1725=VERTEX_POINT('',#28116);
#1726=VERTEX_POINT('',#28123);
#1727=VERTEX_POINT('',#28223);
#1728=VERTEX_POINT('',#28224);
#1729=VERTEX_POINT('',#28226);
#1730=VERTEX_POINT('',#28375);
#1731=VERTEX_POINT('',#28595);
#1732=VERTEX_POINT('',#28596);
#1733=VERTEX_POINT('',#28598);
#1734=VERTEX_POINT('',#28820);
#1735=VERTEX_POINT('',#29040);
#1736=VERTEX_POINT('',#29041);
#1737=VERTEX_POINT('',#29043);
#1738=VERTEX_POINT('',#29123);
#1739=VERTEX_POINT('',#29170);
#1740=VERTEX_POINT('',#29172);
#1741=VERTEX_POINT('',#29320);
#1742=VERTEX_POINT('',#29321);
#1743=VERTEX_POINT('',#29323);
#1744=VERTEX_POINT('',#29391);
#1745=VERTEX_POINT('',#29410);
#1746=VERTEX_POINT('',#29501);
#1747=VERTEX_POINT('',#29502);
#1748=VERTEX_POINT('',#29504);
#1749=VERTEX_POINT('',#29720);
#1750=VERTEX_POINT('',#29854);
#1751=VERTEX_POINT('',#29855);
#1752=VERTEX_POINT('',#29857);
#1753=VERTEX_POINT('',#30204);
#1754=VERTEX_POINT('',#30205);
#1755=VERTEX_POINT('',#30207);
#1756=VERTEX_POINT('',#30275);
#1757=VERTEX_POINT('',#30402);
#1758=VERTEX_POINT('',#30621);
#1759=VERTEX_POINT('',#30785);
#1760=VERTEX_POINT('',#31004);
#1761=VERTEX_POINT('',#31350);
#1762=VERTEX_POINT('',#31862);
#1763=VERTEX_POINT('',#31863);
#1764=VERTEX_POINT('',#31865);
#1765=VERTEX_POINT('',#31867);
#1766=VERTEX_POINT('',#31869);
#1767=VERTEX_POINT('',#31871);
#1768=VERTEX_POINT('',#31875);
#1769=VERTEX_POINT('',#31877);
#1770=VERTEX_POINT('',#31881);
#1771=VERTEX_POINT('',#31885);
#1772=VERTEX_POINT('',#31889);
#1773=VERTEX_POINT('',#31893);
#1774=VERTEX_POINT('',#31901);
#1775=VERTEX_POINT('',#31902);
#1776=VERTEX_POINT('',#31904);
#1777=VERTEX_POINT('',#32014);
#1778=VERTEX_POINT('',#32093);
#1779=VERTEX_POINT('',#32094);
#1780=VERTEX_POINT('',#32096);
#1781=VERTEX_POINT('',#32525);
#1782=VERTEX_POINT('',#32526);
#1783=VERTEX_POINT('',#32744);
#1784=VERTEX_POINT('',#32994);
#1785=VERTEX_POINT('',#32995);
#1786=VERTEX_POINT('',#32997);
#1787=VERTEX_POINT('',#33437);
#1788=VERTEX_POINT('',#33438);
#1789=VERTEX_POINT('',#33658);
#1790=VERTEX_POINT('',#33896);
#1791=VERTEX_POINT('',#33897);
#1792=VERTEX_POINT('',#33899);
#1793=VERTEX_POINT('',#34347);
#1794=VERTEX_POINT('',#34348);
#1795=VERTEX_POINT('',#34566);
#1796=VERTEX_POINT('',#34782);
#1797=VERTEX_POINT('',#34783);
#1798=VERTEX_POINT('',#34785);
#1799=VERTEX_POINT('',#35229);
#1800=VERTEX_POINT('',#35230);
#1801=VERTEX_POINT('',#35452);
#1802=VERTEX_POINT('',#35664);
#1803=VERTEX_POINT('',#35665);
#1804=VERTEX_POINT('',#35667);
#1805=VERTEX_POINT('',#36107);
#1806=VERTEX_POINT('',#36108);
#1807=VERTEX_POINT('',#36320);
#1808=VERTEX_POINT('',#36548);
#1809=VERTEX_POINT('',#36549);
#1810=VERTEX_POINT('',#36551);
#1811=VERTEX_POINT('',#37011);
#1812=VERTEX_POINT('',#37012);
#1813=VERTEX_POINT('',#37222);
#1814=VERTEX_POINT('',#37482);
#1815=VERTEX_POINT('',#37483);
#1816=VERTEX_POINT('',#37485);
#1817=VERTEX_POINT('',#37925);
#1818=VERTEX_POINT('',#37926);
#1819=VERTEX_POINT('',#38140);
#1820=VERTEX_POINT('',#38368);
#1821=VERTEX_POINT('',#38369);
#1822=VERTEX_POINT('',#38371);
#1823=VERTEX_POINT('',#38835);
#1824=VERTEX_POINT('',#38836);
#1825=VERTEX_POINT('',#39060);
#1826=VERTEX_POINT('',#39296);
#1827=VERTEX_POINT('',#39297);
#1828=VERTEX_POINT('',#39299);
#1829=VERTEX_POINT('',#39735);
#1830=VERTEX_POINT('',#39736);
#1831=VERTEX_POINT('',#39958);
#1832=VERTEX_POINT('',#40179);
#1833=VERTEX_POINT('',#40180);
#1834=VERTEX_POINT('',#40182);
#1835=VERTEX_POINT('',#40392);
#1836=VERTEX_POINT('',#40618);
#1837=VERTEX_POINT('',#40619);
#1838=VERTEX_POINT('',#40693);
#1839=VERTEX_POINT('',#40695);
#1840=VERTEX_POINT('',#40701);
#1841=VERTEX_POINT('',#40931);
#1842=VERTEX_POINT('',#41158);
#1843=VERTEX_POINT('',#41388);
#1844=VERTEX_POINT('',#41615);
#1845=VERTEX_POINT('',#41842);
#1846=VERTEX_POINT('',#42069);
#1847=VERTEX_POINT('',#42296);
#1848=VERTEX_POINT('',#42526);
#1849=VERTEX_POINT('',#42753);
#1850=VERTEX_POINT('',#42980);
#1851=VERTEX_POINT('',#43207);
#1852=VERTEX_POINT('',#43434);
#1853=VERTEX_POINT('',#43661);
#1854=VERTEX_POINT('',#43891);
#1855=VERTEX_POINT('',#44121);
#1856=VERTEX_POINT('',#44348);
#1857=VERTEX_POINT('',#44575);
#1858=VERTEX_POINT('',#44802);
#1859=VERTEX_POINT('',#45029);
#1860=VERTEX_POINT('',#45217);
#1861=VERTEX_POINT('',#45219);
#1862=VERTEX_POINT('',#45228);
#1863=VERTEX_POINT('',#45455);
#1864=VERTEX_POINT('',#45682);
#1865=VERTEX_POINT('',#45906);
#1866=VERTEX_POINT('',#46133);
#1867=VERTEX_POINT('',#46360);
#1868=VERTEX_POINT('',#46590);
#1869=VERTEX_POINT('',#46817);
#1870=VERTEX_POINT('',#47044);
#1871=VERTEX_POINT('',#47271);
#1872=VERTEX_POINT('',#47498);
#1873=VERTEX_POINT('',#47725);
#1874=VERTEX_POINT('',#47952);
#1875=VERTEX_POINT('',#48179);
#1876=VERTEX_POINT('',#48406);
#1877=VERTEX_POINT('',#48633);
#1878=VERTEX_POINT('',#48863);
#1879=VERTEX_POINT('',#49090);
#1880=VERTEX_POINT('',#49544);
#1881=VERTEX_POINT('',#49707);
#1882=VERTEX_POINT('',#49709);
#1883=VERTEX_POINT('',#51053);
#1884=VERTEX_POINT('',#51253);
#1885=VERTEX_POINT('',#51254);
#1886=VERTEX_POINT('',#51256);
#1887=VERTEX_POINT('',#51258);
#1888=VERTEX_POINT('',#51260);
#1889=VERTEX_POINT('',#51262);
#1890=VERTEX_POINT('',#51264);
#1891=VERTEX_POINT('',#51271);
#1892=VERTEX_POINT('',#51273);
#1893=VERTEX_POINT('',#51275);
#1894=VERTEX_POINT('',#51277);
#1895=VERTEX_POINT('',#51281);
#1896=VERTEX_POINT('',#51283);
#1897=VERTEX_POINT('',#51285);
#1898=VERTEX_POINT('',#51287);
#1899=VERTEX_POINT('',#51289);
#1900=VERTEX_POINT('',#51291);
#1901=VERTEX_POINT('',#51293);
#1902=VERTEX_POINT('',#51296);
#1903=VERTEX_POINT('',#51299);
#1904=VERTEX_POINT('',#51303);
#1905=VERTEX_POINT('',#51305);
#1906=VERTEX_POINT('',#51307);
#1907=VERTEX_POINT('',#51309);
#1908=VERTEX_POINT('',#51311);
#1909=VERTEX_POINT('',#51314);
#1910=VERTEX_POINT('',#51317);
#1911=VERTEX_POINT('',#51333);
#1912=VERTEX_POINT('',#51337);
#1913=VERTEX_POINT('',#51339);
#1914=VERTEX_POINT('',#51343);
#1915=VERTEX_POINT('',#51344);
#1916=VERTEX_POINT('',#51346);
#1917=VERTEX_POINT('',#51348);
#1918=VERTEX_POINT('',#51352);
#1919=VERTEX_POINT('',#51354);
#1920=VERTEX_POINT('',#51358);
#1921=VERTEX_POINT('',#51360);
#1922=VERTEX_POINT('',#51364);
#1923=VERTEX_POINT('',#51366);
#1924=VERTEX_POINT('',#51370);
#1925=VERTEX_POINT('',#51372);
#1926=VERTEX_POINT('',#51376);
#1927=VERTEX_POINT('',#51378);
#1928=VERTEX_POINT('',#51382);
#1929=VERTEX_POINT('',#51384);
#1930=VERTEX_POINT('',#51391);
#1931=VERTEX_POINT('',#51392);
#1932=VERTEX_POINT('',#51394);
#1933=VERTEX_POINT('',#51396);
#1934=VERTEX_POINT('',#51403);
#1935=VERTEX_POINT('',#51405);
#1936=VERTEX_POINT('',#51409);
#1937=VERTEX_POINT('',#51411);
#1938=VERTEX_POINT('',#51415);
#1939=VERTEX_POINT('',#51417);
#1940=VERTEX_POINT('',#51421);
#1941=VERTEX_POINT('',#51423);
#1942=VERTEX_POINT('',#51427);
#1943=VERTEX_POINT('',#51429);
#1944=VERTEX_POINT('',#51433);
#1945=VERTEX_POINT('',#51435);
#1946=VERTEX_POINT('',#51439);
#1947=VERTEX_POINT('',#51441);
#1948=VERTEX_POINT('',#51451);
#1949=VERTEX_POINT('',#51452);
#1950=VERTEX_POINT('',#51454);
#1951=VERTEX_POINT('',#51456);
#1952=VERTEX_POINT('',#51458);
#1953=VERTEX_POINT('',#51462);
#1954=VERTEX_POINT('',#51465);
#1955=VERTEX_POINT('',#51485);
#1956=VERTEX_POINT('',#51488);
#1957=VERTEX_POINT('',#51492);
#1958=VERTEX_POINT('',#51494);
#1959=VERTEX_POINT('',#51498);
#1960=VERTEX_POINT('',#51501);
#1961=VERTEX_POINT('',#51503);
#1962=VERTEX_POINT('',#51507);
#1963=VERTEX_POINT('',#51508);
#1964=VERTEX_POINT('',#51511);
#1965=VERTEX_POINT('',#51513);
#1966=VERTEX_POINT('',#51516);
#1967=VERTEX_POINT('',#51520);
#1968=EDGE_CURVE('',#1482,#1483,#1167,.T.);
#1969=EDGE_CURVE('',#1484,#1482,#711,.T.);
#1970=EDGE_CURVE('',#1485,#1484,#593,.T.);
#1971=EDGE_CURVE('',#1486,#1485,#712,.T.);
#1972=EDGE_CURVE('',#1487,#1486,#594,.T.);
#1973=EDGE_CURVE('',#1488,#1487,#713,.T.);
#1974=EDGE_CURVE('',#1483,#1488,#595,.T.);
#1975=EDGE_CURVE('',#1489,#1484,#714,.T.);
#1976=EDGE_CURVE('',#1489,#1490,#715,.T.);
#1977=EDGE_CURVE('',#1490,#1491,#716,.T.);
#1978=EDGE_CURVE('',#1491,#1492,#596,.T.);
#1979=EDGE_CURVE('',#1485,#1492,#717,.T.);
#1980=EDGE_CURVE('',#1492,#1493,#718,.T.);
#1981=EDGE_CURVE('',#1493,#1494,#719,.T.);
#1982=EDGE_CURVE('',#1494,#1495,#597,.T.);
#1983=EDGE_CURVE('',#1496,#1495,#598,.T.);
#1984=EDGE_CURVE('',#1496,#1497,#599,.T.);
#1985=EDGE_CURVE('',#1497,#1498,#720,.T.);
#1986=EDGE_CURVE('',#1498,#1499,#600,.T.);
#1987=EDGE_CURVE('',#1486,#1499,#721,.F.);
#1988=EDGE_CURVE('',#1500,#1500,#601,.T.);
#1989=EDGE_CURVE('',#1499,#1501,#722,.T.);
#1990=EDGE_CURVE('',#1487,#1501,#723,.T.);
#1991=EDGE_CURVE('',#1501,#1502,#602,.T.);
#1992=EDGE_CURVE('',#1502,#1503,#724,.T.);
#1993=EDGE_CURVE('',#1503,#1504,#603,.T.);
#1994=EDGE_CURVE('',#1505,#1504,#604,.T.);
#1995=EDGE_CURVE('',#1505,#1506,#605,.T.);
#1996=EDGE_CURVE('',#1488,#1506,#725,.F.);
#1997=EDGE_CURVE('',#1507,#1507,#606,.T.);
#1998=EDGE_CURVE('',#1508,#1493,#607,.F.);
#1999=EDGE_CURVE('',#1508,#1491,#726,.T.);
#2000=EDGE_CURVE('',#1495,#1505,#727,.T.);
#2001=EDGE_CURVE('',#1506,#1494,#728,.T.);
#2002=EDGE_CURVE('',#1504,#1496,#729,.T.);
#2003=EDGE_CURVE('',#1502,#1498,#730,.T.);
#2004=EDGE_CURVE('',#1497,#1503,#731,.T.);
#2005=EDGE_CURVE('',#1507,#1500,#732,.T.);
#2006=EDGE_CURVE('',#1508,#1509,#733,.T.);
#2007=EDGE_CURVE('',#1483,#1509,#734,.T.);
#2008=EDGE_CURVE('',#1510,#1510,#608,.T.);
#2009=EDGE_CURVE('',#1510,#1511,#735,.T.);
#2010=EDGE_CURVE('',#1511,#1511,#609,.T.);
#2011=EDGE_CURVE('',#1512,#1513,#736,.T.);
#2012=EDGE_CURVE('',#1512,#1514,#737,.T.);
#2013=EDGE_CURVE('',#1514,#1515,#738,.T.);
#2014=EDGE_CURVE('',#1513,#1515,#739,.T.);
#2015=EDGE_CURVE('',#1516,#1512,#610,.T.);
#2016=EDGE_CURVE('',#1516,#1517,#740,.T.);
#2017=EDGE_CURVE('',#1517,#1514,#611,.T.);
#2018=EDGE_CURVE('',#1518,#1516,#741,.T.);
#2019=EDGE_CURVE('',#1518,#1519,#742,.T.);
#2020=EDGE_CURVE('',#1519,#1517,#743,.T.);
#2021=EDGE_CURVE('',#1520,#1518,#612,.T.);
#2022=EDGE_CURVE('',#1520,#1521,#744,.T.);
#2023=EDGE_CURVE('',#1521,#1519,#613,.T.);
#2024=EDGE_CURVE('',#1522,#1520,#745,.T.);
#2025=EDGE_CURVE('',#1522,#1523,#746,.T.);
#2026=EDGE_CURVE('',#1523,#1521,#747,.T.);
#2027=EDGE_CURVE('',#1524,#1522,#614,.T.);
#2028=EDGE_CURVE('',#1524,#1525,#748,.T.);
#2029=EDGE_CURVE('',#1525,#1523,#615,.T.);
#2030=EDGE_CURVE('',#1526,#1524,#749,.T.);
#2031=EDGE_CURVE('',#1526,#1527,#750,.T.);
#2032=EDGE_CURVE('',#1527,#1525,#751,.T.);
#2033=EDGE_CURVE('',#1513,#1526,#616,.T.);
#2034=EDGE_CURVE('',#1515,#1527,#617,.T.);
#2035=EDGE_CURVE('',#1528,#1529,#618,.T.);
#2036=EDGE_CURVE('',#1528,#1530,#752,.T.);
#2037=EDGE_CURVE('',#1530,#1531,#619,.T.);
#2038=EDGE_CURVE('',#1529,#1531,#753,.T.);
#2039=EDGE_CURVE('',#1509,#1530,#620,.T.);
#2040=EDGE_CURVE('',#1528,#1482,#621,.T.);
#2041=EDGE_CURVE('',#1489,#1532,#622,.T.);
#2042=EDGE_CURVE('',#1532,#1533,#754,.T.);
#2043=EDGE_CURVE('',#1533,#1490,#623,.T.);
#2044=EDGE_CURVE('',#1534,#1532,#755,.T.);
#2045=EDGE_CURVE('',#1534,#1535,#756,.T.);
#2046=EDGE_CURVE('',#1535,#1533,#757,.T.);
#2047=EDGE_CURVE('',#1536,#1534,#624,.T.);
#2048=EDGE_CURVE('',#1536,#1537,#758,.T.);
#2049=EDGE_CURVE('',#1537,#1535,#625,.T.);
#2050=EDGE_CURVE('',#1538,#1536,#759,.T.);
#2051=EDGE_CURVE('',#1538,#1539,#760,.T.);
#2052=EDGE_CURVE('',#1539,#1537,#761,.T.);
#2053=EDGE_CURVE('',#1540,#1538,#626,.T.);
#2054=EDGE_CURVE('',#1540,#1541,#762,.T.);
#2055=EDGE_CURVE('',#1541,#1539,#627,.T.);
#2056=EDGE_CURVE('',#1542,#1540,#763,.T.);
#2057=EDGE_CURVE('',#1542,#1543,#764,.T.);
#2058=EDGE_CURVE('',#1543,#1541,#765,.T.);
#2059=EDGE_CURVE('',#1544,#1542,#628,.T.);
#2060=EDGE_CURVE('',#1544,#1545,#766,.T.);
#2061=EDGE_CURVE('',#1545,#1543,#629,.T.);
#2062=EDGE_CURVE('',#1529,#1544,#767,.T.);
#2063=EDGE_CURVE('',#1531,#1545,#768,.T.);
#2064=EDGE_CURVE('',#1546,#1547,#769,.T.);
#2065=EDGE_CURVE('',#1547,#1548,#1168,.T.);
#2066=EDGE_CURVE('',#1548,#1549,#630,.T.);
#2067=EDGE_CURVE('',#1546,#1549,#1169,.F.);
#2068=EDGE_CURVE('',#1550,#1551,#770,.T.);
#2069=EDGE_CURVE('',#1551,#1547,#1170,.T.);
#2070=EDGE_CURVE('',#1550,#1546,#1171,.F.);
#2071=EDGE_CURVE('',#1552,#1553,#771,.T.);
#2072=EDGE_CURVE('',#1553,#1551,#1172,.T.);
#2073=EDGE_CURVE('',#1552,#1550,#1173,.F.);
#2074=EDGE_CURVE('',#1554,#1555,#772,.T.);
#2075=EDGE_CURVE('',#1555,#1553,#1174,.T.);
#2076=EDGE_CURVE('',#1556,#1552,#1175,.F.);
#2077=EDGE_CURVE('',#1554,#1556,#1176,.F.);
#2078=EDGE_CURVE('',#1557,#1558,#773,.T.);
#2079=EDGE_CURVE('',#1558,#1559,#1177,.T.);
#2080=EDGE_CURVE('',#1559,#1555,#1178,.T.);
#2081=EDGE_CURVE('',#1557,#1554,#1179,.F.);
#2082=EDGE_CURVE('',#1560,#1561,#774,.T.);
#2083=EDGE_CURVE('',#1561,#1558,#1180,.T.);
#2084=EDGE_CURVE('',#1560,#1557,#1181,.F.);
#2085=EDGE_CURVE('',#1562,#1563,#775,.T.);
#2086=EDGE_CURVE('',#1563,#1561,#1182,.T.);
#2087=EDGE_CURVE('',#1564,#1560,#1183,.F.);
#2088=EDGE_CURVE('',#1562,#1564,#1184,.F.);
#2089=EDGE_CURVE('',#1565,#1566,#776,.T.);
#2090=EDGE_CURVE('',#1566,#1567,#1185,.T.);
#2091=EDGE_CURVE('',#1567,#1563,#1186,.T.);
#2092=EDGE_CURVE('',#1568,#1562,#1187,.F.);
#2093=EDGE_CURVE('',#1565,#1568,#1188,.F.);
#2094=EDGE_CURVE('',#1569,#1570,#777,.T.);
#2095=EDGE_CURVE('',#1570,#1571,#1189,.T.);
#2096=EDGE_CURVE('',#1571,#1566,#1190,.T.);
#2097=EDGE_CURVE('',#1569,#1565,#1191,.F.);
#2098=EDGE_CURVE('',#1572,#1573,#778,.T.);
#2099=EDGE_CURVE('',#1573,#1570,#1192,.T.);
#2100=EDGE_CURVE('',#1572,#1569,#1193,.F.);
#2101=EDGE_CURVE('',#1574,#1575,#779,.T.);
#2102=EDGE_CURVE('',#1575,#1573,#1194,.T.);
#2103=EDGE_CURVE('',#1576,#1572,#1195,.F.);
#2104=EDGE_CURVE('',#1574,#1576,#1196,.F.);
#2105=EDGE_CURVE('',#1577,#1578,#780,.T.);
#2106=EDGE_CURVE('',#1578,#1579,#1197,.T.);
#2107=EDGE_CURVE('',#1579,#1575,#1198,.T.);
#2108=EDGE_CURVE('',#1577,#1574,#1199,.F.);
#2109=EDGE_CURVE('',#1580,#1581,#781,.T.);
#2110=EDGE_CURVE('',#1581,#1578,#1200,.T.);
#2111=EDGE_CURVE('',#1580,#1577,#1201,.F.);
#2112=EDGE_CURVE('',#1582,#1583,#782,.T.);
#2113=EDGE_CURVE('',#1583,#1581,#1202,.T.);
#2114=EDGE_CURVE('',#1584,#1580,#1203,.F.);
#2115=EDGE_CURVE('',#1582,#1584,#1204,.F.);
#2116=EDGE_CURVE('',#1585,#1586,#783,.T.);
#2117=EDGE_CURVE('',#1586,#1587,#1205,.T.);
#2118=EDGE_CURVE('',#1587,#1583,#1206,.T.);
#2119=EDGE_CURVE('',#1585,#1582,#1207,.F.);
#2120=EDGE_CURVE('',#1588,#1589,#784,.T.);
#2121=EDGE_CURVE('',#1590,#1588,#1208,.F.);
#2122=EDGE_CURVE('',#1591,#1590,#1209,.F.);
#2123=EDGE_CURVE('',#1591,#1592,#1210,.T.);
#2124=EDGE_CURVE('',#1592,#1589,#1211,.T.);
#2125=EDGE_CURVE('',#1593,#1594,#1212,.T.);
#2126=EDGE_CURVE('',#1595,#1593,#631,.T.);
#2127=EDGE_CURVE('',#1596,#1595,#1213,.T.);
#2128=EDGE_CURVE('',#1597,#1596,#785,.T.);
#2129=EDGE_CURVE('',#1598,#1597,#1214,.T.);
#2130=EDGE_CURVE('',#1599,#1598,#786,.T.);
#2131=EDGE_CURVE('',#1600,#1599,#1215,.T.);
#2132=EDGE_CURVE('',#1601,#1600,#787,.T.);
#2133=EDGE_CURVE('',#1602,#1601,#1216,.T.);
#2134=EDGE_CURVE('',#1603,#1602,#788,.T.);
#2135=EDGE_CURVE('',#1604,#1603,#1217,.T.);
#2136=EDGE_CURVE('',#1605,#1604,#789,.T.);
#2137=EDGE_CURVE('',#1606,#1605,#1218,.T.);
#2138=EDGE_CURVE('',#1607,#1606,#790,.T.);
#2139=EDGE_CURVE('',#1608,#1607,#1219,.T.);
#2140=EDGE_CURVE('',#1609,#1608,#791,.T.);
#2141=EDGE_CURVE('',#1610,#1609,#1220,.T.);
#2142=EDGE_CURVE('',#1611,#1610,#792,.T.);
#2143=EDGE_CURVE('',#1612,#1611,#1221,.T.);
#2144=EDGE_CURVE('',#1613,#1612,#793,.T.);
#2145=EDGE_CURVE('',#1614,#1613,#1222,.T.);
#2146=EDGE_CURVE('',#1615,#1614,#794,.T.);
#2147=EDGE_CURVE('',#1616,#1615,#1223,.T.);
#2148=EDGE_CURVE('',#1617,#1616,#795,.T.);
#2149=EDGE_CURVE('',#1618,#1617,#1224,.T.);
#2150=EDGE_CURVE('',#1619,#1618,#796,.T.);
#2151=EDGE_CURVE('',#1620,#1619,#1225,.T.);
#2152=EDGE_CURVE('',#1594,#1620,#797,.T.);
#2153=EDGE_CURVE('',#1621,#1593,#1226,.T.);
#2154=EDGE_CURVE('',#1622,#1621,#1227,.T.);
#2155=EDGE_CURVE('',#1623,#1622,#1228,.T.);
#2156=EDGE_CURVE('',#1624,#1623,#1229,.T.);
#2157=EDGE_CURVE('',#1592,#1624,#1230,.T.);
#2158=EDGE_CURVE('',#1625,#1591,#1231,.T.);
#2159=EDGE_CURVE('',#1626,#1625,#1232,.T.);
#2160=EDGE_CURVE('',#1595,#1626,#1233,.T.);
#2161=EDGE_CURVE('',#1627,#1608,#1234,.T.);
#2162=EDGE_CURVE('',#1628,#1627,#1235,.T.);
#2163=EDGE_CURVE('',#1629,#1628,#632,.T.);
#2164=EDGE_CURVE('',#1630,#1629,#1236,.T.);
#2165=EDGE_CURVE('',#1631,#1630,#633,.F.);
#2166=EDGE_CURVE('',#1609,#1631,#1237,.T.);
#2167=EDGE_CURVE('',#1632,#1625,#1238,.T.);
#2168=EDGE_CURVE('',#1633,#1632,#1239,.T.);
#2169=EDGE_CURVE('',#1634,#1633,#1240,.T.);
#2170=EDGE_CURVE('',#1635,#1634,#1241,.T.);
#2171=EDGE_CURVE('',#1636,#1635,#1242,.T.);
#2172=EDGE_CURVE('',#1637,#1636,#1243,.T.);
#2173=EDGE_CURVE('',#1638,#1637,#1244,.T.);
#2174=EDGE_CURVE('',#1639,#1638,#1245,.T.);
#2175=EDGE_CURVE('',#1640,#1639,#1246,.T.);
#2176=EDGE_CURVE('',#1641,#1640,#1247,.T.);
#2177=EDGE_CURVE('',#1642,#1641,#1248,.T.);
#2178=EDGE_CURVE('',#1643,#1642,#1249,.T.);
#2179=EDGE_CURVE('',#1644,#1643,#1250,.T.);
#2180=EDGE_CURVE('',#1645,#1644,#1251,.T.);
#2181=EDGE_CURVE('',#1646,#1645,#1252,.T.);
#2182=EDGE_CURVE('',#1647,#1646,#1253,.T.);
#2183=EDGE_CURVE('',#1648,#1647,#1254,.T.);
#2184=EDGE_CURVE('',#1648,#1649,#634,.T.);
#2185=EDGE_CURVE('',#1650,#1649,#1255,.T.);
#2186=EDGE_CURVE('',#1651,#1650,#1256,.T.);
#2187=EDGE_CURVE('',#1652,#1651,#1257,.T.);
#2188=EDGE_CURVE('',#1653,#1652,#1258,.T.);
#2189=EDGE_CURVE('',#1654,#1653,#1259,.T.);
#2190=EDGE_CURVE('',#1655,#1654,#1260,.T.);
#2191=EDGE_CURVE('',#1656,#1655,#1261,.T.);
#2192=EDGE_CURVE('',#1657,#1656,#1262,.T.);
#2193=EDGE_CURVE('',#1658,#1657,#1263,.T.);
#2194=EDGE_CURVE('',#1659,#1658,#1264,.T.);
#2195=EDGE_CURVE('',#1660,#1659,#1265,.T.);
#2196=EDGE_CURVE('',#1661,#1660,#1266,.T.);
#2197=EDGE_CURVE('',#1662,#1661,#1267,.T.);
#2198=EDGE_CURVE('',#1663,#1662,#1268,.T.);
#2199=EDGE_CURVE('',#1664,#1663,#1269,.T.);
#2200=EDGE_CURVE('',#1665,#1664,#1270,.T.);
#2201=EDGE_CURVE('',#1626,#1665,#1271,.T.);
#2202=EDGE_CURVE('',#1622,#1598,#1272,.T.);
#2203=EDGE_CURVE('',#1599,#1621,#1273,.T.);
#2204=EDGE_CURVE('',#1619,#1602,#1274,.T.);
#2205=EDGE_CURVE('',#1603,#1618,#1275,.T.);
#2206=EDGE_CURVE('',#1615,#1606,#1276,.T.);
#2207=EDGE_CURVE('',#1607,#1614,#1277,.T.);
#2208=EDGE_CURVE('',#1588,#1585,#1278,.F.);
#2209=EDGE_CURVE('',#1549,#1666,#1279,.T.);
#2210=EDGE_CURVE('',#1666,#1648,#1280,.T.);
#2211=EDGE_CURVE('',#1597,#1623,#1281,.F.);
#2212=EDGE_CURVE('',#1601,#1620,#1282,.F.);
#2213=EDGE_CURVE('',#1605,#1616,#1283,.F.);
#2214=EDGE_CURVE('',#1589,#1586,#1284,.T.);
#2215=EDGE_CURVE('',#1596,#1624,#1285,.T.);
#2216=EDGE_CURVE('',#1600,#1594,#1286,.T.);
#2217=EDGE_CURVE('',#1604,#1617,#1287,.T.);
#2218=EDGE_CURVE('',#1649,#1548,#1288,.T.);
#2219=EDGE_CURVE('',#1628,#1613,#1289,.T.);
#2220=EDGE_CURVE('',#1631,#1610,#1290,.T.);
#2221=EDGE_CURVE('',#1611,#1630,#1291,.T.);
#2222=EDGE_CURVE('',#1629,#1612,#1292,.T.);
#2223=EDGE_CURVE('',#1667,#1668,#798,.T.);
#2224=EDGE_CURVE('',#1669,#1667,#1293,.T.);
#2225=EDGE_CURVE('',#1669,#1670,#635,.T.);
#2226=EDGE_CURVE('',#1670,#1668,#1294,.T.);
#2227=EDGE_CURVE('',#1671,#1672,#799,.T.);
#2228=EDGE_CURVE('',#1673,#1671,#1295,.T.);
#2229=EDGE_CURVE('',#1667,#1673,#1296,.T.);
#2230=EDGE_CURVE('',#1668,#1674,#1297,.T.);
#2231=EDGE_CURVE('',#1674,#1672,#1298,.T.);
#2232=EDGE_CURVE('',#1675,#1676,#800,.T.);
#2233=EDGE_CURVE('',#1677,#1675,#1299,.T.);
#2234=EDGE_CURVE('',#1671,#1677,#1300,.T.);
#2235=EDGE_CURVE('',#1672,#1678,#1301,.T.);
#2236=EDGE_CURVE('',#1678,#1676,#1302,.T.);
#2237=EDGE_CURVE('',#1679,#1680,#801,.T.);
#2238=EDGE_CURVE('',#1681,#1679,#1303,.T.);
#2239=EDGE_CURVE('',#1675,#1681,#1304,.T.);
#2240=EDGE_CURVE('',#1676,#1682,#1305,.T.);
#2241=EDGE_CURVE('',#1682,#1680,#1306,.T.);
#2242=EDGE_CURVE('',#1683,#1684,#802,.T.);
#2243=EDGE_CURVE('',#1685,#1683,#1307,.T.);
#2244=EDGE_CURVE('',#1686,#1685,#1308,.T.);
#2245=EDGE_CURVE('',#1686,#1687,#636,.F.);
#2246=EDGE_CURVE('',#1684,#1687,#1309,.F.);
#2247=EDGE_CURVE('',#1688,#1689,#803,.T.);
#2248=EDGE_CURVE('',#1690,#1688,#1310,.T.);
#2249=EDGE_CURVE('',#1683,#1690,#1311,.T.);
#2250=EDGE_CURVE('',#1689,#1684,#1312,.F.);
#2251=EDGE_CURVE('',#1691,#1692,#804,.T.);
#2252=EDGE_CURVE('',#1693,#1691,#1313,.T.);
#2253=EDGE_CURVE('',#1688,#1693,#1314,.T.);
#2254=EDGE_CURVE('',#1692,#1689,#1315,.F.);
#2255=EDGE_CURVE('',#1694,#1695,#805,.T.);
#2256=EDGE_CURVE('',#1696,#1694,#1316,.T.);
#2257=EDGE_CURVE('',#1691,#1696,#1317,.T.);
#2258=EDGE_CURVE('',#1695,#1692,#1318,.F.);
#2259=EDGE_CURVE('',#1697,#1695,#1319,.F.);
#2260=EDGE_CURVE('',#1697,#1698,#637,.T.);
#2261=EDGE_CURVE('',#1694,#1698,#1320,.T.);
#2262=EDGE_CURVE('',#1680,#1699,#1321,.T.);
#2263=EDGE_CURVE('',#1699,#1700,#1322,.T.);
#2264=EDGE_CURVE('',#1700,#1701,#638,.T.);
#2265=EDGE_CURVE('',#1702,#1701,#1323,.T.);
#2266=EDGE_CURVE('',#1679,#1702,#1324,.T.);
#2267=EDGE_CURVE('',#1701,#1703,#1325,.T.);
#2268=EDGE_CURVE('',#1703,#1697,#1326,.T.);
#2269=EDGE_CURVE('',#1687,#1669,#1327,.T.);
#2270=EDGE_CURVE('',#1698,#1700,#1328,.T.);
#2271=EDGE_CURVE('',#1670,#1686,#1329,.T.);
#2272=EDGE_CURVE('',#1704,#1705,#806,.T.);
#2273=EDGE_CURVE('',#1706,#1704,#807,.T.);
#2274=EDGE_CURVE('',#1707,#1706,#808,.T.);
#2275=EDGE_CURVE('',#1708,#1707,#809,.T.);
#2276=EDGE_CURVE('',#1709,#1708,#810,.T.);
#2277=EDGE_CURVE('',#1705,#1709,#811,.T.);
#2278=EDGE_CURVE('',#1709,#1710,#812,.T.);
#2279=EDGE_CURVE('',#1710,#1711,#813,.T.);
#2280=EDGE_CURVE('',#1705,#1711,#814,.T.);
#2281=EDGE_CURVE('',#1708,#1712,#815,.T.);
#2282=EDGE_CURVE('',#1712,#1710,#816,.T.);
#2283=EDGE_CURVE('',#1707,#1713,#817,.T.);
#2284=EDGE_CURVE('',#1713,#1712,#818,.T.);
#2285=EDGE_CURVE('',#1706,#1714,#819,.T.);
#2286=EDGE_CURVE('',#1714,#1713,#820,.T.);
#2287=EDGE_CURVE('',#1704,#1715,#821,.T.);
#2288=EDGE_CURVE('',#1715,#1714,#822,.T.);
#2289=EDGE_CURVE('',#1711,#1715,#823,.T.);
#2290=EDGE_CURVE('',#1716,#1716,#639,.T.);
#2291=EDGE_CURVE('',#1716,#1717,#824,.T.);
#2292=EDGE_CURVE('',#1717,#1717,#640,.T.);
#2293=EDGE_CURVE('',#1718,#1718,#641,.T.);
#2294=EDGE_CURVE('',#1718,#1719,#825,.T.);
#2295=EDGE_CURVE('',#1719,#1719,#642,.T.);
#2296=EDGE_CURVE('',#1720,#1720,#643,.T.);
#2297=EDGE_CURVE('',#1720,#1718,#644,.T.);
#2298=EDGE_CURVE('',#1721,#1721,#645,.T.);
#2299=EDGE_CURVE('',#1722,#1722,#646,.T.);
#2300=EDGE_CURVE('',#1722,#1721,#647,.T.);
#2301=EDGE_CURVE('',#1719,#1722,#648,.T.);
#2302=EDGE_CURVE('',#1723,#1724,#826,.T.);
#2303=EDGE_CURVE('',#1724,#1725,#1330,.T.);
#2304=EDGE_CURVE('',#1726,#1725,#649,.T.);
#2305=EDGE_CURVE('',#1723,#1726,#1331,.T.);
#2306=EDGE_CURVE('',#1727,#1728,#827,.T.);
#2307=EDGE_CURVE('',#1728,#1729,#1332,.T.);
#2308=EDGE_CURVE('',#1729,#1724,#1333,.T.);
#2309=EDGE_CURVE('',#1730,#1723,#1334,.T.);
#2310=EDGE_CURVE('',#1727,#1730,#1335,.T.);
#2311=EDGE_CURVE('',#1731,#1732,#828,.T.);
#2312=EDGE_CURVE('',#1732,#1733,#1336,.T.);
#2313=EDGE_CURVE('',#1733,#1728,#1337,.T.);
#2314=EDGE_CURVE('',#1734,#1727,#1338,.T.);
#2315=EDGE_CURVE('',#1731,#1734,#1339,.T.);
#2316=EDGE_CURVE('',#1735,#1736,#829,.T.);
#2317=EDGE_CURVE('',#1737,#1735,#1340,.T.);
#2318=EDGE_CURVE('',#1738,#1737,#1341,.T.);
#2319=EDGE_CURVE('',#1739,#1738,#650,.T.);
#2320=EDGE_CURVE('',#1739,#1740,#1342,.T.);
#2321=EDGE_CURVE('',#1740,#1736,#1343,.T.);
#2322=EDGE_CURVE('',#1741,#1742,#830,.T.);
#2323=EDGE_CURVE('',#1742,#1743,#1344,.T.);
#2324=EDGE_CURVE('',#1743,#1744,#1345,.T.);
#2325=EDGE_CURVE('',#1745,#1744,#651,.T.);
#2326=EDGE_CURVE('',#1745,#1741,#1346,.T.);
#2327=EDGE_CURVE('',#1746,#1747,#831,.T.);
#2328=EDGE_CURVE('',#1747,#1748,#1347,.T.);
#2329=EDGE_CURVE('',#1748,#1742,#1348,.T.);
#2330=EDGE_CURVE('',#1741,#1749,#1349,.T.);
#2331=EDGE_CURVE('',#1749,#1746,#1350,.T.);
#2332=EDGE_CURVE('',#1750,#1751,#832,.T.);
#2333=EDGE_CURVE('',#1751,#1752,#1351,.T.);
#2334=EDGE_CURVE('',#1752,#1747,#1352,.T.);
#2335=EDGE_CURVE('',#1746,#1750,#1353,.T.);
#2336=EDGE_CURVE('',#1753,#1754,#833,.T.);
#2337=EDGE_CURVE('',#1753,#1755,#1354,.T.);
#2338=EDGE_CURVE('',#1756,#1755,#652,.F.);
#2339=EDGE_CURVE('',#1756,#1754,#1355,.T.);
#2340=EDGE_CURVE('',#1754,#1757,#1356,.T.);
#2341=EDGE_CURVE('',#1757,#1751,#1357,.T.);
#2342=EDGE_CURVE('',#1750,#1758,#1358,.T.);
#2343=EDGE_CURVE('',#1758,#1753,#1359,.T.);
#2344=EDGE_CURVE('',#1736,#1759,#1360,.T.);
#2345=EDGE_CURVE('',#1759,#1732,#1361,.T.);
#2346=EDGE_CURVE('',#1760,#1731,#1362,.T.);
#2347=EDGE_CURVE('',#1735,#1760,#1363,.T.);
#2348=EDGE_CURVE('',#1725,#1761,#1364,.T.);
#2349=EDGE_CURVE('',#1755,#1739,#1365,.T.);
#2350=EDGE_CURVE('',#1761,#1745,#1366,.T.);
#2351=EDGE_CURVE('',#1744,#1726,#1367,.T.);
#2352=EDGE_CURVE('',#1738,#1756,#1368,.T.);
#2353=EDGE_CURVE('',#1762,#1763,#834,.T.);
#2354=EDGE_CURVE('',#1763,#1764,#835,.T.);
#2355=EDGE_CURVE('',#1764,#1765,#836,.T.);
#2356=EDGE_CURVE('',#1765,#1766,#837,.T.);
#2357=EDGE_CURVE('',#1766,#1767,#838,.T.);
#2358=EDGE_CURVE('',#1767,#1762,#839,.T.);
#2359=EDGE_CURVE('',#1763,#1768,#840,.T.);
#2360=EDGE_CURVE('',#1769,#1768,#841,.T.);
#2361=EDGE_CURVE('',#1764,#1769,#842,.T.);
#2362=EDGE_CURVE('',#1770,#1769,#843,.T.);
#2363=EDGE_CURVE('',#1765,#1770,#844,.T.);
#2364=EDGE_CURVE('',#1771,#1770,#845,.T.);
#2365=EDGE_CURVE('',#1766,#1771,#846,.T.);
#2366=EDGE_CURVE('',#1772,#1771,#847,.T.);
#2367=EDGE_CURVE('',#1767,#1772,#848,.T.);
#2368=EDGE_CURVE('',#1773,#1772,#849,.T.);
#2369=EDGE_CURVE('',#1762,#1773,#850,.T.);
#2370=EDGE_CURVE('',#1768,#1773,#851,.T.);
#2371=EDGE_CURVE('',#1774,#1775,#852,.T.);
#2372=EDGE_CURVE('',#1776,#1774,#1369,.T.);
#2373=EDGE_CURVE('',#1777,#1776,#653,.T.);
#2374=EDGE_CURVE('',#1777,#1775,#1370,.T.);
#2375=EDGE_CURVE('',#1778,#1779,#853,.T.);
#2376=EDGE_CURVE('',#1780,#1778,#1371,.F.);
#2377=EDGE_CURVE('',#1774,#1780,#1372,.T.);
#2378=EDGE_CURVE('',#1775,#1779,#1373,.T.);
#2379=EDGE_CURVE('',#1781,#1782,#854,.T.);
#2380=EDGE_CURVE('',#1778,#1781,#1374,.F.);
#2381=EDGE_CURVE('',#1779,#1783,#1375,.T.);
#2382=EDGE_CURVE('',#1783,#1782,#1376,.T.);
#2383=EDGE_CURVE('',#1784,#1785,#855,.T.);
#2384=EDGE_CURVE('',#1786,#1784,#1377,.F.);
#2385=EDGE_CURVE('',#1781,#1786,#1378,.F.);
#2386=EDGE_CURVE('',#1782,#1785,#1379,.T.);
#2387=EDGE_CURVE('',#1787,#1788,#856,.T.);
#2388=EDGE_CURVE('',#1784,#1787,#1380,.F.);
#2389=EDGE_CURVE('',#1785,#1789,#1381,.T.);
#2390=EDGE_CURVE('',#1789,#1788,#1382,.T.);
#2391=EDGE_CURVE('',#1790,#1791,#857,.T.);
#2392=EDGE_CURVE('',#1792,#1790,#1383,.F.);
#2393=EDGE_CURVE('',#1787,#1792,#1384,.F.);
#2394=EDGE_CURVE('',#1788,#1791,#1385,.T.);
#2395=EDGE_CURVE('',#1793,#1794,#858,.T.);
#2396=EDGE_CURVE('',#1790,#1793,#1386,.F.);
#2397=EDGE_CURVE('',#1791,#1795,#1387,.T.);
#2398=EDGE_CURVE('',#1795,#1794,#1388,.T.);
#2399=EDGE_CURVE('',#1796,#1797,#859,.T.);
#2400=EDGE_CURVE('',#1798,#1796,#1389,.F.);
#2401=EDGE_CURVE('',#1793,#1798,#1390,.F.);
#2402=EDGE_CURVE('',#1794,#1797,#1391,.T.);
#2403=EDGE_CURVE('',#1799,#1800,#860,.T.);
#2404=EDGE_CURVE('',#1796,#1799,#1392,.F.);
#2405=EDGE_CURVE('',#1797,#1801,#1393,.T.);
#2406=EDGE_CURVE('',#1801,#1800,#1394,.T.);
#2407=EDGE_CURVE('',#1802,#1803,#861,.T.);
#2408=EDGE_CURVE('',#1804,#1802,#1395,.F.);
#2409=EDGE_CURVE('',#1799,#1804,#1396,.F.);
#2410=EDGE_CURVE('',#1800,#1803,#1397,.T.);
#2411=EDGE_CURVE('',#1805,#1806,#862,.T.);
#2412=EDGE_CURVE('',#1802,#1805,#1398,.F.);
#2413=EDGE_CURVE('',#1803,#1807,#1399,.T.);
#2414=EDGE_CURVE('',#1807,#1806,#1400,.T.);
#2415=EDGE_CURVE('',#1808,#1809,#863,.T.);
#2416=EDGE_CURVE('',#1810,#1808,#1401,.F.);
#2417=EDGE_CURVE('',#1805,#1810,#1402,.F.);
#2418=EDGE_CURVE('',#1806,#1809,#1403,.T.);
#2419=EDGE_CURVE('',#1811,#1812,#864,.T.);
#2420=EDGE_CURVE('',#1808,#1811,#1404,.F.);
#2421=EDGE_CURVE('',#1809,#1813,#1405,.T.);
#2422=EDGE_CURVE('',#1813,#1812,#1406,.T.);
#2423=EDGE_CURVE('',#1814,#1815,#865,.T.);
#2424=EDGE_CURVE('',#1816,#1814,#1407,.F.);
#2425=EDGE_CURVE('',#1811,#1816,#1408,.F.);
#2426=EDGE_CURVE('',#1812,#1815,#1409,.T.);
#2427=EDGE_CURVE('',#1817,#1818,#866,.T.);
#2428=EDGE_CURVE('',#1814,#1817,#1410,.F.);
#2429=EDGE_CURVE('',#1815,#1819,#1411,.T.);
#2430=EDGE_CURVE('',#1819,#1818,#1412,.T.);
#2431=EDGE_CURVE('',#1820,#1821,#867,.T.);
#2432=EDGE_CURVE('',#1822,#1820,#1413,.F.);
#2433=EDGE_CURVE('',#1817,#1822,#1414,.F.);
#2434=EDGE_CURVE('',#1818,#1821,#1415,.T.);
#2435=EDGE_CURVE('',#1823,#1824,#868,.T.);
#2436=EDGE_CURVE('',#1820,#1823,#1416,.F.);
#2437=EDGE_CURVE('',#1821,#1825,#1417,.T.);
#2438=EDGE_CURVE('',#1825,#1824,#1418,.T.);
#2439=EDGE_CURVE('',#1826,#1827,#869,.T.);
#2440=EDGE_CURVE('',#1828,#1826,#1419,.F.);
#2441=EDGE_CURVE('',#1823,#1828,#1420,.F.);
#2442=EDGE_CURVE('',#1824,#1827,#1421,.T.);
#2443=EDGE_CURVE('',#1829,#1830,#870,.T.);
#2444=EDGE_CURVE('',#1826,#1829,#1422,.F.);
#2445=EDGE_CURVE('',#1827,#1831,#1423,.T.);
#2446=EDGE_CURVE('',#1831,#1830,#1424,.T.);
#2447=EDGE_CURVE('',#1832,#1833,#871,.T.);
#2448=EDGE_CURVE('',#1834,#1832,#1425,.T.);
#2449=EDGE_CURVE('',#1829,#1834,#1426,.F.);
#2450=EDGE_CURVE('',#1830,#1835,#1427,.T.);
#2451=EDGE_CURVE('',#1835,#1833,#1428,.F.);
#2452=EDGE_CURVE('',#1836,#1837,#1429,.T.);
#2453=EDGE_CURVE('',#1838,#1837,#654,.F.);
#2454=EDGE_CURVE('',#1838,#1839,#1430,.T.);
#2455=EDGE_CURVE('',#1839,#1840,#1431,.T.);
#2456=EDGE_CURVE('',#1840,#1841,#1432,.T.);
#2457=EDGE_CURVE('',#1841,#1842,#1433,.T.);
#2458=EDGE_CURVE('',#1842,#1843,#1434,.T.);
#2459=EDGE_CURVE('',#1843,#1844,#1435,.T.);
#2460=EDGE_CURVE('',#1844,#1845,#1436,.T.);
#2461=EDGE_CURVE('',#1845,#1846,#1437,.T.);
#2462=EDGE_CURVE('',#1846,#1847,#1438,.T.);
#2463=EDGE_CURVE('',#1847,#1848,#1439,.T.);
#2464=EDGE_CURVE('',#1848,#1849,#1440,.T.);
#2465=EDGE_CURVE('',#1849,#1850,#1441,.T.);
#2466=EDGE_CURVE('',#1850,#1851,#1442,.T.);
#2467=EDGE_CURVE('',#1851,#1852,#1443,.T.);
#2468=EDGE_CURVE('',#1852,#1853,#1444,.T.);
#2469=EDGE_CURVE('',#1853,#1854,#1445,.T.);
#2470=EDGE_CURVE('',#1854,#1855,#1446,.T.);
#2471=EDGE_CURVE('',#1855,#1856,#1447,.T.);
#2472=EDGE_CURVE('',#1856,#1857,#1448,.T.);
#2473=EDGE_CURVE('',#1857,#1858,#1449,.T.);
#2474=EDGE_CURVE('',#1858,#1859,#1450,.T.);
#2475=EDGE_CURVE('',#1860,#1859,#655,.T.);
#2476=EDGE_CURVE('',#1860,#1861,#1451,.T.);
#2477=EDGE_CURVE('',#1861,#1862,#1452,.T.);
#2478=EDGE_CURVE('',#1862,#1863,#1453,.T.);
#2479=EDGE_CURVE('',#1863,#1864,#1454,.T.);
#2480=EDGE_CURVE('',#1864,#1865,#1455,.T.);
#2481=EDGE_CURVE('',#1865,#1866,#1456,.T.);
#2482=EDGE_CURVE('',#1866,#1867,#1457,.T.);
#2483=EDGE_CURVE('',#1867,#1868,#1458,.T.);
#2484=EDGE_CURVE('',#1868,#1869,#1459,.T.);
#2485=EDGE_CURVE('',#1869,#1870,#1460,.T.);
#2486=EDGE_CURVE('',#1870,#1871,#1461,.T.);
#2487=EDGE_CURVE('',#1871,#1872,#1462,.T.);
#2488=EDGE_CURVE('',#1872,#1873,#1463,.T.);
#2489=EDGE_CURVE('',#1873,#1874,#1464,.T.);
#2490=EDGE_CURVE('',#1874,#1875,#1465,.T.);
#2491=EDGE_CURVE('',#1875,#1876,#1466,.T.);
#2492=EDGE_CURVE('',#1876,#1877,#1467,.T.);
#2493=EDGE_CURVE('',#1877,#1878,#1468,.T.);
#2494=EDGE_CURVE('',#1878,#1879,#1469,.T.);
#2495=EDGE_CURVE('',#1879,#1836,#1470,.T.);
#2496=EDGE_CURVE('',#1833,#1880,#1471,.F.);
#2497=EDGE_CURVE('',#1881,#1880,#656,.T.);
#2498=EDGE_CURVE('',#1882,#1881,#1472,.T.);
#2499=EDGE_CURVE('',#1832,#1882,#1473,.T.);
#2500=EDGE_CURVE('',#1859,#1881,#1474,.T.);
#2501=EDGE_CURVE('',#1776,#1838,#1475,.T.);
#2502=EDGE_CURVE('',#1883,#1860,#1476,.T.);
#2503=EDGE_CURVE('',#1880,#1883,#1477,.T.);
#2504=EDGE_CURVE('',#1837,#1777,#1478,.T.);
#2505=EDGE_CURVE('',#1884,#1885,#657,.T.);
#2506=EDGE_CURVE('',#1885,#1886,#872,.T.);
#2507=EDGE_CURVE('',#1886,#1887,#658,.T.);
#2508=EDGE_CURVE('',#1887,#1888,#873,.T.);
#2509=EDGE_CURVE('',#1888,#1889,#659,.T.);
#2510=EDGE_CURVE('',#1889,#1890,#874,.T.);
#2511=EDGE_CURVE('',#1890,#1884,#1479,.T.);
#2512=EDGE_CURVE('',#1888,#1891,#875,.T.);
#2513=EDGE_CURVE('',#1892,#1891,#660,.T.);
#2514=EDGE_CURVE('',#1893,#1892,#876,.T.);
#2515=EDGE_CURVE('',#1894,#1893,#877,.T.);
#2516=EDGE_CURVE('',#1894,#1889,#878,.T.);
#2517=EDGE_CURVE('',#1887,#1895,#879,.F.);
#2518=EDGE_CURVE('',#1896,#1895,#661,.T.);
#2519=EDGE_CURVE('',#1897,#1896,#880,.T.);
#2520=EDGE_CURVE('',#1898,#1897,#662,.T.);
#2521=EDGE_CURVE('',#1898,#1899,#663,.T.);
#2522=EDGE_CURVE('',#1900,#1899,#664,.T.);
#2523=EDGE_CURVE('',#1901,#1900,#881,.T.);
#2524=EDGE_CURVE('',#1891,#1901,#882,.T.);
#2525=EDGE_CURVE('',#1902,#1902,#665,.T.);
#2526=EDGE_CURVE('',#1886,#1903,#883,.T.);
#2527=EDGE_CURVE('',#1895,#1903,#884,.T.);
#2528=EDGE_CURVE('',#1885,#1904,#885,.F.);
#2529=EDGE_CURVE('',#1905,#1904,#666,.T.);
#2530=EDGE_CURVE('',#1905,#1906,#667,.T.);
#2531=EDGE_CURVE('',#1907,#1906,#668,.T.);
#2532=EDGE_CURVE('',#1908,#1907,#886,.T.);
#2533=EDGE_CURVE('',#1903,#1908,#669,.T.);
#2534=EDGE_CURVE('',#1909,#1909,#670,.T.);
#2535=EDGE_CURVE('',#1910,#1901,#671,.F.);
#2536=EDGE_CURVE('',#1910,#1892,#887,.T.);
#2537=EDGE_CURVE('',#1904,#1900,#888,.T.);
#2538=EDGE_CURVE('',#1899,#1905,#889,.T.);
#2539=EDGE_CURVE('',#1906,#1898,#890,.T.);
#2540=EDGE_CURVE('',#1908,#1896,#891,.T.);
#2541=EDGE_CURVE('',#1897,#1907,#892,.T.);
#2542=EDGE_CURVE('',#1902,#1909,#893,.T.);
#2543=EDGE_CURVE('',#1884,#1911,#894,.T.);
#2544=EDGE_CURVE('',#1910,#1911,#895,.T.);
#2545=EDGE_CURVE('',#1912,#1912,#672,.T.);
#2546=EDGE_CURVE('',#1912,#1913,#896,.T.);
#2547=EDGE_CURVE('',#1913,#1913,#673,.T.);
#2548=EDGE_CURVE('',#1914,#1915,#897,.T.);
#2549=EDGE_CURVE('',#1915,#1916,#898,.T.);
#2550=EDGE_CURVE('',#1917,#1916,#899,.T.);
#2551=EDGE_CURVE('',#1914,#1917,#900,.T.);
#2552=EDGE_CURVE('',#1918,#1914,#674,.T.);
#2553=EDGE_CURVE('',#1919,#1917,#675,.T.);
#2554=EDGE_CURVE('',#1918,#1919,#901,.T.);
#2555=EDGE_CURVE('',#1920,#1918,#902,.T.);
#2556=EDGE_CURVE('',#1921,#1919,#903,.T.);
#2557=EDGE_CURVE('',#1920,#1921,#904,.T.);
#2558=EDGE_CURVE('',#1922,#1920,#676,.T.);
#2559=EDGE_CURVE('',#1923,#1921,#677,.T.);
#2560=EDGE_CURVE('',#1922,#1923,#905,.T.);
#2561=EDGE_CURVE('',#1924,#1922,#906,.T.);
#2562=EDGE_CURVE('',#1925,#1923,#907,.T.);
#2563=EDGE_CURVE('',#1924,#1925,#908,.T.);
#2564=EDGE_CURVE('',#1926,#1924,#678,.T.);
#2565=EDGE_CURVE('',#1927,#1925,#679,.T.);
#2566=EDGE_CURVE('',#1926,#1927,#909,.T.);
#2567=EDGE_CURVE('',#1928,#1926,#910,.T.);
#2568=EDGE_CURVE('',#1929,#1927,#911,.T.);
#2569=EDGE_CURVE('',#1928,#1929,#912,.T.);
#2570=EDGE_CURVE('',#1915,#1928,#680,.T.);
#2571=EDGE_CURVE('',#1916,#1929,#681,.T.);
#2572=EDGE_CURVE('',#1930,#1931,#682,.T.);
#2573=EDGE_CURVE('',#1931,#1932,#913,.T.);
#2574=EDGE_CURVE('',#1933,#1932,#683,.T.);
#2575=EDGE_CURVE('',#1930,#1933,#914,.T.);
#2576=EDGE_CURVE('',#1930,#1890,#684,.T.);
#2577=EDGE_CURVE('',#1911,#1933,#685,.T.);
#2578=EDGE_CURVE('',#1894,#1934,#686,.T.);
#2579=EDGE_CURVE('',#1935,#1893,#687,.T.);
#2580=EDGE_CURVE('',#1934,#1935,#915,.T.);
#2581=EDGE_CURVE('',#1936,#1934,#916,.T.);
#2582=EDGE_CURVE('',#1937,#1935,#917,.T.);
#2583=EDGE_CURVE('',#1936,#1937,#918,.T.);
#2584=EDGE_CURVE('',#1938,#1936,#688,.T.);
#2585=EDGE_CURVE('',#1939,#1937,#689,.T.);
#2586=EDGE_CURVE('',#1938,#1939,#919,.T.);
#2587=EDGE_CURVE('',#1940,#1938,#920,.T.);
#2588=EDGE_CURVE('',#1941,#1939,#921,.T.);
#2589=EDGE_CURVE('',#1940,#1941,#922,.T.);
#2590=EDGE_CURVE('',#1942,#1940,#690,.T.);
#2591=EDGE_CURVE('',#1943,#1941,#691,.T.);
#2592=EDGE_CURVE('',#1942,#1943,#923,.T.);
#2593=EDGE_CURVE('',#1944,#1942,#924,.T.);
#2594=EDGE_CURVE('',#1945,#1943,#925,.T.);
#2595=EDGE_CURVE('',#1944,#1945,#926,.T.);
#2596=EDGE_CURVE('',#1946,#1944,#692,.T.);
#2597=EDGE_CURVE('',#1947,#1945,#693,.T.);
#2598=EDGE_CURVE('',#1946,#1947,#927,.T.);
#2599=EDGE_CURVE('',#1931,#1946,#928,.T.);
#2600=EDGE_CURVE('',#1932,#1947,#929,.T.);
#2601=EDGE_CURVE('',#1948,#1949,#930,.T.);
#2602=EDGE_CURVE('',#1950,#1948,#694,.T.);
#2603=EDGE_CURVE('',#1951,#1950,#695,.T.);
#2604=EDGE_CURVE('',#1952,#1951,#931,.T.);
#2605=EDGE_CURVE('',#1949,#1952,#932,.T.);
#2606=EDGE_CURVE('',#1953,#1953,#696,.T.);
#2607=EDGE_CURVE('',#1953,#1950,#933,.T.);
#2608=EDGE_CURVE('',#1954,#1948,#1480,.T.);
#2609=EDGE_CURVE('',#1951,#1954,#1481,.T.);
#2610=EDGE_CURVE('',#1952,#1949,#697,.T.);
#2611=EDGE_CURVE('',#1955,#1955,#698,.T.);
#2612=EDGE_CURVE('',#1956,#1956,#699,.T.);
#2613=EDGE_CURVE('',#1956,#1954,#934,.T.);
#2614=EDGE_CURVE('',#1955,#1957,#935,.T.);
#2615=EDGE_CURVE('',#1957,#1958,#700,.T.);
#2616=EDGE_CURVE('',#1958,#1957,#701,.T.);
#2617=EDGE_CURVE('',#1959,#1958,#702,.T.);
#2618=EDGE_CURVE('',#1960,#1960,#703,.T.);
#2619=EDGE_CURVE('',#1960,#1961,#936,.T.);
#2620=EDGE_CURVE('',#1961,#1961,#704,.T.);
#2621=EDGE_CURVE('',#1962,#1963,#705,.T.);
#2622=EDGE_CURVE('',#1963,#1962,#706,.T.);
#2623=EDGE_CURVE('',#1964,#1962,#707,.T.);
#2624=EDGE_CURVE('',#1965,#1965,#708,.T.);
#2625=EDGE_CURVE('',#1963,#1966,#937,.T.);
#2626=EDGE_CURVE('',#1966,#1966,#709,.T.);
#2627=EDGE_CURVE('',#1967,#1967,#710,.T.);
#2628=EDGE_CURVE('',#1967,#1965,#938,.T.);
#2629=ORIENTED_EDGE('',*,*,#1968,.F.);
#2630=ORIENTED_EDGE('',*,*,#1969,.F.);
#2631=ORIENTED_EDGE('',*,*,#1970,.F.);
#2632=ORIENTED_EDGE('',*,*,#1971,.F.);
#2633=ORIENTED_EDGE('',*,*,#1972,.F.);
#2634=ORIENTED_EDGE('',*,*,#1973,.F.);
#2635=ORIENTED_EDGE('',*,*,#1974,.F.);
#2636=ORIENTED_EDGE('',*,*,#1970,.T.);
#2637=ORIENTED_EDGE('',*,*,#1975,.F.);
#2638=ORIENTED_EDGE('',*,*,#1976,.T.);
#2639=ORIENTED_EDGE('',*,*,#1977,.T.);
#2640=ORIENTED_EDGE('',*,*,#1978,.T.);
#2641=ORIENTED_EDGE('',*,*,#1979,.F.);
#2642=ORIENTED_EDGE('',*,*,#1971,.T.);
#2643=ORIENTED_EDGE('',*,*,#1979,.T.);
#2644=ORIENTED_EDGE('',*,*,#1980,.T.);
#2645=ORIENTED_EDGE('',*,*,#1981,.T.);
#2646=ORIENTED_EDGE('',*,*,#1982,.T.);
#2647=ORIENTED_EDGE('',*,*,#1983,.F.);
#2648=ORIENTED_EDGE('',*,*,#1984,.T.);
#2649=ORIENTED_EDGE('',*,*,#1985,.T.);
#2650=ORIENTED_EDGE('',*,*,#1986,.T.);
#2651=ORIENTED_EDGE('',*,*,#1987,.F.);
#2652=ORIENTED_EDGE('',*,*,#1988,.F.);
#2653=ORIENTED_EDGE('',*,*,#1972,.T.);
#2654=ORIENTED_EDGE('',*,*,#1987,.T.);
#2655=ORIENTED_EDGE('',*,*,#1989,.T.);
#2656=ORIENTED_EDGE('',*,*,#1990,.F.);
#2657=ORIENTED_EDGE('',*,*,#1973,.T.);
#2658=ORIENTED_EDGE('',*,*,#1990,.T.);
#2659=ORIENTED_EDGE('',*,*,#1991,.T.);
#2660=ORIENTED_EDGE('',*,*,#1992,.T.);
#2661=ORIENTED_EDGE('',*,*,#1993,.T.);
#2662=ORIENTED_EDGE('',*,*,#1994,.F.);
#2663=ORIENTED_EDGE('',*,*,#1995,.T.);
#2664=ORIENTED_EDGE('',*,*,#1996,.F.);
#2665=ORIENTED_EDGE('',*,*,#1997,.F.);
#2666=ORIENTED_EDGE('',*,*,#1998,.T.);
#2667=ORIENTED_EDGE('',*,*,#1980,.F.);
#2668=ORIENTED_EDGE('',*,*,#1978,.F.);
#2669=ORIENTED_EDGE('',*,*,#1999,.F.);
#2670=ORIENTED_EDGE('',*,*,#1995,.F.);
#2671=ORIENTED_EDGE('',*,*,#2000,.F.);
#2672=ORIENTED_EDGE('',*,*,#1982,.F.);
#2673=ORIENTED_EDGE('',*,*,#2001,.F.);
#2674=ORIENTED_EDGE('',*,*,#2000,.T.);
#2675=ORIENTED_EDGE('',*,*,#1994,.T.);
#2676=ORIENTED_EDGE('',*,*,#2002,.T.);
#2677=ORIENTED_EDGE('',*,*,#1983,.T.);
#2678=ORIENTED_EDGE('',*,*,#1991,.F.);
#2679=ORIENTED_EDGE('',*,*,#1989,.F.);
#2680=ORIENTED_EDGE('',*,*,#1986,.F.);
#2681=ORIENTED_EDGE('',*,*,#2003,.F.);
#2682=ORIENTED_EDGE('',*,*,#2003,.T.);
#2683=ORIENTED_EDGE('',*,*,#1985,.F.);
#2684=ORIENTED_EDGE('',*,*,#2004,.T.);
#2685=ORIENTED_EDGE('',*,*,#1992,.F.);
#2686=ORIENTED_EDGE('',*,*,#1993,.F.);
#2687=ORIENTED_EDGE('',*,*,#2004,.F.);
#2688=ORIENTED_EDGE('',*,*,#1984,.F.);
#2689=ORIENTED_EDGE('',*,*,#2002,.F.);
#2690=ORIENTED_EDGE('',*,*,#1997,.T.);
#2691=ORIENTED_EDGE('',*,*,#2005,.T.);
#2692=ORIENTED_EDGE('',*,*,#1988,.T.);
#2693=ORIENTED_EDGE('',*,*,#2005,.F.);
#2694=ORIENTED_EDGE('',*,*,#1974,.T.);
#2695=ORIENTED_EDGE('',*,*,#1996,.T.);
#2696=ORIENTED_EDGE('',*,*,#2001,.T.);
#2697=ORIENTED_EDGE('',*,*,#1981,.F.);
#2698=ORIENTED_EDGE('',*,*,#1998,.F.);
#2699=ORIENTED_EDGE('',*,*,#2006,.T.);
#2700=ORIENTED_EDGE('',*,*,#2007,.F.);
#2701=ORIENTED_EDGE('',*,*,#2008,.T.);
#2702=ORIENTED_EDGE('',*,*,#2009,.T.);
#2703=ORIENTED_EDGE('',*,*,#2010,.F.);
#2704=ORIENTED_EDGE('',*,*,#2009,.F.);
#2705=ORIENTED_EDGE('',*,*,#2011,.F.);
#2706=ORIENTED_EDGE('',*,*,#2012,.T.);
#2707=ORIENTED_EDGE('',*,*,#2013,.T.);
#2708=ORIENTED_EDGE('',*,*,#2014,.F.);
#2709=ORIENTED_EDGE('',*,*,#2015,.F.);
#2710=ORIENTED_EDGE('',*,*,#2016,.T.);
#2711=ORIENTED_EDGE('',*,*,#2017,.T.);
#2712=ORIENTED_EDGE('',*,*,#2012,.F.);
#2713=ORIENTED_EDGE('',*,*,#2018,.F.);
#2714=ORIENTED_EDGE('',*,*,#2019,.T.);
#2715=ORIENTED_EDGE('',*,*,#2020,.T.);
#2716=ORIENTED_EDGE('',*,*,#2016,.F.);
#2717=ORIENTED_EDGE('',*,*,#2021,.F.);
#2718=ORIENTED_EDGE('',*,*,#2022,.T.);
#2719=ORIENTED_EDGE('',*,*,#2023,.T.);
#2720=ORIENTED_EDGE('',*,*,#2019,.F.);
#2721=ORIENTED_EDGE('',*,*,#2024,.F.);
#2722=ORIENTED_EDGE('',*,*,#2025,.T.);
#2723=ORIENTED_EDGE('',*,*,#2026,.T.);
#2724=ORIENTED_EDGE('',*,*,#2022,.F.);
#2725=ORIENTED_EDGE('',*,*,#2027,.F.);
#2726=ORIENTED_EDGE('',*,*,#2028,.T.);
#2727=ORIENTED_EDGE('',*,*,#2029,.T.);
#2728=ORIENTED_EDGE('',*,*,#2025,.F.);
#2729=ORIENTED_EDGE('',*,*,#2030,.F.);
#2730=ORIENTED_EDGE('',*,*,#2031,.T.);
#2731=ORIENTED_EDGE('',*,*,#2032,.T.);
#2732=ORIENTED_EDGE('',*,*,#2028,.F.);
#2733=ORIENTED_EDGE('',*,*,#2033,.F.);
#2734=ORIENTED_EDGE('',*,*,#2014,.T.);
#2735=ORIENTED_EDGE('',*,*,#2034,.T.);
#2736=ORIENTED_EDGE('',*,*,#2031,.F.);
#2737=ORIENTED_EDGE('',*,*,#2035,.F.);
#2738=ORIENTED_EDGE('',*,*,#2036,.T.);
#2739=ORIENTED_EDGE('',*,*,#2037,.T.);
#2740=ORIENTED_EDGE('',*,*,#2038,.F.);
#2741=ORIENTED_EDGE('',*,*,#1968,.T.);
#2742=ORIENTED_EDGE('',*,*,#2007,.T.);
#2743=ORIENTED_EDGE('',*,*,#2039,.T.);
#2744=ORIENTED_EDGE('',*,*,#2036,.F.);
#2745=ORIENTED_EDGE('',*,*,#2040,.T.);
#2746=ORIENTED_EDGE('',*,*,#2041,.T.);
#2747=ORIENTED_EDGE('',*,*,#2042,.T.);
#2748=ORIENTED_EDGE('',*,*,#2043,.T.);
#2749=ORIENTED_EDGE('',*,*,#1976,.F.);
#2750=ORIENTED_EDGE('',*,*,#2044,.F.);
#2751=ORIENTED_EDGE('',*,*,#2045,.T.);
#2752=ORIENTED_EDGE('',*,*,#2046,.T.);
#2753=ORIENTED_EDGE('',*,*,#2042,.F.);
#2754=ORIENTED_EDGE('',*,*,#2047,.F.);
#2755=ORIENTED_EDGE('',*,*,#2048,.T.);
#2756=ORIENTED_EDGE('',*,*,#2049,.T.);
#2757=ORIENTED_EDGE('',*,*,#2045,.F.);
#2758=ORIENTED_EDGE('',*,*,#2050,.F.);
#2759=ORIENTED_EDGE('',*,*,#2051,.T.);
#2760=ORIENTED_EDGE('',*,*,#2052,.T.);
#2761=ORIENTED_EDGE('',*,*,#2048,.F.);
#2762=ORIENTED_EDGE('',*,*,#2053,.F.);
#2763=ORIENTED_EDGE('',*,*,#2054,.T.);
#2764=ORIENTED_EDGE('',*,*,#2055,.T.);
#2765=ORIENTED_EDGE('',*,*,#2051,.F.);
#2766=ORIENTED_EDGE('',*,*,#2056,.F.);
#2767=ORIENTED_EDGE('',*,*,#2057,.T.);
#2768=ORIENTED_EDGE('',*,*,#2058,.T.);
#2769=ORIENTED_EDGE('',*,*,#2054,.F.);
#2770=ORIENTED_EDGE('',*,*,#2059,.F.);
#2771=ORIENTED_EDGE('',*,*,#2060,.T.);
#2772=ORIENTED_EDGE('',*,*,#2061,.T.);
#2773=ORIENTED_EDGE('',*,*,#2057,.F.);
#2774=ORIENTED_EDGE('',*,*,#2062,.F.);
#2775=ORIENTED_EDGE('',*,*,#2038,.T.);
#2776=ORIENTED_EDGE('',*,*,#2063,.T.);
#2777=ORIENTED_EDGE('',*,*,#2060,.F.);
#2778=ORIENTED_EDGE('',*,*,#2006,.F.);
#2779=ORIENTED_EDGE('',*,*,#1999,.T.);
#2780=ORIENTED_EDGE('',*,*,#1977,.F.);
#2781=ORIENTED_EDGE('',*,*,#2043,.F.);
#2782=ORIENTED_EDGE('',*,*,#2046,.F.);
#2783=ORIENTED_EDGE('',*,*,#2049,.F.);
#2784=ORIENTED_EDGE('',*,*,#2052,.F.);
#2785=ORIENTED_EDGE('',*,*,#2055,.F.);
#2786=ORIENTED_EDGE('',*,*,#2058,.F.);
#2787=ORIENTED_EDGE('',*,*,#2061,.F.);
#2788=ORIENTED_EDGE('',*,*,#2063,.F.);
#2789=ORIENTED_EDGE('',*,*,#2037,.F.);
#2790=ORIENTED_EDGE('',*,*,#2039,.F.);
#2791=ORIENTED_EDGE('',*,*,#2034,.F.);
#2792=ORIENTED_EDGE('',*,*,#2013,.F.);
#2793=ORIENTED_EDGE('',*,*,#2017,.F.);
#2794=ORIENTED_EDGE('',*,*,#2020,.F.);
#2795=ORIENTED_EDGE('',*,*,#2023,.F.);
#2796=ORIENTED_EDGE('',*,*,#2026,.F.);
#2797=ORIENTED_EDGE('',*,*,#2029,.F.);
#2798=ORIENTED_EDGE('',*,*,#2032,.F.);
#2799=ORIENTED_EDGE('',*,*,#2008,.F.);
#2800=ORIENTED_EDGE('',*,*,#1969,.T.);
#2801=ORIENTED_EDGE('',*,*,#2040,.F.);
#2802=ORIENTED_EDGE('',*,*,#2035,.T.);
#2803=ORIENTED_EDGE('',*,*,#2062,.T.);
#2804=ORIENTED_EDGE('',*,*,#2059,.T.);
#2805=ORIENTED_EDGE('',*,*,#2056,.T.);
#2806=ORIENTED_EDGE('',*,*,#2053,.T.);
#2807=ORIENTED_EDGE('',*,*,#2050,.T.);
#2808=ORIENTED_EDGE('',*,*,#2047,.T.);
#2809=ORIENTED_EDGE('',*,*,#2044,.T.);
#2810=ORIENTED_EDGE('',*,*,#2041,.F.);
#2811=ORIENTED_EDGE('',*,*,#1975,.T.);
#2812=ORIENTED_EDGE('',*,*,#2033,.T.);
#2813=ORIENTED_EDGE('',*,*,#2030,.T.);
#2814=ORIENTED_EDGE('',*,*,#2027,.T.);
#2815=ORIENTED_EDGE('',*,*,#2024,.T.);
#2816=ORIENTED_EDGE('',*,*,#2021,.T.);
#2817=ORIENTED_EDGE('',*,*,#2018,.T.);
#2818=ORIENTED_EDGE('',*,*,#2015,.T.);
#2819=ORIENTED_EDGE('',*,*,#2011,.T.);
#2820=ORIENTED_EDGE('',*,*,#2010,.T.);
#2821=ORIENTED_EDGE('',*,*,#2064,.T.);
#2822=ORIENTED_EDGE('',*,*,#2065,.T.);
#2823=ORIENTED_EDGE('',*,*,#2066,.T.);
#2824=ORIENTED_EDGE('',*,*,#2067,.F.);
#2825=ORIENTED_EDGE('',*,*,#2068,.T.);
#2826=ORIENTED_EDGE('',*,*,#2069,.T.);
#2827=ORIENTED_EDGE('',*,*,#2064,.F.);
#2828=ORIENTED_EDGE('',*,*,#2070,.F.);
#2829=ORIENTED_EDGE('',*,*,#2071,.T.);
#2830=ORIENTED_EDGE('',*,*,#2072,.T.);
#2831=ORIENTED_EDGE('',*,*,#2068,.F.);
#2832=ORIENTED_EDGE('',*,*,#2073,.F.);
#2833=ORIENTED_EDGE('',*,*,#2074,.T.);
#2834=ORIENTED_EDGE('',*,*,#2075,.T.);
#2835=ORIENTED_EDGE('',*,*,#2071,.F.);
#2836=ORIENTED_EDGE('',*,*,#2076,.F.);
#2837=ORIENTED_EDGE('',*,*,#2077,.F.);
#2838=ORIENTED_EDGE('',*,*,#2078,.T.);
#2839=ORIENTED_EDGE('',*,*,#2079,.T.);
#2840=ORIENTED_EDGE('',*,*,#2080,.T.);
#2841=ORIENTED_EDGE('',*,*,#2074,.F.);
#2842=ORIENTED_EDGE('',*,*,#2081,.F.);
#2843=ORIENTED_EDGE('',*,*,#2082,.T.);
#2844=ORIENTED_EDGE('',*,*,#2083,.T.);
#2845=ORIENTED_EDGE('',*,*,#2078,.F.);
#2846=ORIENTED_EDGE('',*,*,#2084,.F.);
#2847=ORIENTED_EDGE('',*,*,#2085,.T.);
#2848=ORIENTED_EDGE('',*,*,#2086,.T.);
#2849=ORIENTED_EDGE('',*,*,#2082,.F.);
#2850=ORIENTED_EDGE('',*,*,#2087,.F.);
#2851=ORIENTED_EDGE('',*,*,#2088,.F.);
#2852=ORIENTED_EDGE('',*,*,#2089,.T.);
#2853=ORIENTED_EDGE('',*,*,#2090,.T.);
#2854=ORIENTED_EDGE('',*,*,#2091,.T.);
#2855=ORIENTED_EDGE('',*,*,#2085,.F.);
#2856=ORIENTED_EDGE('',*,*,#2092,.F.);
#2857=ORIENTED_EDGE('',*,*,#2093,.F.);
#2858=ORIENTED_EDGE('',*,*,#2094,.T.);
#2859=ORIENTED_EDGE('',*,*,#2095,.T.);
#2860=ORIENTED_EDGE('',*,*,#2096,.T.);
#2861=ORIENTED_EDGE('',*,*,#2089,.F.);
#2862=ORIENTED_EDGE('',*,*,#2097,.F.);
#2863=ORIENTED_EDGE('',*,*,#2098,.T.);
#2864=ORIENTED_EDGE('',*,*,#2099,.T.);
#2865=ORIENTED_EDGE('',*,*,#2094,.F.);
#2866=ORIENTED_EDGE('',*,*,#2100,.F.);
#2867=ORIENTED_EDGE('',*,*,#2101,.T.);
#2868=ORIENTED_EDGE('',*,*,#2102,.T.);
#2869=ORIENTED_EDGE('',*,*,#2098,.F.);
#2870=ORIENTED_EDGE('',*,*,#2103,.F.);
#2871=ORIENTED_EDGE('',*,*,#2104,.F.);
#2872=ORIENTED_EDGE('',*,*,#2105,.T.);
#2873=ORIENTED_EDGE('',*,*,#2106,.T.);
#2874=ORIENTED_EDGE('',*,*,#2107,.T.);
#2875=ORIENTED_EDGE('',*,*,#2101,.F.);
#2876=ORIENTED_EDGE('',*,*,#2108,.F.);
#2877=ORIENTED_EDGE('',*,*,#2109,.T.);
#2878=ORIENTED_EDGE('',*,*,#2110,.T.);
#2879=ORIENTED_EDGE('',*,*,#2105,.F.);
#2880=ORIENTED_EDGE('',*,*,#2111,.F.);
#2881=ORIENTED_EDGE('',*,*,#2112,.T.);
#2882=ORIENTED_EDGE('',*,*,#2113,.T.);
#2883=ORIENTED_EDGE('',*,*,#2109,.F.);
#2884=ORIENTED_EDGE('',*,*,#2114,.F.);
#2885=ORIENTED_EDGE('',*,*,#2115,.F.);
#2886=ORIENTED_EDGE('',*,*,#2116,.T.);
#2887=ORIENTED_EDGE('',*,*,#2117,.T.);
#2888=ORIENTED_EDGE('',*,*,#2118,.T.);
#2889=ORIENTED_EDGE('',*,*,#2112,.F.);
#2890=ORIENTED_EDGE('',*,*,#2119,.F.);
#2891=ORIENTED_EDGE('',*,*,#2120,.F.);
#2892=ORIENTED_EDGE('',*,*,#2121,.F.);
#2893=ORIENTED_EDGE('',*,*,#2122,.F.);
#2894=ORIENTED_EDGE('',*,*,#2123,.T.);
#2895=ORIENTED_EDGE('',*,*,#2124,.T.);
#2896=ORIENTED_EDGE('',*,*,#2125,.F.);
#2897=ORIENTED_EDGE('',*,*,#2126,.F.);
#2898=ORIENTED_EDGE('',*,*,#2127,.F.);
#2899=ORIENTED_EDGE('',*,*,#2128,.F.);
#2900=ORIENTED_EDGE('',*,*,#2129,.F.);
#2901=ORIENTED_EDGE('',*,*,#2130,.F.);
#2902=ORIENTED_EDGE('',*,*,#2131,.F.);
#2903=ORIENTED_EDGE('',*,*,#2132,.F.);
#2904=ORIENTED_EDGE('',*,*,#2133,.F.);
#2905=ORIENTED_EDGE('',*,*,#2134,.F.);
#2906=ORIENTED_EDGE('',*,*,#2135,.F.);
#2907=ORIENTED_EDGE('',*,*,#2136,.F.);
#2908=ORIENTED_EDGE('',*,*,#2137,.F.);
#2909=ORIENTED_EDGE('',*,*,#2138,.F.);
#2910=ORIENTED_EDGE('',*,*,#2139,.F.);
#2911=ORIENTED_EDGE('',*,*,#2140,.F.);
#2912=ORIENTED_EDGE('',*,*,#2141,.F.);
#2913=ORIENTED_EDGE('',*,*,#2142,.F.);
#2914=ORIENTED_EDGE('',*,*,#2143,.F.);
#2915=ORIENTED_EDGE('',*,*,#2144,.F.);
#2916=ORIENTED_EDGE('',*,*,#2145,.F.);
#2917=ORIENTED_EDGE('',*,*,#2146,.F.);
#2918=ORIENTED_EDGE('',*,*,#2147,.F.);
#2919=ORIENTED_EDGE('',*,*,#2148,.F.);
#2920=ORIENTED_EDGE('',*,*,#2149,.F.);
#2921=ORIENTED_EDGE('',*,*,#2150,.F.);
#2922=ORIENTED_EDGE('',*,*,#2151,.F.);
#2923=ORIENTED_EDGE('',*,*,#2152,.F.);
#2924=ORIENTED_EDGE('',*,*,#2153,.F.);
#2925=ORIENTED_EDGE('',*,*,#2154,.F.);
#2926=ORIENTED_EDGE('',*,*,#2155,.F.);
#2927=ORIENTED_EDGE('',*,*,#2156,.F.);
#2928=ORIENTED_EDGE('',*,*,#2157,.F.);
#2929=ORIENTED_EDGE('',*,*,#2123,.F.);
#2930=ORIENTED_EDGE('',*,*,#2158,.F.);
#2931=ORIENTED_EDGE('',*,*,#2159,.F.);
#2932=ORIENTED_EDGE('',*,*,#2160,.F.);
#2933=ORIENTED_EDGE('',*,*,#2126,.T.);
#2934=ORIENTED_EDGE('',*,*,#2140,.T.);
#2935=ORIENTED_EDGE('',*,*,#2161,.F.);
#2936=ORIENTED_EDGE('',*,*,#2162,.F.);
#2937=ORIENTED_EDGE('',*,*,#2163,.F.);
#2938=ORIENTED_EDGE('',*,*,#2164,.F.);
#2939=ORIENTED_EDGE('',*,*,#2165,.F.);
#2940=ORIENTED_EDGE('',*,*,#2166,.F.);
#2941=ORIENTED_EDGE('',*,*,#2159,.T.);
#2942=ORIENTED_EDGE('',*,*,#2167,.F.);
#2943=ORIENTED_EDGE('',*,*,#2168,.F.);
#2944=ORIENTED_EDGE('',*,*,#2169,.F.);
#2945=ORIENTED_EDGE('',*,*,#2170,.F.);
#2946=ORIENTED_EDGE('',*,*,#2171,.F.);
#2947=ORIENTED_EDGE('',*,*,#2172,.F.);
#2948=ORIENTED_EDGE('',*,*,#2173,.F.);
#2949=ORIENTED_EDGE('',*,*,#2174,.F.);
#2950=ORIENTED_EDGE('',*,*,#2175,.F.);
#2951=ORIENTED_EDGE('',*,*,#2176,.F.);
#2952=ORIENTED_EDGE('',*,*,#2177,.F.);
#2953=ORIENTED_EDGE('',*,*,#2178,.F.);
#2954=ORIENTED_EDGE('',*,*,#2179,.F.);
#2955=ORIENTED_EDGE('',*,*,#2180,.F.);
#2956=ORIENTED_EDGE('',*,*,#2181,.F.);
#2957=ORIENTED_EDGE('',*,*,#2182,.F.);
#2958=ORIENTED_EDGE('',*,*,#2183,.F.);
#2959=ORIENTED_EDGE('',*,*,#2184,.T.);
#2960=ORIENTED_EDGE('',*,*,#2185,.F.);
#2961=ORIENTED_EDGE('',*,*,#2186,.F.);
#2962=ORIENTED_EDGE('',*,*,#2187,.F.);
#2963=ORIENTED_EDGE('',*,*,#2188,.F.);
#2964=ORIENTED_EDGE('',*,*,#2189,.F.);
#2965=ORIENTED_EDGE('',*,*,#2190,.F.);
#2966=ORIENTED_EDGE('',*,*,#2191,.F.);
#2967=ORIENTED_EDGE('',*,*,#2192,.F.);
#2968=ORIENTED_EDGE('',*,*,#2193,.F.);
#2969=ORIENTED_EDGE('',*,*,#2194,.F.);
#2970=ORIENTED_EDGE('',*,*,#2195,.F.);
#2971=ORIENTED_EDGE('',*,*,#2196,.F.);
#2972=ORIENTED_EDGE('',*,*,#2197,.F.);
#2973=ORIENTED_EDGE('',*,*,#2198,.F.);
#2974=ORIENTED_EDGE('',*,*,#2199,.F.);
#2975=ORIENTED_EDGE('',*,*,#2200,.F.);
#2976=ORIENTED_EDGE('',*,*,#2201,.F.);
#2977=ORIENTED_EDGE('',*,*,#2130,.T.);
#2978=ORIENTED_EDGE('',*,*,#2202,.F.);
#2979=ORIENTED_EDGE('',*,*,#2154,.T.);
#2980=ORIENTED_EDGE('',*,*,#2203,.F.);
#2981=ORIENTED_EDGE('',*,*,#2134,.T.);
#2982=ORIENTED_EDGE('',*,*,#2204,.F.);
#2983=ORIENTED_EDGE('',*,*,#2150,.T.);
#2984=ORIENTED_EDGE('',*,*,#2205,.F.);
#2985=ORIENTED_EDGE('',*,*,#2138,.T.);
#2986=ORIENTED_EDGE('',*,*,#2206,.F.);
#2987=ORIENTED_EDGE('',*,*,#2146,.T.);
#2988=ORIENTED_EDGE('',*,*,#2207,.F.);
#2989=ORIENTED_EDGE('',*,*,#2158,.T.);
#2990=ORIENTED_EDGE('',*,*,#2122,.T.);
#2991=ORIENTED_EDGE('',*,*,#2121,.T.);
#2992=ORIENTED_EDGE('',*,*,#2208,.T.);
#2993=ORIENTED_EDGE('',*,*,#2119,.T.);
#2994=ORIENTED_EDGE('',*,*,#2115,.T.);
#2995=ORIENTED_EDGE('',*,*,#2114,.T.);
#2996=ORIENTED_EDGE('',*,*,#2111,.T.);
#2997=ORIENTED_EDGE('',*,*,#2108,.T.);
#2998=ORIENTED_EDGE('',*,*,#2104,.T.);
#2999=ORIENTED_EDGE('',*,*,#2103,.T.);
#3000=ORIENTED_EDGE('',*,*,#2100,.T.);
#3001=ORIENTED_EDGE('',*,*,#2097,.T.);
#3002=ORIENTED_EDGE('',*,*,#2093,.T.);
#3003=ORIENTED_EDGE('',*,*,#2092,.T.);
#3004=ORIENTED_EDGE('',*,*,#2088,.T.);
#3005=ORIENTED_EDGE('',*,*,#2087,.T.);
#3006=ORIENTED_EDGE('',*,*,#2084,.T.);
#3007=ORIENTED_EDGE('',*,*,#2081,.T.);
#3008=ORIENTED_EDGE('',*,*,#2077,.T.);
#3009=ORIENTED_EDGE('',*,*,#2076,.T.);
#3010=ORIENTED_EDGE('',*,*,#2073,.T.);
#3011=ORIENTED_EDGE('',*,*,#2070,.T.);
#3012=ORIENTED_EDGE('',*,*,#2067,.T.);
#3013=ORIENTED_EDGE('',*,*,#2209,.T.);
#3014=ORIENTED_EDGE('',*,*,#2210,.T.);
#3015=ORIENTED_EDGE('',*,*,#2183,.T.);
#3016=ORIENTED_EDGE('',*,*,#2182,.T.);
#3017=ORIENTED_EDGE('',*,*,#2181,.T.);
#3018=ORIENTED_EDGE('',*,*,#2180,.T.);
#3019=ORIENTED_EDGE('',*,*,#2179,.T.);
#3020=ORIENTED_EDGE('',*,*,#2178,.T.);
#3021=ORIENTED_EDGE('',*,*,#2177,.T.);
#3022=ORIENTED_EDGE('',*,*,#2176,.T.);
#3023=ORIENTED_EDGE('',*,*,#2175,.T.);
#3024=ORIENTED_EDGE('',*,*,#2174,.T.);
#3025=ORIENTED_EDGE('',*,*,#2173,.T.);
#3026=ORIENTED_EDGE('',*,*,#2172,.T.);
#3027=ORIENTED_EDGE('',*,*,#2171,.T.);
#3028=ORIENTED_EDGE('',*,*,#2170,.T.);
#3029=ORIENTED_EDGE('',*,*,#2169,.T.);
#3030=ORIENTED_EDGE('',*,*,#2168,.T.);
#3031=ORIENTED_EDGE('',*,*,#2167,.T.);
#3032=ORIENTED_EDGE('',*,*,#2129,.T.);
#3033=ORIENTED_EDGE('',*,*,#2211,.T.);
#3034=ORIENTED_EDGE('',*,*,#2155,.T.);
#3035=ORIENTED_EDGE('',*,*,#2202,.T.);
#3036=ORIENTED_EDGE('',*,*,#2133,.T.);
#3037=ORIENTED_EDGE('',*,*,#2212,.T.);
#3038=ORIENTED_EDGE('',*,*,#2151,.T.);
#3039=ORIENTED_EDGE('',*,*,#2204,.T.);
#3040=ORIENTED_EDGE('',*,*,#2137,.T.);
#3041=ORIENTED_EDGE('',*,*,#2213,.T.);
#3042=ORIENTED_EDGE('',*,*,#2147,.T.);
#3043=ORIENTED_EDGE('',*,*,#2206,.T.);
#3044=ORIENTED_EDGE('',*,*,#2120,.T.);
#3045=ORIENTED_EDGE('',*,*,#2214,.T.);
#3046=ORIENTED_EDGE('',*,*,#2116,.F.);
#3047=ORIENTED_EDGE('',*,*,#2208,.F.);
#3048=ORIENTED_EDGE('',*,*,#2128,.T.);
#3049=ORIENTED_EDGE('',*,*,#2215,.T.);
#3050=ORIENTED_EDGE('',*,*,#2156,.T.);
#3051=ORIENTED_EDGE('',*,*,#2211,.F.);
#3052=ORIENTED_EDGE('',*,*,#2132,.T.);
#3053=ORIENTED_EDGE('',*,*,#2216,.T.);
#3054=ORIENTED_EDGE('',*,*,#2152,.T.);
#3055=ORIENTED_EDGE('',*,*,#2212,.F.);
#3056=ORIENTED_EDGE('',*,*,#2136,.T.);
#3057=ORIENTED_EDGE('',*,*,#2217,.T.);
#3058=ORIENTED_EDGE('',*,*,#2148,.T.);
#3059=ORIENTED_EDGE('',*,*,#2213,.F.);
#3060=ORIENTED_EDGE('',*,*,#2127,.T.);
#3061=ORIENTED_EDGE('',*,*,#2160,.T.);
#3062=ORIENTED_EDGE('',*,*,#2201,.T.);
#3063=ORIENTED_EDGE('',*,*,#2200,.T.);
#3064=ORIENTED_EDGE('',*,*,#2199,.T.);
#3065=ORIENTED_EDGE('',*,*,#2198,.T.);
#3066=ORIENTED_EDGE('',*,*,#2197,.T.);
#3067=ORIENTED_EDGE('',*,*,#2196,.T.);
#3068=ORIENTED_EDGE('',*,*,#2195,.T.);
#3069=ORIENTED_EDGE('',*,*,#2194,.T.);
#3070=ORIENTED_EDGE('',*,*,#2193,.T.);
#3071=ORIENTED_EDGE('',*,*,#2192,.T.);
#3072=ORIENTED_EDGE('',*,*,#2191,.T.);
#3073=ORIENTED_EDGE('',*,*,#2190,.T.);
#3074=ORIENTED_EDGE('',*,*,#2189,.T.);
#3075=ORIENTED_EDGE('',*,*,#2188,.T.);
#3076=ORIENTED_EDGE('',*,*,#2187,.T.);
#3077=ORIENTED_EDGE('',*,*,#2186,.T.);
#3078=ORIENTED_EDGE('',*,*,#2185,.T.);
#3079=ORIENTED_EDGE('',*,*,#2218,.T.);
#3080=ORIENTED_EDGE('',*,*,#2065,.F.);
#3081=ORIENTED_EDGE('',*,*,#2069,.F.);
#3082=ORIENTED_EDGE('',*,*,#2072,.F.);
#3083=ORIENTED_EDGE('',*,*,#2075,.F.);
#3084=ORIENTED_EDGE('',*,*,#2080,.F.);
#3085=ORIENTED_EDGE('',*,*,#2079,.F.);
#3086=ORIENTED_EDGE('',*,*,#2083,.F.);
#3087=ORIENTED_EDGE('',*,*,#2086,.F.);
#3088=ORIENTED_EDGE('',*,*,#2091,.F.);
#3089=ORIENTED_EDGE('',*,*,#2090,.F.);
#3090=ORIENTED_EDGE('',*,*,#2096,.F.);
#3091=ORIENTED_EDGE('',*,*,#2095,.F.);
#3092=ORIENTED_EDGE('',*,*,#2099,.F.);
#3093=ORIENTED_EDGE('',*,*,#2102,.F.);
#3094=ORIENTED_EDGE('',*,*,#2107,.F.);
#3095=ORIENTED_EDGE('',*,*,#2106,.F.);
#3096=ORIENTED_EDGE('',*,*,#2110,.F.);
#3097=ORIENTED_EDGE('',*,*,#2113,.F.);
#3098=ORIENTED_EDGE('',*,*,#2118,.F.);
#3099=ORIENTED_EDGE('',*,*,#2117,.F.);
#3100=ORIENTED_EDGE('',*,*,#2214,.F.);
#3101=ORIENTED_EDGE('',*,*,#2124,.F.);
#3102=ORIENTED_EDGE('',*,*,#2157,.T.);
#3103=ORIENTED_EDGE('',*,*,#2215,.F.);
#3104=ORIENTED_EDGE('',*,*,#2131,.T.);
#3105=ORIENTED_EDGE('',*,*,#2203,.T.);
#3106=ORIENTED_EDGE('',*,*,#2153,.T.);
#3107=ORIENTED_EDGE('',*,*,#2125,.T.);
#3108=ORIENTED_EDGE('',*,*,#2216,.F.);
#3109=ORIENTED_EDGE('',*,*,#2135,.T.);
#3110=ORIENTED_EDGE('',*,*,#2205,.T.);
#3111=ORIENTED_EDGE('',*,*,#2149,.T.);
#3112=ORIENTED_EDGE('',*,*,#2217,.F.);
#3113=ORIENTED_EDGE('',*,*,#2139,.T.);
#3114=ORIENTED_EDGE('',*,*,#2207,.T.);
#3115=ORIENTED_EDGE('',*,*,#2145,.T.);
#3116=ORIENTED_EDGE('',*,*,#2219,.F.);
#3117=ORIENTED_EDGE('',*,*,#2162,.T.);
#3118=ORIENTED_EDGE('',*,*,#2161,.T.);
#3119=ORIENTED_EDGE('',*,*,#2142,.T.);
#3120=ORIENTED_EDGE('',*,*,#2220,.F.);
#3121=ORIENTED_EDGE('',*,*,#2165,.T.);
#3122=ORIENTED_EDGE('',*,*,#2221,.F.);
#3123=ORIENTED_EDGE('',*,*,#2144,.T.);
#3124=ORIENTED_EDGE('',*,*,#2222,.F.);
#3125=ORIENTED_EDGE('',*,*,#2163,.T.);
#3126=ORIENTED_EDGE('',*,*,#2219,.T.);
#3127=ORIENTED_EDGE('',*,*,#2141,.T.);
#3128=ORIENTED_EDGE('',*,*,#2166,.T.);
#3129=ORIENTED_EDGE('',*,*,#2220,.T.);
#3130=ORIENTED_EDGE('',*,*,#2143,.T.);
#3131=ORIENTED_EDGE('',*,*,#2221,.T.);
#3132=ORIENTED_EDGE('',*,*,#2164,.T.);
#3133=ORIENTED_EDGE('',*,*,#2222,.T.);
#3134=ORIENTED_EDGE('',*,*,#2218,.F.);
#3135=ORIENTED_EDGE('',*,*,#2184,.F.);
#3136=ORIENTED_EDGE('',*,*,#2210,.F.);
#3137=ORIENTED_EDGE('',*,*,#2209,.F.);
#3138=ORIENTED_EDGE('',*,*,#2066,.F.);
#3139=ORIENTED_EDGE('',*,*,#2223,.F.);
#3140=ORIENTED_EDGE('',*,*,#2224,.F.);
#3141=ORIENTED_EDGE('',*,*,#2225,.T.);
#3142=ORIENTED_EDGE('',*,*,#2226,.T.);
#3143=ORIENTED_EDGE('',*,*,#2227,.F.);
#3144=ORIENTED_EDGE('',*,*,#2228,.F.);
#3145=ORIENTED_EDGE('',*,*,#2229,.F.);
#3146=ORIENTED_EDGE('',*,*,#2223,.T.);
#3147=ORIENTED_EDGE('',*,*,#2230,.T.);
#3148=ORIENTED_EDGE('',*,*,#2231,.T.);
#3149=ORIENTED_EDGE('',*,*,#2232,.F.);
#3150=ORIENTED_EDGE('',*,*,#2233,.F.);
#3151=ORIENTED_EDGE('',*,*,#2234,.F.);
#3152=ORIENTED_EDGE('',*,*,#2227,.T.);
#3153=ORIENTED_EDGE('',*,*,#2235,.T.);
#3154=ORIENTED_EDGE('',*,*,#2236,.T.);
#3155=ORIENTED_EDGE('',*,*,#2237,.F.);
#3156=ORIENTED_EDGE('',*,*,#2238,.F.);
#3157=ORIENTED_EDGE('',*,*,#2239,.F.);
#3158=ORIENTED_EDGE('',*,*,#2232,.T.);
#3159=ORIENTED_EDGE('',*,*,#2240,.T.);
#3160=ORIENTED_EDGE('',*,*,#2241,.T.);
#3161=ORIENTED_EDGE('',*,*,#2242,.F.);
#3162=ORIENTED_EDGE('',*,*,#2243,.F.);
#3163=ORIENTED_EDGE('',*,*,#2244,.F.);
#3164=ORIENTED_EDGE('',*,*,#2245,.T.);
#3165=ORIENTED_EDGE('',*,*,#2246,.F.);
#3166=ORIENTED_EDGE('',*,*,#2247,.F.);
#3167=ORIENTED_EDGE('',*,*,#2248,.F.);
#3168=ORIENTED_EDGE('',*,*,#2249,.F.);
#3169=ORIENTED_EDGE('',*,*,#2242,.T.);
#3170=ORIENTED_EDGE('',*,*,#2250,.F.);
#3171=ORIENTED_EDGE('',*,*,#2251,.F.);
#3172=ORIENTED_EDGE('',*,*,#2252,.F.);
#3173=ORIENTED_EDGE('',*,*,#2253,.F.);
#3174=ORIENTED_EDGE('',*,*,#2247,.T.);
#3175=ORIENTED_EDGE('',*,*,#2254,.F.);
#3176=ORIENTED_EDGE('',*,*,#2255,.F.);
#3177=ORIENTED_EDGE('',*,*,#2256,.F.);
#3178=ORIENTED_EDGE('',*,*,#2257,.F.);
#3179=ORIENTED_EDGE('',*,*,#2251,.T.);
#3180=ORIENTED_EDGE('',*,*,#2258,.F.);
#3181=ORIENTED_EDGE('',*,*,#2255,.T.);
#3182=ORIENTED_EDGE('',*,*,#2259,.F.);
#3183=ORIENTED_EDGE('',*,*,#2260,.T.);
#3184=ORIENTED_EDGE('',*,*,#2261,.F.);
#3185=ORIENTED_EDGE('',*,*,#2237,.T.);
#3186=ORIENTED_EDGE('',*,*,#2262,.T.);
#3187=ORIENTED_EDGE('',*,*,#2263,.T.);
#3188=ORIENTED_EDGE('',*,*,#2264,.T.);
#3189=ORIENTED_EDGE('',*,*,#2265,.F.);
#3190=ORIENTED_EDGE('',*,*,#2266,.F.);
#3191=ORIENTED_EDGE('',*,*,#2267,.T.);
#3192=ORIENTED_EDGE('',*,*,#2268,.T.);
#3193=ORIENTED_EDGE('',*,*,#2259,.T.);
#3194=ORIENTED_EDGE('',*,*,#2258,.T.);
#3195=ORIENTED_EDGE('',*,*,#2254,.T.);
#3196=ORIENTED_EDGE('',*,*,#2250,.T.);
#3197=ORIENTED_EDGE('',*,*,#2246,.T.);
#3198=ORIENTED_EDGE('',*,*,#2269,.T.);
#3199=ORIENTED_EDGE('',*,*,#2224,.T.);
#3200=ORIENTED_EDGE('',*,*,#2229,.T.);
#3201=ORIENTED_EDGE('',*,*,#2228,.T.);
#3202=ORIENTED_EDGE('',*,*,#2234,.T.);
#3203=ORIENTED_EDGE('',*,*,#2233,.T.);
#3204=ORIENTED_EDGE('',*,*,#2239,.T.);
#3205=ORIENTED_EDGE('',*,*,#2238,.T.);
#3206=ORIENTED_EDGE('',*,*,#2266,.T.);
#3207=ORIENTED_EDGE('',*,*,#2265,.T.);
#3208=ORIENTED_EDGE('',*,*,#2270,.T.);
#3209=ORIENTED_EDGE('',*,*,#2263,.F.);
#3210=ORIENTED_EDGE('',*,*,#2262,.F.);
#3211=ORIENTED_EDGE('',*,*,#2241,.F.);
#3212=ORIENTED_EDGE('',*,*,#2240,.F.);
#3213=ORIENTED_EDGE('',*,*,#2236,.F.);
#3214=ORIENTED_EDGE('',*,*,#2235,.F.);
#3215=ORIENTED_EDGE('',*,*,#2231,.F.);
#3216=ORIENTED_EDGE('',*,*,#2230,.F.);
#3217=ORIENTED_EDGE('',*,*,#2226,.F.);
#3218=ORIENTED_EDGE('',*,*,#2271,.T.);
#3219=ORIENTED_EDGE('',*,*,#2244,.T.);
#3220=ORIENTED_EDGE('',*,*,#2243,.T.);
#3221=ORIENTED_EDGE('',*,*,#2249,.T.);
#3222=ORIENTED_EDGE('',*,*,#2248,.T.);
#3223=ORIENTED_EDGE('',*,*,#2253,.T.);
#3224=ORIENTED_EDGE('',*,*,#2252,.T.);
#3225=ORIENTED_EDGE('',*,*,#2257,.T.);
#3226=ORIENTED_EDGE('',*,*,#2256,.T.);
#3227=ORIENTED_EDGE('',*,*,#2261,.T.);
#3228=ORIENTED_EDGE('',*,*,#2272,.F.);
#3229=ORIENTED_EDGE('',*,*,#2273,.F.);
#3230=ORIENTED_EDGE('',*,*,#2274,.F.);
#3231=ORIENTED_EDGE('',*,*,#2275,.F.);
#3232=ORIENTED_EDGE('',*,*,#2276,.F.);
#3233=ORIENTED_EDGE('',*,*,#2277,.F.);
#3234=ORIENTED_EDGE('',*,*,#2269,.F.);
#3235=ORIENTED_EDGE('',*,*,#2245,.F.);
#3236=ORIENTED_EDGE('',*,*,#2271,.F.);
#3237=ORIENTED_EDGE('',*,*,#2225,.F.);
#3238=ORIENTED_EDGE('',*,*,#2277,.T.);
#3239=ORIENTED_EDGE('',*,*,#2278,.T.);
#3240=ORIENTED_EDGE('',*,*,#2279,.T.);
#3241=ORIENTED_EDGE('',*,*,#2280,.F.);
#3242=ORIENTED_EDGE('',*,*,#2276,.T.);
#3243=ORIENTED_EDGE('',*,*,#2281,.T.);
#3244=ORIENTED_EDGE('',*,*,#2282,.T.);
#3245=ORIENTED_EDGE('',*,*,#2278,.F.);
#3246=ORIENTED_EDGE('',*,*,#2275,.T.);
#3247=ORIENTED_EDGE('',*,*,#2283,.T.);
#3248=ORIENTED_EDGE('',*,*,#2284,.T.);
#3249=ORIENTED_EDGE('',*,*,#2281,.F.);
#3250=ORIENTED_EDGE('',*,*,#2274,.T.);
#3251=ORIENTED_EDGE('',*,*,#2285,.T.);
#3252=ORIENTED_EDGE('',*,*,#2286,.T.);
#3253=ORIENTED_EDGE('',*,*,#2283,.F.);
#3254=ORIENTED_EDGE('',*,*,#2273,.T.);
#3255=ORIENTED_EDGE('',*,*,#2287,.T.);
#3256=ORIENTED_EDGE('',*,*,#2288,.T.);
#3257=ORIENTED_EDGE('',*,*,#2285,.F.);
#3258=ORIENTED_EDGE('',*,*,#2272,.T.);
#3259=ORIENTED_EDGE('',*,*,#2280,.T.);
#3260=ORIENTED_EDGE('',*,*,#2289,.T.);
#3261=ORIENTED_EDGE('',*,*,#2287,.F.);
#3262=ORIENTED_EDGE('',*,*,#2289,.F.);
#3263=ORIENTED_EDGE('',*,*,#2279,.F.);
#3264=ORIENTED_EDGE('',*,*,#2282,.F.);
#3265=ORIENTED_EDGE('',*,*,#2284,.F.);
#3266=ORIENTED_EDGE('',*,*,#2286,.F.);
#3267=ORIENTED_EDGE('',*,*,#2288,.F.);
#3268=ORIENTED_EDGE('',*,*,#2267,.F.);
#3269=ORIENTED_EDGE('',*,*,#2264,.F.);
#3270=ORIENTED_EDGE('',*,*,#2270,.F.);
#3271=ORIENTED_EDGE('',*,*,#2260,.F.);
#3272=ORIENTED_EDGE('',*,*,#2268,.F.);
#3273=ORIENTED_EDGE('',*,*,#2290,.F.);
#3274=ORIENTED_EDGE('',*,*,#2291,.T.);
#3275=ORIENTED_EDGE('',*,*,#2292,.F.);
#3276=ORIENTED_EDGE('',*,*,#2291,.F.);
#3277=ORIENTED_EDGE('',*,*,#2293,.F.);
#3278=ORIENTED_EDGE('',*,*,#2294,.T.);
#3279=ORIENTED_EDGE('',*,*,#2295,.T.);
#3280=ORIENTED_EDGE('',*,*,#2294,.F.);
#3281=ORIENTED_EDGE('',*,*,#2296,.F.);
#3282=ORIENTED_EDGE('',*,*,#2297,.T.);
#3283=ORIENTED_EDGE('',*,*,#2293,.T.);
#3284=ORIENTED_EDGE('',*,*,#2297,.F.);
#3285=ORIENTED_EDGE('',*,*,#2296,.T.);
#3286=ORIENTED_EDGE('',*,*,#2290,.T.);
#3287=ORIENTED_EDGE('',*,*,#2298,.F.);
#3288=ORIENTED_EDGE('',*,*,#2292,.T.);
#3289=ORIENTED_EDGE('',*,*,#2299,.F.);
#3290=ORIENTED_EDGE('',*,*,#2300,.T.);
#3291=ORIENTED_EDGE('',*,*,#2298,.T.);
#3292=ORIENTED_EDGE('',*,*,#2300,.F.);
#3293=ORIENTED_EDGE('',*,*,#2295,.F.);
#3294=ORIENTED_EDGE('',*,*,#2301,.T.);
#3295=ORIENTED_EDGE('',*,*,#2299,.T.);
#3296=ORIENTED_EDGE('',*,*,#2301,.F.);
#3297=ORIENTED_EDGE('',*,*,#2302,.T.);
#3298=ORIENTED_EDGE('',*,*,#2303,.T.);
#3299=ORIENTED_EDGE('',*,*,#2304,.F.);
#3300=ORIENTED_EDGE('',*,*,#2305,.F.);
#3301=ORIENTED_EDGE('',*,*,#2306,.T.);
#3302=ORIENTED_EDGE('',*,*,#2307,.T.);
#3303=ORIENTED_EDGE('',*,*,#2308,.T.);
#3304=ORIENTED_EDGE('',*,*,#2302,.F.);
#3305=ORIENTED_EDGE('',*,*,#2309,.F.);
#3306=ORIENTED_EDGE('',*,*,#2310,.F.);
#3307=ORIENTED_EDGE('',*,*,#2311,.T.);
#3308=ORIENTED_EDGE('',*,*,#2312,.T.);
#3309=ORIENTED_EDGE('',*,*,#2313,.T.);
#3310=ORIENTED_EDGE('',*,*,#2306,.F.);
#3311=ORIENTED_EDGE('',*,*,#2314,.F.);
#3312=ORIENTED_EDGE('',*,*,#2315,.F.);
#3313=ORIENTED_EDGE('',*,*,#2316,.F.);
#3314=ORIENTED_EDGE('',*,*,#2317,.F.);
#3315=ORIENTED_EDGE('',*,*,#2318,.F.);
#3316=ORIENTED_EDGE('',*,*,#2319,.F.);
#3317=ORIENTED_EDGE('',*,*,#2320,.T.);
#3318=ORIENTED_EDGE('',*,*,#2321,.T.);
#3319=ORIENTED_EDGE('',*,*,#2322,.T.);
#3320=ORIENTED_EDGE('',*,*,#2323,.T.);
#3321=ORIENTED_EDGE('',*,*,#2324,.T.);
#3322=ORIENTED_EDGE('',*,*,#2325,.F.);
#3323=ORIENTED_EDGE('',*,*,#2326,.T.);
#3324=ORIENTED_EDGE('',*,*,#2327,.T.);
#3325=ORIENTED_EDGE('',*,*,#2328,.T.);
#3326=ORIENTED_EDGE('',*,*,#2329,.T.);
#3327=ORIENTED_EDGE('',*,*,#2322,.F.);
#3328=ORIENTED_EDGE('',*,*,#2330,.T.);
#3329=ORIENTED_EDGE('',*,*,#2331,.T.);
#3330=ORIENTED_EDGE('',*,*,#2332,.T.);
#3331=ORIENTED_EDGE('',*,*,#2333,.T.);
#3332=ORIENTED_EDGE('',*,*,#2334,.T.);
#3333=ORIENTED_EDGE('',*,*,#2327,.F.);
#3334=ORIENTED_EDGE('',*,*,#2335,.T.);
#3335=ORIENTED_EDGE('',*,*,#2336,.F.);
#3336=ORIENTED_EDGE('',*,*,#2337,.T.);
#3337=ORIENTED_EDGE('',*,*,#2338,.F.);
#3338=ORIENTED_EDGE('',*,*,#2339,.T.);
#3339=ORIENTED_EDGE('',*,*,#2336,.T.);
#3340=ORIENTED_EDGE('',*,*,#2340,.T.);
#3341=ORIENTED_EDGE('',*,*,#2341,.T.);
#3342=ORIENTED_EDGE('',*,*,#2332,.F.);
#3343=ORIENTED_EDGE('',*,*,#2342,.T.);
#3344=ORIENTED_EDGE('',*,*,#2343,.T.);
#3345=ORIENTED_EDGE('',*,*,#2316,.T.);
#3346=ORIENTED_EDGE('',*,*,#2344,.T.);
#3347=ORIENTED_EDGE('',*,*,#2345,.T.);
#3348=ORIENTED_EDGE('',*,*,#2311,.F.);
#3349=ORIENTED_EDGE('',*,*,#2346,.F.);
#3350=ORIENTED_EDGE('',*,*,#2347,.F.);
#3351=ORIENTED_EDGE('',*,*,#2348,.F.);
#3352=ORIENTED_EDGE('',*,*,#2303,.F.);
#3353=ORIENTED_EDGE('',*,*,#2308,.F.);
#3354=ORIENTED_EDGE('',*,*,#2307,.F.);
#3355=ORIENTED_EDGE('',*,*,#2313,.F.);
#3356=ORIENTED_EDGE('',*,*,#2312,.F.);
#3357=ORIENTED_EDGE('',*,*,#2345,.F.);
#3358=ORIENTED_EDGE('',*,*,#2344,.F.);
#3359=ORIENTED_EDGE('',*,*,#2321,.F.);
#3360=ORIENTED_EDGE('',*,*,#2320,.F.);
#3361=ORIENTED_EDGE('',*,*,#2349,.F.);
#3362=ORIENTED_EDGE('',*,*,#2337,.F.);
#3363=ORIENTED_EDGE('',*,*,#2343,.F.);
#3364=ORIENTED_EDGE('',*,*,#2342,.F.);
#3365=ORIENTED_EDGE('',*,*,#2335,.F.);
#3366=ORIENTED_EDGE('',*,*,#2331,.F.);
#3367=ORIENTED_EDGE('',*,*,#2330,.F.);
#3368=ORIENTED_EDGE('',*,*,#2326,.F.);
#3369=ORIENTED_EDGE('',*,*,#2350,.F.);
#3370=ORIENTED_EDGE('',*,*,#2351,.F.);
#3371=ORIENTED_EDGE('',*,*,#2324,.F.);
#3372=ORIENTED_EDGE('',*,*,#2323,.F.);
#3373=ORIENTED_EDGE('',*,*,#2329,.F.);
#3374=ORIENTED_EDGE('',*,*,#2328,.F.);
#3375=ORIENTED_EDGE('',*,*,#2334,.F.);
#3376=ORIENTED_EDGE('',*,*,#2333,.F.);
#3377=ORIENTED_EDGE('',*,*,#2341,.F.);
#3378=ORIENTED_EDGE('',*,*,#2340,.F.);
#3379=ORIENTED_EDGE('',*,*,#2339,.F.);
#3380=ORIENTED_EDGE('',*,*,#2352,.F.);
#3381=ORIENTED_EDGE('',*,*,#2318,.T.);
#3382=ORIENTED_EDGE('',*,*,#2317,.T.);
#3383=ORIENTED_EDGE('',*,*,#2347,.T.);
#3384=ORIENTED_EDGE('',*,*,#2346,.T.);
#3385=ORIENTED_EDGE('',*,*,#2315,.T.);
#3386=ORIENTED_EDGE('',*,*,#2314,.T.);
#3387=ORIENTED_EDGE('',*,*,#2310,.T.);
#3388=ORIENTED_EDGE('',*,*,#2309,.T.);
#3389=ORIENTED_EDGE('',*,*,#2305,.T.);
#3390=ORIENTED_EDGE('',*,*,#2353,.T.);
#3391=ORIENTED_EDGE('',*,*,#2354,.T.);
#3392=ORIENTED_EDGE('',*,*,#2355,.T.);
#3393=ORIENTED_EDGE('',*,*,#2356,.T.);
#3394=ORIENTED_EDGE('',*,*,#2357,.T.);
#3395=ORIENTED_EDGE('',*,*,#2358,.T.);
#3396=ORIENTED_EDGE('',*,*,#2349,.T.);
#3397=ORIENTED_EDGE('',*,*,#2319,.T.);
#3398=ORIENTED_EDGE('',*,*,#2352,.T.);
#3399=ORIENTED_EDGE('',*,*,#2338,.T.);
#3400=ORIENTED_EDGE('',*,*,#2354,.F.);
#3401=ORIENTED_EDGE('',*,*,#2359,.T.);
#3402=ORIENTED_EDGE('',*,*,#2360,.F.);
#3403=ORIENTED_EDGE('',*,*,#2361,.F.);
#3404=ORIENTED_EDGE('',*,*,#2355,.F.);
#3405=ORIENTED_EDGE('',*,*,#2361,.T.);
#3406=ORIENTED_EDGE('',*,*,#2362,.F.);
#3407=ORIENTED_EDGE('',*,*,#2363,.F.);
#3408=ORIENTED_EDGE('',*,*,#2356,.F.);
#3409=ORIENTED_EDGE('',*,*,#2363,.T.);
#3410=ORIENTED_EDGE('',*,*,#2364,.F.);
#3411=ORIENTED_EDGE('',*,*,#2365,.F.);
#3412=ORIENTED_EDGE('',*,*,#2357,.F.);
#3413=ORIENTED_EDGE('',*,*,#2365,.T.);
#3414=ORIENTED_EDGE('',*,*,#2366,.F.);
#3415=ORIENTED_EDGE('',*,*,#2367,.F.);
#3416=ORIENTED_EDGE('',*,*,#2358,.F.);
#3417=ORIENTED_EDGE('',*,*,#2367,.T.);
#3418=ORIENTED_EDGE('',*,*,#2368,.F.);
#3419=ORIENTED_EDGE('',*,*,#2369,.F.);
#3420=ORIENTED_EDGE('',*,*,#2353,.F.);
#3421=ORIENTED_EDGE('',*,*,#2369,.T.);
#3422=ORIENTED_EDGE('',*,*,#2370,.F.);
#3423=ORIENTED_EDGE('',*,*,#2359,.F.);
#3424=ORIENTED_EDGE('',*,*,#2370,.T.);
#3425=ORIENTED_EDGE('',*,*,#2368,.T.);
#3426=ORIENTED_EDGE('',*,*,#2366,.T.);
#3427=ORIENTED_EDGE('',*,*,#2364,.T.);
#3428=ORIENTED_EDGE('',*,*,#2362,.T.);
#3429=ORIENTED_EDGE('',*,*,#2360,.T.);
#3430=ORIENTED_EDGE('',*,*,#2348,.T.);
#3431=ORIENTED_EDGE('',*,*,#2350,.T.);
#3432=ORIENTED_EDGE('',*,*,#2325,.T.);
#3433=ORIENTED_EDGE('',*,*,#2351,.T.);
#3434=ORIENTED_EDGE('',*,*,#2304,.T.);
#3435=ORIENTED_EDGE('',*,*,#2371,.F.);
#3436=ORIENTED_EDGE('',*,*,#2372,.F.);
#3437=ORIENTED_EDGE('',*,*,#2373,.F.);
#3438=ORIENTED_EDGE('',*,*,#2374,.T.);
#3439=ORIENTED_EDGE('',*,*,#2375,.F.);
#3440=ORIENTED_EDGE('',*,*,#2376,.F.);
#3441=ORIENTED_EDGE('',*,*,#2377,.F.);
#3442=ORIENTED_EDGE('',*,*,#2371,.T.);
#3443=ORIENTED_EDGE('',*,*,#2378,.T.);
#3444=ORIENTED_EDGE('',*,*,#2379,.F.);
#3445=ORIENTED_EDGE('',*,*,#2380,.F.);
#3446=ORIENTED_EDGE('',*,*,#2375,.T.);
#3447=ORIENTED_EDGE('',*,*,#2381,.T.);
#3448=ORIENTED_EDGE('',*,*,#2382,.T.);
#3449=ORIENTED_EDGE('',*,*,#2383,.F.);
#3450=ORIENTED_EDGE('',*,*,#2384,.F.);
#3451=ORIENTED_EDGE('',*,*,#2385,.F.);
#3452=ORIENTED_EDGE('',*,*,#2379,.T.);
#3453=ORIENTED_EDGE('',*,*,#2386,.T.);
#3454=ORIENTED_EDGE('',*,*,#2387,.F.);
#3455=ORIENTED_EDGE('',*,*,#2388,.F.);
#3456=ORIENTED_EDGE('',*,*,#2383,.T.);
#3457=ORIENTED_EDGE('',*,*,#2389,.T.);
#3458=ORIENTED_EDGE('',*,*,#2390,.T.);
#3459=ORIENTED_EDGE('',*,*,#2391,.F.);
#3460=ORIENTED_EDGE('',*,*,#2392,.F.);
#3461=ORIENTED_EDGE('',*,*,#2393,.F.);
#3462=ORIENTED_EDGE('',*,*,#2387,.T.);
#3463=ORIENTED_EDGE('',*,*,#2394,.T.);
#3464=ORIENTED_EDGE('',*,*,#2395,.F.);
#3465=ORIENTED_EDGE('',*,*,#2396,.F.);
#3466=ORIENTED_EDGE('',*,*,#2391,.T.);
#3467=ORIENTED_EDGE('',*,*,#2397,.T.);
#3468=ORIENTED_EDGE('',*,*,#2398,.T.);
#3469=ORIENTED_EDGE('',*,*,#2399,.F.);
#3470=ORIENTED_EDGE('',*,*,#2400,.F.);
#3471=ORIENTED_EDGE('',*,*,#2401,.F.);
#3472=ORIENTED_EDGE('',*,*,#2395,.T.);
#3473=ORIENTED_EDGE('',*,*,#2402,.T.);
#3474=ORIENTED_EDGE('',*,*,#2403,.F.);
#3475=ORIENTED_EDGE('',*,*,#2404,.F.);
#3476=ORIENTED_EDGE('',*,*,#2399,.T.);
#3477=ORIENTED_EDGE('',*,*,#2405,.T.);
#3478=ORIENTED_EDGE('',*,*,#2406,.T.);
#3479=ORIENTED_EDGE('',*,*,#2407,.F.);
#3480=ORIENTED_EDGE('',*,*,#2408,.F.);
#3481=ORIENTED_EDGE('',*,*,#2409,.F.);
#3482=ORIENTED_EDGE('',*,*,#2403,.T.);
#3483=ORIENTED_EDGE('',*,*,#2410,.T.);
#3484=ORIENTED_EDGE('',*,*,#2411,.F.);
#3485=ORIENTED_EDGE('',*,*,#2412,.F.);
#3486=ORIENTED_EDGE('',*,*,#2407,.T.);
#3487=ORIENTED_EDGE('',*,*,#2413,.T.);
#3488=ORIENTED_EDGE('',*,*,#2414,.T.);
#3489=ORIENTED_EDGE('',*,*,#2415,.F.);
#3490=ORIENTED_EDGE('',*,*,#2416,.F.);
#3491=ORIENTED_EDGE('',*,*,#2417,.F.);
#3492=ORIENTED_EDGE('',*,*,#2411,.T.);
#3493=ORIENTED_EDGE('',*,*,#2418,.T.);
#3494=ORIENTED_EDGE('',*,*,#2419,.F.);
#3495=ORIENTED_EDGE('',*,*,#2420,.F.);
#3496=ORIENTED_EDGE('',*,*,#2415,.T.);
#3497=ORIENTED_EDGE('',*,*,#2421,.T.);
#3498=ORIENTED_EDGE('',*,*,#2422,.T.);
#3499=ORIENTED_EDGE('',*,*,#2423,.F.);
#3500=ORIENTED_EDGE('',*,*,#2424,.F.);
#3501=ORIENTED_EDGE('',*,*,#2425,.F.);
#3502=ORIENTED_EDGE('',*,*,#2419,.T.);
#3503=ORIENTED_EDGE('',*,*,#2426,.T.);
#3504=ORIENTED_EDGE('',*,*,#2427,.F.);
#3505=ORIENTED_EDGE('',*,*,#2428,.F.);
#3506=ORIENTED_EDGE('',*,*,#2423,.T.);
#3507=ORIENTED_EDGE('',*,*,#2429,.T.);
#3508=ORIENTED_EDGE('',*,*,#2430,.T.);
#3509=ORIENTED_EDGE('',*,*,#2431,.F.);
#3510=ORIENTED_EDGE('',*,*,#2432,.F.);
#3511=ORIENTED_EDGE('',*,*,#2433,.F.);
#3512=ORIENTED_EDGE('',*,*,#2427,.T.);
#3513=ORIENTED_EDGE('',*,*,#2434,.T.);
#3514=ORIENTED_EDGE('',*,*,#2435,.F.);
#3515=ORIENTED_EDGE('',*,*,#2436,.F.);
#3516=ORIENTED_EDGE('',*,*,#2431,.T.);
#3517=ORIENTED_EDGE('',*,*,#2437,.T.);
#3518=ORIENTED_EDGE('',*,*,#2438,.T.);
#3519=ORIENTED_EDGE('',*,*,#2439,.F.);
#3520=ORIENTED_EDGE('',*,*,#2440,.F.);
#3521=ORIENTED_EDGE('',*,*,#2441,.F.);
#3522=ORIENTED_EDGE('',*,*,#2435,.T.);
#3523=ORIENTED_EDGE('',*,*,#2442,.T.);
#3524=ORIENTED_EDGE('',*,*,#2443,.F.);
#3525=ORIENTED_EDGE('',*,*,#2444,.F.);
#3526=ORIENTED_EDGE('',*,*,#2439,.T.);
#3527=ORIENTED_EDGE('',*,*,#2445,.T.);
#3528=ORIENTED_EDGE('',*,*,#2446,.T.);
#3529=ORIENTED_EDGE('',*,*,#2447,.F.);
#3530=ORIENTED_EDGE('',*,*,#2448,.F.);
#3531=ORIENTED_EDGE('',*,*,#2449,.F.);
#3532=ORIENTED_EDGE('',*,*,#2443,.T.);
#3533=ORIENTED_EDGE('',*,*,#2450,.T.);
#3534=ORIENTED_EDGE('',*,*,#2451,.T.);
#3535=ORIENTED_EDGE('',*,*,#2452,.T.);
#3536=ORIENTED_EDGE('',*,*,#2453,.F.);
#3537=ORIENTED_EDGE('',*,*,#2454,.T.);
#3538=ORIENTED_EDGE('',*,*,#2455,.T.);
#3539=ORIENTED_EDGE('',*,*,#2456,.T.);
#3540=ORIENTED_EDGE('',*,*,#2457,.T.);
#3541=ORIENTED_EDGE('',*,*,#2458,.T.);
#3542=ORIENTED_EDGE('',*,*,#2459,.T.);
#3543=ORIENTED_EDGE('',*,*,#2460,.T.);
#3544=ORIENTED_EDGE('',*,*,#2461,.T.);
#3545=ORIENTED_EDGE('',*,*,#2462,.T.);
#3546=ORIENTED_EDGE('',*,*,#2463,.T.);
#3547=ORIENTED_EDGE('',*,*,#2464,.T.);
#3548=ORIENTED_EDGE('',*,*,#2465,.T.);
#3549=ORIENTED_EDGE('',*,*,#2466,.T.);
#3550=ORIENTED_EDGE('',*,*,#2467,.T.);
#3551=ORIENTED_EDGE('',*,*,#2468,.T.);
#3552=ORIENTED_EDGE('',*,*,#2469,.T.);
#3553=ORIENTED_EDGE('',*,*,#2470,.T.);
#3554=ORIENTED_EDGE('',*,*,#2471,.T.);
#3555=ORIENTED_EDGE('',*,*,#2472,.T.);
#3556=ORIENTED_EDGE('',*,*,#2473,.T.);
#3557=ORIENTED_EDGE('',*,*,#2474,.T.);
#3558=ORIENTED_EDGE('',*,*,#2475,.F.);
#3559=ORIENTED_EDGE('',*,*,#2476,.T.);
#3560=ORIENTED_EDGE('',*,*,#2477,.T.);
#3561=ORIENTED_EDGE('',*,*,#2478,.T.);
#3562=ORIENTED_EDGE('',*,*,#2479,.T.);
#3563=ORIENTED_EDGE('',*,*,#2480,.T.);
#3564=ORIENTED_EDGE('',*,*,#2481,.T.);
#3565=ORIENTED_EDGE('',*,*,#2482,.T.);
#3566=ORIENTED_EDGE('',*,*,#2483,.T.);
#3567=ORIENTED_EDGE('',*,*,#2484,.T.);
#3568=ORIENTED_EDGE('',*,*,#2485,.T.);
#3569=ORIENTED_EDGE('',*,*,#2486,.T.);
#3570=ORIENTED_EDGE('',*,*,#2487,.T.);
#3571=ORIENTED_EDGE('',*,*,#2488,.T.);
#3572=ORIENTED_EDGE('',*,*,#2489,.T.);
#3573=ORIENTED_EDGE('',*,*,#2490,.T.);
#3574=ORIENTED_EDGE('',*,*,#2491,.T.);
#3575=ORIENTED_EDGE('',*,*,#2492,.T.);
#3576=ORIENTED_EDGE('',*,*,#2493,.T.);
#3577=ORIENTED_EDGE('',*,*,#2494,.T.);
#3578=ORIENTED_EDGE('',*,*,#2495,.T.);
#3579=ORIENTED_EDGE('',*,*,#2447,.T.);
#3580=ORIENTED_EDGE('',*,*,#2496,.T.);
#3581=ORIENTED_EDGE('',*,*,#2497,.F.);
#3582=ORIENTED_EDGE('',*,*,#2498,.F.);
#3583=ORIENTED_EDGE('',*,*,#2499,.F.);
#3584=ORIENTED_EDGE('',*,*,#2500,.F.);
#3585=ORIENTED_EDGE('',*,*,#2474,.F.);
#3586=ORIENTED_EDGE('',*,*,#2473,.F.);
#3587=ORIENTED_EDGE('',*,*,#2472,.F.);
#3588=ORIENTED_EDGE('',*,*,#2471,.F.);
#3589=ORIENTED_EDGE('',*,*,#2470,.F.);
#3590=ORIENTED_EDGE('',*,*,#2469,.F.);
#3591=ORIENTED_EDGE('',*,*,#2468,.F.);
#3592=ORIENTED_EDGE('',*,*,#2467,.F.);
#3593=ORIENTED_EDGE('',*,*,#2466,.F.);
#3594=ORIENTED_EDGE('',*,*,#2465,.F.);
#3595=ORIENTED_EDGE('',*,*,#2464,.F.);
#3596=ORIENTED_EDGE('',*,*,#2463,.F.);
#3597=ORIENTED_EDGE('',*,*,#2462,.F.);
#3598=ORIENTED_EDGE('',*,*,#2461,.F.);
#3599=ORIENTED_EDGE('',*,*,#2460,.F.);
#3600=ORIENTED_EDGE('',*,*,#2459,.F.);
#3601=ORIENTED_EDGE('',*,*,#2458,.F.);
#3602=ORIENTED_EDGE('',*,*,#2457,.F.);
#3603=ORIENTED_EDGE('',*,*,#2456,.F.);
#3604=ORIENTED_EDGE('',*,*,#2455,.F.);
#3605=ORIENTED_EDGE('',*,*,#2454,.F.);
#3606=ORIENTED_EDGE('',*,*,#2501,.F.);
#3607=ORIENTED_EDGE('',*,*,#2372,.T.);
#3608=ORIENTED_EDGE('',*,*,#2377,.T.);
#3609=ORIENTED_EDGE('',*,*,#2376,.T.);
#3610=ORIENTED_EDGE('',*,*,#2380,.T.);
#3611=ORIENTED_EDGE('',*,*,#2385,.T.);
#3612=ORIENTED_EDGE('',*,*,#2384,.T.);
#3613=ORIENTED_EDGE('',*,*,#2388,.T.);
#3614=ORIENTED_EDGE('',*,*,#2393,.T.);
#3615=ORIENTED_EDGE('',*,*,#2392,.T.);
#3616=ORIENTED_EDGE('',*,*,#2396,.T.);
#3617=ORIENTED_EDGE('',*,*,#2401,.T.);
#3618=ORIENTED_EDGE('',*,*,#2400,.T.);
#3619=ORIENTED_EDGE('',*,*,#2404,.T.);
#3620=ORIENTED_EDGE('',*,*,#2409,.T.);
#3621=ORIENTED_EDGE('',*,*,#2408,.T.);
#3622=ORIENTED_EDGE('',*,*,#2412,.T.);
#3623=ORIENTED_EDGE('',*,*,#2417,.T.);
#3624=ORIENTED_EDGE('',*,*,#2416,.T.);
#3625=ORIENTED_EDGE('',*,*,#2420,.T.);
#3626=ORIENTED_EDGE('',*,*,#2425,.T.);
#3627=ORIENTED_EDGE('',*,*,#2424,.T.);
#3628=ORIENTED_EDGE('',*,*,#2428,.T.);
#3629=ORIENTED_EDGE('',*,*,#2433,.T.);
#3630=ORIENTED_EDGE('',*,*,#2432,.T.);
#3631=ORIENTED_EDGE('',*,*,#2436,.T.);
#3632=ORIENTED_EDGE('',*,*,#2441,.T.);
#3633=ORIENTED_EDGE('',*,*,#2440,.T.);
#3634=ORIENTED_EDGE('',*,*,#2444,.T.);
#3635=ORIENTED_EDGE('',*,*,#2449,.T.);
#3636=ORIENTED_EDGE('',*,*,#2448,.T.);
#3637=ORIENTED_EDGE('',*,*,#2499,.T.);
#3638=ORIENTED_EDGE('',*,*,#2498,.T.);
#3639=ORIENTED_EDGE('',*,*,#2502,.F.);
#3640=ORIENTED_EDGE('',*,*,#2503,.F.);
#3641=ORIENTED_EDGE('',*,*,#2496,.F.);
#3642=ORIENTED_EDGE('',*,*,#2451,.F.);
#3643=ORIENTED_EDGE('',*,*,#2450,.F.);
#3644=ORIENTED_EDGE('',*,*,#2446,.F.);
#3645=ORIENTED_EDGE('',*,*,#2445,.F.);
#3646=ORIENTED_EDGE('',*,*,#2442,.F.);
#3647=ORIENTED_EDGE('',*,*,#2438,.F.);
#3648=ORIENTED_EDGE('',*,*,#2437,.F.);
#3649=ORIENTED_EDGE('',*,*,#2434,.F.);
#3650=ORIENTED_EDGE('',*,*,#2430,.F.);
#3651=ORIENTED_EDGE('',*,*,#2429,.F.);
#3652=ORIENTED_EDGE('',*,*,#2426,.F.);
#3653=ORIENTED_EDGE('',*,*,#2422,.F.);
#3654=ORIENTED_EDGE('',*,*,#2421,.F.);
#3655=ORIENTED_EDGE('',*,*,#2418,.F.);
#3656=ORIENTED_EDGE('',*,*,#2414,.F.);
#3657=ORIENTED_EDGE('',*,*,#2413,.F.);
#3658=ORIENTED_EDGE('',*,*,#2410,.F.);
#3659=ORIENTED_EDGE('',*,*,#2406,.F.);
#3660=ORIENTED_EDGE('',*,*,#2405,.F.);
#3661=ORIENTED_EDGE('',*,*,#2402,.F.);
#3662=ORIENTED_EDGE('',*,*,#2398,.F.);
#3663=ORIENTED_EDGE('',*,*,#2397,.F.);
#3664=ORIENTED_EDGE('',*,*,#2394,.F.);
#3665=ORIENTED_EDGE('',*,*,#2390,.F.);
#3666=ORIENTED_EDGE('',*,*,#2389,.F.);
#3667=ORIENTED_EDGE('',*,*,#2386,.F.);
#3668=ORIENTED_EDGE('',*,*,#2382,.F.);
#3669=ORIENTED_EDGE('',*,*,#2381,.F.);
#3670=ORIENTED_EDGE('',*,*,#2378,.F.);
#3671=ORIENTED_EDGE('',*,*,#2374,.F.);
#3672=ORIENTED_EDGE('',*,*,#2504,.F.);
#3673=ORIENTED_EDGE('',*,*,#2452,.F.);
#3674=ORIENTED_EDGE('',*,*,#2495,.F.);
#3675=ORIENTED_EDGE('',*,*,#2494,.F.);
#3676=ORIENTED_EDGE('',*,*,#2493,.F.);
#3677=ORIENTED_EDGE('',*,*,#2492,.F.);
#3678=ORIENTED_EDGE('',*,*,#2491,.F.);
#3679=ORIENTED_EDGE('',*,*,#2490,.F.);
#3680=ORIENTED_EDGE('',*,*,#2489,.F.);
#3681=ORIENTED_EDGE('',*,*,#2488,.F.);
#3682=ORIENTED_EDGE('',*,*,#2487,.F.);
#3683=ORIENTED_EDGE('',*,*,#2486,.F.);
#3684=ORIENTED_EDGE('',*,*,#2485,.F.);
#3685=ORIENTED_EDGE('',*,*,#2484,.F.);
#3686=ORIENTED_EDGE('',*,*,#2483,.F.);
#3687=ORIENTED_EDGE('',*,*,#2482,.F.);
#3688=ORIENTED_EDGE('',*,*,#2481,.F.);
#3689=ORIENTED_EDGE('',*,*,#2480,.F.);
#3690=ORIENTED_EDGE('',*,*,#2479,.F.);
#3691=ORIENTED_EDGE('',*,*,#2478,.F.);
#3692=ORIENTED_EDGE('',*,*,#2477,.F.);
#3693=ORIENTED_EDGE('',*,*,#2476,.F.);
#3694=ORIENTED_EDGE('',*,*,#2500,.T.);
#3695=ORIENTED_EDGE('',*,*,#2497,.T.);
#3696=ORIENTED_EDGE('',*,*,#2503,.T.);
#3697=ORIENTED_EDGE('',*,*,#2502,.T.);
#3698=ORIENTED_EDGE('',*,*,#2475,.T.);
#3699=ORIENTED_EDGE('',*,*,#2501,.T.);
#3700=ORIENTED_EDGE('',*,*,#2453,.T.);
#3701=ORIENTED_EDGE('',*,*,#2504,.T.);
#3702=ORIENTED_EDGE('',*,*,#2373,.T.);
#3703=ORIENTED_EDGE('',*,*,#2505,.T.);
#3704=ORIENTED_EDGE('',*,*,#2506,.T.);
#3705=ORIENTED_EDGE('',*,*,#2507,.T.);
#3706=ORIENTED_EDGE('',*,*,#2508,.T.);
#3707=ORIENTED_EDGE('',*,*,#2509,.T.);
#3708=ORIENTED_EDGE('',*,*,#2510,.T.);
#3709=ORIENTED_EDGE('',*,*,#2511,.T.);
#3710=ORIENTED_EDGE('',*,*,#2509,.F.);
#3711=ORIENTED_EDGE('',*,*,#2512,.T.);
#3712=ORIENTED_EDGE('',*,*,#2513,.F.);
#3713=ORIENTED_EDGE('',*,*,#2514,.F.);
#3714=ORIENTED_EDGE('',*,*,#2515,.F.);
#3715=ORIENTED_EDGE('',*,*,#2516,.T.);
#3716=ORIENTED_EDGE('',*,*,#2508,.F.);
#3717=ORIENTED_EDGE('',*,*,#2517,.T.);
#3718=ORIENTED_EDGE('',*,*,#2518,.F.);
#3719=ORIENTED_EDGE('',*,*,#2519,.F.);
#3720=ORIENTED_EDGE('',*,*,#2520,.F.);
#3721=ORIENTED_EDGE('',*,*,#2521,.T.);
#3722=ORIENTED_EDGE('',*,*,#2522,.F.);
#3723=ORIENTED_EDGE('',*,*,#2523,.F.);
#3724=ORIENTED_EDGE('',*,*,#2524,.F.);
#3725=ORIENTED_EDGE('',*,*,#2512,.F.);
#3726=ORIENTED_EDGE('',*,*,#2525,.T.);
#3727=ORIENTED_EDGE('',*,*,#2507,.F.);
#3728=ORIENTED_EDGE('',*,*,#2526,.T.);
#3729=ORIENTED_EDGE('',*,*,#2527,.F.);
#3730=ORIENTED_EDGE('',*,*,#2517,.F.);
#3731=ORIENTED_EDGE('',*,*,#2506,.F.);
#3732=ORIENTED_EDGE('',*,*,#2528,.T.);
#3733=ORIENTED_EDGE('',*,*,#2529,.F.);
#3734=ORIENTED_EDGE('',*,*,#2530,.T.);
#3735=ORIENTED_EDGE('',*,*,#2531,.F.);
#3736=ORIENTED_EDGE('',*,*,#2532,.F.);
#3737=ORIENTED_EDGE('',*,*,#2533,.F.);
#3738=ORIENTED_EDGE('',*,*,#2526,.F.);
#3739=ORIENTED_EDGE('',*,*,#2534,.T.);
#3740=ORIENTED_EDGE('',*,*,#2535,.F.);
#3741=ORIENTED_EDGE('',*,*,#2536,.T.);
#3742=ORIENTED_EDGE('',*,*,#2513,.T.);
#3743=ORIENTED_EDGE('',*,*,#2524,.T.);
#3744=ORIENTED_EDGE('',*,*,#2529,.T.);
#3745=ORIENTED_EDGE('',*,*,#2537,.T.);
#3746=ORIENTED_EDGE('',*,*,#2522,.T.);
#3747=ORIENTED_EDGE('',*,*,#2538,.T.);
#3748=ORIENTED_EDGE('',*,*,#2538,.F.);
#3749=ORIENTED_EDGE('',*,*,#2521,.F.);
#3750=ORIENTED_EDGE('',*,*,#2539,.F.);
#3751=ORIENTED_EDGE('',*,*,#2530,.F.);
#3752=ORIENTED_EDGE('',*,*,#2533,.T.);
#3753=ORIENTED_EDGE('',*,*,#2540,.T.);
#3754=ORIENTED_EDGE('',*,*,#2518,.T.);
#3755=ORIENTED_EDGE('',*,*,#2527,.T.);
#3756=ORIENTED_EDGE('',*,*,#2540,.F.);
#3757=ORIENTED_EDGE('',*,*,#2532,.T.);
#3758=ORIENTED_EDGE('',*,*,#2541,.F.);
#3759=ORIENTED_EDGE('',*,*,#2519,.T.);
#3760=ORIENTED_EDGE('',*,*,#2531,.T.);
#3761=ORIENTED_EDGE('',*,*,#2539,.T.);
#3762=ORIENTED_EDGE('',*,*,#2520,.T.);
#3763=ORIENTED_EDGE('',*,*,#2541,.T.);
#3764=ORIENTED_EDGE('',*,*,#2525,.F.);
#3765=ORIENTED_EDGE('',*,*,#2542,.T.);
#3766=ORIENTED_EDGE('',*,*,#2534,.F.);
#3767=ORIENTED_EDGE('',*,*,#2542,.F.);
#3768=ORIENTED_EDGE('',*,*,#2505,.F.);
#3769=ORIENTED_EDGE('',*,*,#2543,.T.);
#3770=ORIENTED_EDGE('',*,*,#2544,.F.);
#3771=ORIENTED_EDGE('',*,*,#2535,.T.);
#3772=ORIENTED_EDGE('',*,*,#2523,.T.);
#3773=ORIENTED_EDGE('',*,*,#2537,.F.);
#3774=ORIENTED_EDGE('',*,*,#2528,.F.);
#3775=ORIENTED_EDGE('',*,*,#2545,.T.);
#3776=ORIENTED_EDGE('',*,*,#2546,.T.);
#3777=ORIENTED_EDGE('',*,*,#2547,.F.);
#3778=ORIENTED_EDGE('',*,*,#2546,.F.);
#3779=ORIENTED_EDGE('',*,*,#2548,.T.);
#3780=ORIENTED_EDGE('',*,*,#2549,.T.);
#3781=ORIENTED_EDGE('',*,*,#2550,.F.);
#3782=ORIENTED_EDGE('',*,*,#2551,.F.);
#3783=ORIENTED_EDGE('',*,*,#2552,.T.);
#3784=ORIENTED_EDGE('',*,*,#2551,.T.);
#3785=ORIENTED_EDGE('',*,*,#2553,.F.);
#3786=ORIENTED_EDGE('',*,*,#2554,.F.);
#3787=ORIENTED_EDGE('',*,*,#2555,.T.);
#3788=ORIENTED_EDGE('',*,*,#2554,.T.);
#3789=ORIENTED_EDGE('',*,*,#2556,.F.);
#3790=ORIENTED_EDGE('',*,*,#2557,.F.);
#3791=ORIENTED_EDGE('',*,*,#2558,.T.);
#3792=ORIENTED_EDGE('',*,*,#2557,.T.);
#3793=ORIENTED_EDGE('',*,*,#2559,.F.);
#3794=ORIENTED_EDGE('',*,*,#2560,.F.);
#3795=ORIENTED_EDGE('',*,*,#2561,.T.);
#3796=ORIENTED_EDGE('',*,*,#2560,.T.);
#3797=ORIENTED_EDGE('',*,*,#2562,.F.);
#3798=ORIENTED_EDGE('',*,*,#2563,.F.);
#3799=ORIENTED_EDGE('',*,*,#2564,.T.);
#3800=ORIENTED_EDGE('',*,*,#2563,.T.);
#3801=ORIENTED_EDGE('',*,*,#2565,.F.);
#3802=ORIENTED_EDGE('',*,*,#2566,.F.);
#3803=ORIENTED_EDGE('',*,*,#2567,.T.);
#3804=ORIENTED_EDGE('',*,*,#2566,.T.);
#3805=ORIENTED_EDGE('',*,*,#2568,.F.);
#3806=ORIENTED_EDGE('',*,*,#2569,.F.);
#3807=ORIENTED_EDGE('',*,*,#2570,.T.);
#3808=ORIENTED_EDGE('',*,*,#2569,.T.);
#3809=ORIENTED_EDGE('',*,*,#2571,.F.);
#3810=ORIENTED_EDGE('',*,*,#2549,.F.);
#3811=ORIENTED_EDGE('',*,*,#2572,.T.);
#3812=ORIENTED_EDGE('',*,*,#2573,.T.);
#3813=ORIENTED_EDGE('',*,*,#2574,.F.);
#3814=ORIENTED_EDGE('',*,*,#2575,.F.);
#3815=ORIENTED_EDGE('',*,*,#2511,.F.);
#3816=ORIENTED_EDGE('',*,*,#2576,.F.);
#3817=ORIENTED_EDGE('',*,*,#2575,.T.);
#3818=ORIENTED_EDGE('',*,*,#2577,.F.);
#3819=ORIENTED_EDGE('',*,*,#2543,.F.);
#3820=ORIENTED_EDGE('',*,*,#2578,.F.);
#3821=ORIENTED_EDGE('',*,*,#2515,.T.);
#3822=ORIENTED_EDGE('',*,*,#2579,.F.);
#3823=ORIENTED_EDGE('',*,*,#2580,.F.);
#3824=ORIENTED_EDGE('',*,*,#2581,.T.);
#3825=ORIENTED_EDGE('',*,*,#2580,.T.);
#3826=ORIENTED_EDGE('',*,*,#2582,.F.);
#3827=ORIENTED_EDGE('',*,*,#2583,.F.);
#3828=ORIENTED_EDGE('',*,*,#2584,.T.);
#3829=ORIENTED_EDGE('',*,*,#2583,.T.);
#3830=ORIENTED_EDGE('',*,*,#2585,.F.);
#3831=ORIENTED_EDGE('',*,*,#2586,.F.);
#3832=ORIENTED_EDGE('',*,*,#2587,.T.);
#3833=ORIENTED_EDGE('',*,*,#2586,.T.);
#3834=ORIENTED_EDGE('',*,*,#2588,.F.);
#3835=ORIENTED_EDGE('',*,*,#2589,.F.);
#3836=ORIENTED_EDGE('',*,*,#2590,.T.);
#3837=ORIENTED_EDGE('',*,*,#2589,.T.);
#3838=ORIENTED_EDGE('',*,*,#2591,.F.);
#3839=ORIENTED_EDGE('',*,*,#2592,.F.);
#3840=ORIENTED_EDGE('',*,*,#2593,.T.);
#3841=ORIENTED_EDGE('',*,*,#2592,.T.);
#3842=ORIENTED_EDGE('',*,*,#2594,.F.);
#3843=ORIENTED_EDGE('',*,*,#2595,.F.);
#3844=ORIENTED_EDGE('',*,*,#2596,.T.);
#3845=ORIENTED_EDGE('',*,*,#2595,.T.);
#3846=ORIENTED_EDGE('',*,*,#2597,.F.);
#3847=ORIENTED_EDGE('',*,*,#2598,.F.);
#3848=ORIENTED_EDGE('',*,*,#2599,.T.);
#3849=ORIENTED_EDGE('',*,*,#2598,.T.);
#3850=ORIENTED_EDGE('',*,*,#2600,.F.);
#3851=ORIENTED_EDGE('',*,*,#2573,.F.);
#3852=ORIENTED_EDGE('',*,*,#2577,.T.);
#3853=ORIENTED_EDGE('',*,*,#2574,.T.);
#3854=ORIENTED_EDGE('',*,*,#2600,.T.);
#3855=ORIENTED_EDGE('',*,*,#2597,.T.);
#3856=ORIENTED_EDGE('',*,*,#2594,.T.);
#3857=ORIENTED_EDGE('',*,*,#2591,.T.);
#3858=ORIENTED_EDGE('',*,*,#2588,.T.);
#3859=ORIENTED_EDGE('',*,*,#2585,.T.);
#3860=ORIENTED_EDGE('',*,*,#2582,.T.);
#3861=ORIENTED_EDGE('',*,*,#2579,.T.);
#3862=ORIENTED_EDGE('',*,*,#2514,.T.);
#3863=ORIENTED_EDGE('',*,*,#2536,.F.);
#3864=ORIENTED_EDGE('',*,*,#2544,.T.);
#3865=ORIENTED_EDGE('',*,*,#2571,.T.);
#3866=ORIENTED_EDGE('',*,*,#2568,.T.);
#3867=ORIENTED_EDGE('',*,*,#2565,.T.);
#3868=ORIENTED_EDGE('',*,*,#2562,.T.);
#3869=ORIENTED_EDGE('',*,*,#2559,.T.);
#3870=ORIENTED_EDGE('',*,*,#2556,.T.);
#3871=ORIENTED_EDGE('',*,*,#2553,.T.);
#3872=ORIENTED_EDGE('',*,*,#2550,.T.);
#3873=ORIENTED_EDGE('',*,*,#2547,.T.);
#3874=ORIENTED_EDGE('',*,*,#2510,.F.);
#3875=ORIENTED_EDGE('',*,*,#2516,.F.);
#3876=ORIENTED_EDGE('',*,*,#2578,.T.);
#3877=ORIENTED_EDGE('',*,*,#2581,.F.);
#3878=ORIENTED_EDGE('',*,*,#2584,.F.);
#3879=ORIENTED_EDGE('',*,*,#2587,.F.);
#3880=ORIENTED_EDGE('',*,*,#2590,.F.);
#3881=ORIENTED_EDGE('',*,*,#2593,.F.);
#3882=ORIENTED_EDGE('',*,*,#2596,.F.);
#3883=ORIENTED_EDGE('',*,*,#2599,.F.);
#3884=ORIENTED_EDGE('',*,*,#2572,.F.);
#3885=ORIENTED_EDGE('',*,*,#2576,.T.);
#3886=ORIENTED_EDGE('',*,*,#2570,.F.);
#3887=ORIENTED_EDGE('',*,*,#2548,.F.);
#3888=ORIENTED_EDGE('',*,*,#2552,.F.);
#3889=ORIENTED_EDGE('',*,*,#2555,.F.);
#3890=ORIENTED_EDGE('',*,*,#2558,.F.);
#3891=ORIENTED_EDGE('',*,*,#2561,.F.);
#3892=ORIENTED_EDGE('',*,*,#2564,.F.);
#3893=ORIENTED_EDGE('',*,*,#2567,.F.);
#3894=ORIENTED_EDGE('',*,*,#2545,.F.);
#3895=ORIENTED_EDGE('',*,*,#2601,.F.);
#3896=ORIENTED_EDGE('',*,*,#2602,.F.);
#3897=ORIENTED_EDGE('',*,*,#2603,.F.);
#3898=ORIENTED_EDGE('',*,*,#2604,.F.);
#3899=ORIENTED_EDGE('',*,*,#2605,.F.);
#3900=ORIENTED_EDGE('',*,*,#2606,.F.);
#3901=ORIENTED_EDGE('',*,*,#2607,.T.);
#3902=ORIENTED_EDGE('',*,*,#2602,.T.);
#3903=ORIENTED_EDGE('',*,*,#2608,.F.);
#3904=ORIENTED_EDGE('',*,*,#2609,.F.);
#3905=ORIENTED_EDGE('',*,*,#2603,.T.);
#3906=ORIENTED_EDGE('',*,*,#2607,.F.);
#3907=ORIENTED_EDGE('',*,*,#2605,.T.);
#3908=ORIENTED_EDGE('',*,*,#2610,.T.);
#3909=ORIENTED_EDGE('',*,*,#2611,.T.);
#3910=ORIENTED_EDGE('',*,*,#2606,.T.);
#3911=ORIENTED_EDGE('',*,*,#2612,.T.);
#3912=ORIENTED_EDGE('',*,*,#2613,.T.);
#3913=ORIENTED_EDGE('',*,*,#2608,.T.);
#3914=ORIENTED_EDGE('',*,*,#2601,.T.);
#3915=ORIENTED_EDGE('',*,*,#2610,.F.);
#3916=ORIENTED_EDGE('',*,*,#2604,.T.);
#3917=ORIENTED_EDGE('',*,*,#2609,.T.);
#3918=ORIENTED_EDGE('',*,*,#2613,.F.);
#3919=ORIENTED_EDGE('',*,*,#2611,.F.);
#3920=ORIENTED_EDGE('',*,*,#2614,.T.);
#3921=ORIENTED_EDGE('',*,*,#2615,.T.);
#3922=ORIENTED_EDGE('',*,*,#2616,.T.);
#3923=ORIENTED_EDGE('',*,*,#2614,.F.);
#3924=ORIENTED_EDGE('',*,*,#2616,.F.);
#3925=ORIENTED_EDGE('',*,*,#2617,.F.);
#3926=ORIENTED_EDGE('',*,*,#2617,.T.);
#3927=ORIENTED_EDGE('',*,*,#2615,.F.);
#3928=ORIENTED_EDGE('',*,*,#2612,.F.);
#3929=ORIENTED_EDGE('',*,*,#2618,.T.);
#3930=ORIENTED_EDGE('',*,*,#2619,.T.);
#3931=ORIENTED_EDGE('',*,*,#2620,.T.);
#3932=ORIENTED_EDGE('',*,*,#2619,.F.);
#3933=ORIENTED_EDGE('',*,*,#2621,.T.);
#3934=ORIENTED_EDGE('',*,*,#2622,.T.);
#3935=ORIENTED_EDGE('',*,*,#2623,.F.);
#3936=ORIENTED_EDGE('',*,*,#2623,.T.);
#3937=ORIENTED_EDGE('',*,*,#2624,.T.);
#3938=ORIENTED_EDGE('',*,*,#2621,.F.);
#3939=ORIENTED_EDGE('',*,*,#2622,.F.);
#3940=ORIENTED_EDGE('',*,*,#2625,.T.);
#3941=ORIENTED_EDGE('',*,*,#2626,.T.);
#3942=ORIENTED_EDGE('',*,*,#2625,.F.);
#3943=ORIENTED_EDGE('',*,*,#2627,.F.);
#3944=ORIENTED_EDGE('',*,*,#2627,.T.);
#3945=ORIENTED_EDGE('',*,*,#2628,.T.);
#3946=ORIENTED_EDGE('',*,*,#2624,.F.);
#3947=ORIENTED_EDGE('',*,*,#2628,.F.);
#3948=ORIENTED_EDGE('',*,*,#2626,.F.);
#3949=ORIENTED_EDGE('',*,*,#2618,.F.);
#3950=ORIENTED_EDGE('',*,*,#2620,.F.);
#3951=CYLINDRICAL_SURFACE('',#4359,3.);
#3952=CYLINDRICAL_SURFACE('',#4378,0.5);
#3953=CYLINDRICAL_SURFACE('',#4380,3.5);
#3954=CYLINDRICAL_SURFACE('',#4381,24.7141941620437);
#3955=CYLINDRICAL_SURFACE('',#4382,9.);
#3956=CYLINDRICAL_SURFACE('',#4384,9.);
#3957=CYLINDRICAL_SURFACE('',#4385,4.445);
#3958=CYLINDRICAL_SURFACE('',#4387,4.445);
#3959=CYLINDRICAL_SURFACE('',#4391,3.99999999999999);
#3960=CYLINDRICAL_SURFACE('',#4395,4.00000000000001);
#3961=CYLINDRICAL_SURFACE('',#4399,4.00000000000001);
#3962=CYLINDRICAL_SURFACE('',#4403,4.00000000000001);
#3963=CYLINDRICAL_SURFACE('',#4406,6.99999999999999);
#3964=CYLINDRICAL_SURFACE('',#4409,9.9094315895918);
#3965=CYLINDRICAL_SURFACE('',#4412,5.);
#3966=CYLINDRICAL_SURFACE('',#4416,5.99999999999999);
#3967=CYLINDRICAL_SURFACE('',#4420,5.99999999999999);
#3968=CYLINDRICAL_SURFACE('',#4424,7.);
#3969=CYLINDRICAL_SURFACE('',#4431,3.22274999999998);
#3970=CYLINDRICAL_SURFACE('',#4433,3.22274999999998);
#3971=CYLINDRICAL_SURFACE('',#4434,3.22274999999998);
#3972=CYLINDRICAL_SURFACE('',#4435,3.22274999999998);
#3973=CYLINDRICAL_SURFACE('',#4436,3.22274999999998);
#3974=CYLINDRICAL_SURFACE('',#4437,3.22274999999998);
#3975=CYLINDRICAL_SURFACE('',#4438,3.22274999999998);
#3976=CYLINDRICAL_SURFACE('',#4439,3.22274999999998);
#3977=CYLINDRICAL_SURFACE('',#4440,3.22274999999998);
#3978=CYLINDRICAL_SURFACE('',#4441,3.22274999999998);
#3979=CYLINDRICAL_SURFACE('',#4442,3.22274999999998);
#3980=CYLINDRICAL_SURFACE('',#4443,3.22274999999998);
#3981=CYLINDRICAL_SURFACE('',#4444,3.22274999999998);
#3982=CYLINDRICAL_SURFACE('',#4445,3.22274999999998);
#3983=CYLINDRICAL_SURFACE('',#4446,3.22274999999998);
#3984=CYLINDRICAL_SURFACE('',#4447,3.22274999999998);
#3985=CYLINDRICAL_SURFACE('',#4450,5.);
#3986=CYLINDRICAL_SURFACE('',#4454,3.933);
#3987=CYLINDRICAL_SURFACE('',#4456,3.933);
#3988=CYLINDRICAL_SURFACE('',#4457,3.933);
#3989=CYLINDRICAL_SURFACE('',#4458,3.933);
#3990=CYLINDRICAL_SURFACE('',#4459,3.22274999999998);
#3991=CYLINDRICAL_SURFACE('',#4460,3.22274999999998);
#3992=CYLINDRICAL_SURFACE('',#4461,3.22274999999998);
#3993=CYLINDRICAL_SURFACE('',#4462,3.22274999999998);
#3994=CYLINDRICAL_SURFACE('',#4463,3.933);
#3995=CYLINDRICAL_SURFACE('',#4464,3.22274999999998);
#3996=CYLINDRICAL_SURFACE('',#4467,4.08499999999997);
#3997=CYLINDRICAL_SURFACE('',#4469,4.08499999999997);
#3998=CYLINDRICAL_SURFACE('',#4470,4.08499999999997);
#3999=CYLINDRICAL_SURFACE('',#4471,4.08499999999997);
#4000=CYLINDRICAL_SURFACE('',#4472,3.38975);
#4001=CYLINDRICAL_SURFACE('',#4474,3.38975);
#4002=CYLINDRICAL_SURFACE('',#4475,3.38975);
#4003=CYLINDRICAL_SURFACE('',#4476,3.38975);
#4004=CYLINDRICAL_SURFACE('',#4477,3.38975);
#4005=CYLINDRICAL_SURFACE('',#4479,4.08499999999997);
#4006=CYLINDRICAL_SURFACE('',#4490,5.);
#4007=CYLINDRICAL_SURFACE('',#4493,10.5388214764323);
#4008=CYLINDRICAL_SURFACE('',#4508,4.08499999999997);
#4009=CYLINDRICAL_SURFACE('',#4510,4.08499999999997);
#4010=CYLINDRICAL_SURFACE('',#4511,4.08499999999997);
#4011=CYLINDRICAL_SURFACE('',#4512,4.08499999999997);
#4012=CYLINDRICAL_SURFACE('',#4514,3.38975);
#4013=CYLINDRICAL_SURFACE('',#4516,3.38975);
#4014=CYLINDRICAL_SURFACE('',#4517,3.38975);
#4015=CYLINDRICAL_SURFACE('',#4518,3.38975);
#4016=CYLINDRICAL_SURFACE('',#4520,3.38975);
#4017=CYLINDRICAL_SURFACE('',#4521,4.08499999999997);
#4018=CYLINDRICAL_SURFACE('',#4531,3.22274999999998);
#4019=CYLINDRICAL_SURFACE('',#4533,3.22274999999998);
#4020=CYLINDRICAL_SURFACE('',#4534,3.22274999999998);
#4021=CYLINDRICAL_SURFACE('',#4535,3.22274999999998);
#4022=CYLINDRICAL_SURFACE('',#4536,3.22274999999998);
#4023=CYLINDRICAL_SURFACE('',#4537,3.22274999999998);
#4024=CYLINDRICAL_SURFACE('',#4538,3.22274999999998);
#4025=CYLINDRICAL_SURFACE('',#4539,3.22274999999998);
#4026=CYLINDRICAL_SURFACE('',#4540,3.22274999999998);
#4027=CYLINDRICAL_SURFACE('',#4541,3.22274999999998);
#4028=CYLINDRICAL_SURFACE('',#4542,3.22274999999998);
#4029=CYLINDRICAL_SURFACE('',#4543,3.22274999999998);
#4030=CYLINDRICAL_SURFACE('',#4544,3.22274999999998);
#4031=CYLINDRICAL_SURFACE('',#4545,3.22274999999998);
#4032=CYLINDRICAL_SURFACE('',#4546,3.22274999999998);
#4033=CYLINDRICAL_SURFACE('',#4547,3.22274999999998);
#4034=CYLINDRICAL_SURFACE('',#4548,3.22274999999998);
#4035=CYLINDRICAL_SURFACE('',#4549,3.22274999999998);
#4036=CYLINDRICAL_SURFACE('',#4550,3.22274999999998);
#4037=CYLINDRICAL_SURFACE('',#4551,3.22274999999998);
#4038=CYLINDRICAL_SURFACE('',#4552,3.933);
#4039=CYLINDRICAL_SURFACE('',#4555,3.22274999999998);
#4040=CYLINDRICAL_SURFACE('',#4560,3.);
#4041=CYLINDRICAL_SURFACE('',#4579,0.5);
#4042=CYLINDRICAL_SURFACE('',#4581,3.5);
#4043=CYLINDRICAL_SURFACE('',#4582,24.7141941620437);
#4044=CYLINDRICAL_SURFACE('',#4583,9.);
#4045=CYLINDRICAL_SURFACE('',#4585,9.);
#4046=CYLINDRICAL_SURFACE('',#4586,4.445);
#4047=CYLINDRICAL_SURFACE('',#4588,4.445);
#4048=CYLINDRICAL_SURFACE('',#4592,3.99999999999999);
#4049=CYLINDRICAL_SURFACE('',#4596,4.00000000000001);
#4050=CYLINDRICAL_SURFACE('',#4600,4.00000000000001);
#4051=CYLINDRICAL_SURFACE('',#4604,4.00000000000001);
#4052=CYLINDRICAL_SURFACE('',#4607,6.99999999999999);
#4053=CYLINDRICAL_SURFACE('',#4610,9.9094315895918);
#4054=CYLINDRICAL_SURFACE('',#4613,5.);
#4055=CYLINDRICAL_SURFACE('',#4617,5.99999999999999);
#4056=CYLINDRICAL_SURFACE('',#4621,5.99999999999999);
#4057=CYLINDRICAL_SURFACE('',#4625,7.);
#4058=CYLINDRICAL_SURFACE('',#4635,5.);
#4059=CYLINDRICAL_SURFACE('',#4641,4.49999999999996);
#4060=CYLINDRICAL_SURFACE('',#4643,5.62967641351579);
#4061=CYLINDRICAL_SURFACE('',#4648,4.9623029756639);
#4062=CYLINDRICAL_SURFACE('',#4656,5.62967641351579);
#4063=CYLINDRICAL_SURFACE('',#4660,4.49999999999996);
#4064=ADVANCED_FACE('',(#181),#3951,.T.);
#4065=ADVANCED_FACE('',(#182),#120,.F.);
#4066=ADVANCED_FACE('',(#183,#98),#121,.F.);
#4067=ADVANCED_FACE('',(#184),#122,.F.);
#4068=ADVANCED_FACE('',(#185,#99),#123,.F.);
#4069=ADVANCED_FACE('',(#186),#3952,.F.);
#4070=ADVANCED_FACE('',(#187),#3953,.T.);
#4071=ADVANCED_FACE('',(#188),#3954,.F.);
#4072=ADVANCED_FACE('',(#189),#3955,.T.);
#4073=ADVANCED_FACE('',(#190),#124,.F.);
#4074=ADVANCED_FACE('',(#191),#3956,.T.);
#4075=ADVANCED_FACE('',(#192),#3957,.F.);
#4076=ADVANCED_FACE('',(#193),#125,.F.);
#4077=ADVANCED_FACE('',(#194),#3958,.F.);
#4078=ADVANCED_FACE('',(#195),#126,.F.);
#4079=ADVANCED_FACE('',(#196),#3959,.F.);
#4080=ADVANCED_FACE('',(#197),#127,.F.);
#4081=ADVANCED_FACE('',(#198),#3960,.F.);
#4082=ADVANCED_FACE('',(#199),#128,.F.);
#4083=ADVANCED_FACE('',(#200),#3961,.F.);
#4084=ADVANCED_FACE('',(#201),#129,.F.);
#4085=ADVANCED_FACE('',(#202),#3962,.F.);
#4086=ADVANCED_FACE('',(#203),#3963,.T.);
#4087=ADVANCED_FACE('',(#204),#3964,.F.);
#4088=ADVANCED_FACE('',(#205),#3965,.F.);
#4089=ADVANCED_FACE('',(#206),#130,.F.);
#4090=ADVANCED_FACE('',(#207),#3966,.T.);
#4091=ADVANCED_FACE('',(#208),#131,.F.);
#4092=ADVANCED_FACE('',(#209),#3967,.T.);
#4093=ADVANCED_FACE('',(#210),#132,.F.);
#4094=ADVANCED_FACE('',(#211),#3968,.T.);
#4095=ADVANCED_FACE('',(#212),#133,.F.);
#4096=ADVANCED_FACE('',(#213,#100,#101),#134,.F.);
#4097=ADVANCED_FACE('',(#214,#102,#103),#135,.T.);
#4098=ADVANCED_FACE('',(#215),#3969,.T.);
#4099=ADVANCED_FACE('',(#216),#3970,.T.);
#4100=ADVANCED_FACE('',(#217),#3971,.T.);
#4101=ADVANCED_FACE('',(#218),#3972,.T.);
#4102=ADVANCED_FACE('',(#219),#3973,.T.);
#4103=ADVANCED_FACE('',(#220),#3974,.T.);
#4104=ADVANCED_FACE('',(#221),#3975,.T.);
#4105=ADVANCED_FACE('',(#222),#3976,.T.);
#4106=ADVANCED_FACE('',(#223),#3977,.T.);
#4107=ADVANCED_FACE('',(#224),#3978,.T.);
#4108=ADVANCED_FACE('',(#225),#3979,.T.);
#4109=ADVANCED_FACE('',(#226),#3980,.T.);
#4110=ADVANCED_FACE('',(#227),#3981,.T.);
#4111=ADVANCED_FACE('',(#228),#3982,.T.);
#4112=ADVANCED_FACE('',(#229),#3983,.T.);
#4113=ADVANCED_FACE('',(#230),#3984,.T.);
#4114=ADVANCED_FACE('',(#231),#136,.T.);
#4115=ADVANCED_FACE('',(#232),#3985,.F.);
#4116=ADVANCED_FACE('',(#233),#137,.F.);
#4117=ADVANCED_FACE('',(#234),#3986,.T.);
#4118=ADVANCED_FACE('',(#235),#3987,.T.);
#4119=ADVANCED_FACE('',(#236),#3988,.T.);
#4120=ADVANCED_FACE('',(#237),#3989,.T.);
#4121=ADVANCED_FACE('',(#238),#48,.T.);
#4122=ADVANCED_FACE('',(#239),#49,.T.);
#4123=ADVANCED_FACE('',(#240),#50,.T.);
#4124=ADVANCED_FACE('',(#241),#51,.T.);
#4125=ADVANCED_FACE('',(#242),#3990,.T.);
#4126=ADVANCED_FACE('',(#243),#3991,.T.);
#4127=ADVANCED_FACE('',(#244),#3992,.T.);
#4128=ADVANCED_FACE('',(#245),#3993,.T.);
#4129=ADVANCED_FACE('',(#246),#52,.T.);
#4130=ADVANCED_FACE('',(#247),#53,.T.);
#4131=ADVANCED_FACE('',(#248),#54,.T.);
#4132=ADVANCED_FACE('',(#249),#55,.T.);
#4133=ADVANCED_FACE('',(#250),#3994,.T.);
#4134=ADVANCED_FACE('',(#251),#3995,.T.);
#4135=ADVANCED_FACE('',(#252),#56,.T.);
#4136=ADVANCED_FACE('',(#253),#57,.T.);
#4137=ADVANCED_FACE('',(#254),#138,.T.);
#4138=ADVANCED_FACE('',(#255),#3996,.F.);
#4139=ADVANCED_FACE('',(#256),#3997,.F.);
#4140=ADVANCED_FACE('',(#257),#3998,.F.);
#4141=ADVANCED_FACE('',(#258),#3999,.F.);
#4142=ADVANCED_FACE('',(#259),#4000,.F.);
#4143=ADVANCED_FACE('',(#260),#4001,.F.);
#4144=ADVANCED_FACE('',(#261),#4002,.F.);
#4145=ADVANCED_FACE('',(#262),#4003,.F.);
#4146=ADVANCED_FACE('',(#263),#4004,.F.);
#4147=ADVANCED_FACE('',(#264),#4005,.F.);
#4148=ADVANCED_FACE('',(#265),#58,.T.);
#4149=ADVANCED_FACE('',(#266),#59,.T.);
#4150=ADVANCED_FACE('',(#267,#104),#139,.F.);
#4151=ADVANCED_FACE('',(#268),#140,.F.);
#4152=ADVANCED_FACE('',(#269),#141,.F.);
#4153=ADVANCED_FACE('',(#270),#142,.F.);
#4154=ADVANCED_FACE('',(#271),#143,.F.);
#4155=ADVANCED_FACE('',(#272),#144,.F.);
#4156=ADVANCED_FACE('',(#273),#145,.F.);
#4157=ADVANCED_FACE('',(#274,#105),#146,.T.);
#4158=ADVANCED_FACE('',(#275),#4006,.F.);
#4159=ADVANCED_FACE('',(#276),#4007,.T.);
#4160=ADVANCED_FACE('',(#277),#45,.T.);
#4161=ADVANCED_FACE('',(#278,#106),#147,.T.);
#4162=ADVANCED_FACE('',(#279,#107),#148,.T.);
#4163=ADVANCED_FACE('',(#280),#46,.T.);
#4164=ADVANCED_FACE('',(#281),#47,.T.);
#4165=ADVANCED_FACE('',(#282),#4008,.F.);
#4166=ADVANCED_FACE('',(#283),#4009,.F.);
#4167=ADVANCED_FACE('',(#284),#4010,.F.);
#4168=ADVANCED_FACE('',(#285),#4011,.F.);
#4169=ADVANCED_FACE('',(#286),#4012,.F.);
#4170=ADVANCED_FACE('',(#287),#4013,.F.);
#4171=ADVANCED_FACE('',(#288),#4014,.F.);
#4172=ADVANCED_FACE('',(#289),#4015,.F.);
#4173=ADVANCED_FACE('',(#290),#4016,.F.);
#4174=ADVANCED_FACE('',(#291),#4017,.F.);
#4175=ADVANCED_FACE('',(#292),#60,.F.);
#4176=ADVANCED_FACE('',(#293),#61,.F.);
#4177=ADVANCED_FACE('',(#294,#108),#149,.T.);
#4178=ADVANCED_FACE('',(#295),#150,.T.);
#4179=ADVANCED_FACE('',(#296),#151,.T.);
#4180=ADVANCED_FACE('',(#297),#152,.T.);
#4181=ADVANCED_FACE('',(#298),#153,.T.);
#4182=ADVANCED_FACE('',(#299),#154,.T.);
#4183=ADVANCED_FACE('',(#300),#155,.T.);
#4184=ADVANCED_FACE('',(#301,#109),#156,.F.);
#4185=ADVANCED_FACE('',(#302),#4018,.T.);
#4186=ADVANCED_FACE('',(#303),#4019,.T.);
#4187=ADVANCED_FACE('',(#304),#4020,.T.);
#4188=ADVANCED_FACE('',(#305),#4021,.T.);
#4189=ADVANCED_FACE('',(#306),#4022,.T.);
#4190=ADVANCED_FACE('',(#307),#4023,.T.);
#4191=ADVANCED_FACE('',(#308),#4024,.T.);
#4192=ADVANCED_FACE('',(#309),#4025,.T.);
#4193=ADVANCED_FACE('',(#310),#4026,.T.);
#4194=ADVANCED_FACE('',(#311),#4027,.T.);
#4195=ADVANCED_FACE('',(#312),#4028,.T.);
#4196=ADVANCED_FACE('',(#313),#4029,.T.);
#4197=ADVANCED_FACE('',(#314),#4030,.T.);
#4198=ADVANCED_FACE('',(#315),#4031,.T.);
#4199=ADVANCED_FACE('',(#316),#4032,.T.);
#4200=ADVANCED_FACE('',(#317),#4033,.T.);
#4201=ADVANCED_FACE('',(#318),#4034,.T.);
#4202=ADVANCED_FACE('',(#319),#4035,.T.);
#4203=ADVANCED_FACE('',(#320),#4036,.T.);
#4204=ADVANCED_FACE('',(#321),#4037,.T.);
#4205=ADVANCED_FACE('',(#322),#4038,.T.);
#4206=ADVANCED_FACE('',(#323),#4039,.T.);
#4207=ADVANCED_FACE('',(#324),#62,.F.);
#4208=ADVANCED_FACE('',(#325),#63,.F.);
#4209=ADVANCED_FACE('',(#326),#157,.F.);
#4210=ADVANCED_FACE('',(#327),#158,.T.);
#4211=ADVANCED_FACE('',(#328),#4040,.T.);
#4212=ADVANCED_FACE('',(#329),#159,.T.);
#4213=ADVANCED_FACE('',(#330,#110),#160,.T.);
#4214=ADVANCED_FACE('',(#331),#161,.T.);
#4215=ADVANCED_FACE('',(#332,#111),#162,.T.);
#4216=ADVANCED_FACE('',(#333),#4041,.F.);
#4217=ADVANCED_FACE('',(#334),#4042,.T.);
#4218=ADVANCED_FACE('',(#335),#4043,.F.);
#4219=ADVANCED_FACE('',(#336),#4044,.T.);
#4220=ADVANCED_FACE('',(#337),#163,.T.);
#4221=ADVANCED_FACE('',(#338),#4045,.T.);
#4222=ADVANCED_FACE('',(#339),#4046,.F.);
#4223=ADVANCED_FACE('',(#340),#164,.T.);
#4224=ADVANCED_FACE('',(#341),#4047,.F.);
#4225=ADVANCED_FACE('',(#342),#165,.T.);
#4226=ADVANCED_FACE('',(#343),#4048,.F.);
#4227=ADVANCED_FACE('',(#344),#166,.T.);
#4228=ADVANCED_FACE('',(#345),#4049,.F.);
#4229=ADVANCED_FACE('',(#346),#167,.T.);
#4230=ADVANCED_FACE('',(#347),#4050,.F.);
#4231=ADVANCED_FACE('',(#348),#168,.T.);
#4232=ADVANCED_FACE('',(#349),#4051,.F.);
#4233=ADVANCED_FACE('',(#350),#4052,.T.);
#4234=ADVANCED_FACE('',(#351),#4053,.F.);
#4235=ADVANCED_FACE('',(#352),#4054,.F.);
#4236=ADVANCED_FACE('',(#353),#169,.T.);
#4237=ADVANCED_FACE('',(#354),#4055,.T.);
#4238=ADVANCED_FACE('',(#355),#170,.T.);
#4239=ADVANCED_FACE('',(#356),#4056,.T.);
#4240=ADVANCED_FACE('',(#357),#171,.T.);
#4241=ADVANCED_FACE('',(#358),#4057,.T.);
#4242=ADVANCED_FACE('',(#359),#172,.T.);
#4243=ADVANCED_FACE('',(#360,#112,#113),#173,.T.);
#4244=ADVANCED_FACE('',(#361,#114,#115),#174,.F.);
#4245=ADVANCED_FACE('',(#362),#175,.T.);
#4246=ADVANCED_FACE('',(#363),#4058,.F.);
#4247=ADVANCED_FACE('',(#364),#176,.T.);
#4248=ADVANCED_FACE('',(#365,#116),#177,.F.);
#4249=ADVANCED_FACE('',(#366),#4059,.F.);
#4250=ADVANCED_FACE('',(#367),#4060,.T.);
#4251=ADVANCED_FACE('',(#368,#117),#43,.T.);
#4252=ADVANCED_FACE('',(#369),#4061,.T.);
#4253=ADVANCED_FACE('',(#370,#118),#44,.T.);
#4254=ADVANCED_FACE('',(#371),#4062,.T.);
#4255=ADVANCED_FACE('',(#372),#178,.F.);
#4256=ADVANCED_FACE('',(#373),#4063,.F.);
#4257=ADVANCED_FACE('',(#374,#119),#179,.T.);
#4258=ADVANCED_FACE('',(#375),#180,.F.);
#4259=CLOSED_SHELL('',(#4064,#4065,#4066,#4067,#4068,#4069,#4070,#4071,
#4072,#4073,#4074,#4075,#4076,#4077,#4078,#4079,#4080,#4081,#4082,#4083,
#4084,#4085,#4086,#4087,#4088,#4089,#4090,#4091,#4092,#4093,#4094,#4095,
#4096,#4097));
#4260=CLOSED_SHELL('',(#4098,#4099,#4100,#4101,#4102,#4103,#4104,#4105,
#4106,#4107,#4108,#4109,#4110,#4111,#4112,#4113,#4114,#4115,#4116,#4117,
#4118,#4119,#4120,#4121,#4122,#4123,#4124,#4125,#4126,#4127,#4128,#4129,
#4130,#4131,#4132,#4133,#4134,#4135,#4136,#4137));
#4261=CLOSED_SHELL('',(#4138,#4139,#4140,#4141,#4142,#4143,#4144,#4145,
#4146,#4147,#4148,#4149,#4150,#4151,#4152,#4153,#4154,#4155,#4156,#4157));
#4262=CLOSED_SHELL('',(#4158,#4159,#4160,#4161,#4162,#4163,#4164));
#4263=CLOSED_SHELL('',(#4165,#4166,#4167,#4168,#4169,#4170,#4171,#4172,
#4173,#4174,#4175,#4176,#4177,#4178,#4179,#4180,#4181,#4182,#4183,#4184));
#4264=CLOSED_SHELL('',(#4185,#4186,#4187,#4188,#4189,#4190,#4191,#4192,
#4193,#4194,#4195,#4196,#4197,#4198,#4199,#4200,#4201,#4202,#4203,#4204,
#4205,#4206,#4207,#4208,#4209,#4210));
#4265=CLOSED_SHELL('',(#4211,#4212,#4213,#4214,#4215,#4216,#4217,#4218,
#4219,#4220,#4221,#4222,#4223,#4224,#4225,#4226,#4227,#4228,#4229,#4230,
#4231,#4232,#4233,#4234,#4235,#4236,#4237,#4238,#4239,#4240,#4241,#4242,
#4243,#4244));
#4266=CLOSED_SHELL('',(#4245,#4246,#4247,#4248,#4249,#4250,#4251));
#4267=CLOSED_SHELL('',(#4252,#4253,#4254,#4255,#4256,#4257,#4258));
#4268=DERIVED_UNIT_ELEMENT(#4284,1.);
#4269=DERIVED_UNIT_ELEMENT(#51555,-3.);
#4270=DERIVED_UNIT_ELEMENT(#4284,1.);
#4271=DERIVED_UNIT_ELEMENT(#51555,-3.);
#4272=DERIVED_UNIT_ELEMENT(#4284,1.);
#4273=DERIVED_UNIT_ELEMENT(#51555,-3.);
#4274=DERIVED_UNIT_ELEMENT(#4284,1.);
#4275=DERIVED_UNIT_ELEMENT(#51555,-3.);
#4276=DERIVED_UNIT_ELEMENT(#4284,1.);
#4277=DERIVED_UNIT_ELEMENT(#51555,-3.);
#4278=DERIVED_UNIT_ELEMENT(#4284,1.);
#4279=DERIVED_UNIT_ELEMENT(#51555,-3.);
#4280=DERIVED_UNIT_ELEMENT(#4284,1.);
#4281=DERIVED_UNIT_ELEMENT(#51555,-3.);
#4282=DERIVED_UNIT_ELEMENT(#4284,1.);
#4283=DERIVED_UNIT_ELEMENT(#51555,-3.);
#4284=(
MASS_UNIT()
NAMED_UNIT(*)
SI_UNIT(.KILO.,.GRAM.)
);
#4285=DERIVED_UNIT((#4268,#4269));
#4286=DERIVED_UNIT((#4270,#4271));
#4287=DERIVED_UNIT((#4272,#4273));
#4288=DERIVED_UNIT((#4274,#4275));
#4289=DERIVED_UNIT((#4276,#4277));
#4290=DERIVED_UNIT((#4278,#4279));
#4291=DERIVED_UNIT((#4280,#4281));
#4292=DERIVED_UNIT((#4282,#4283));
#4293=MEASURE_REPRESENTATION_ITEM('density measure',
POSITIVE_RATIO_MEASURE(7850.),#4285);
#4294=MEASURE_REPRESENTATION_ITEM('density measure',
POSITIVE_RATIO_MEASURE(7850.),#4286);
#4295=MEASURE_REPRESENTATION_ITEM('density measure',
POSITIVE_RATIO_MEASURE(7850.),#4287);
#4296=MEASURE_REPRESENTATION_ITEM('density measure',
POSITIVE_RATIO_MEASURE(7850.),#4288);
#4297=MEASURE_REPRESENTATION_ITEM('density measure',
POSITIVE_RATIO_MEASURE(7850.),#4289);
#4298=MEASURE_REPRESENTATION_ITEM('density measure',
POSITIVE_RATIO_MEASURE(7850.),#4290);
#4299=MEASURE_REPRESENTATION_ITEM('density measure',
POSITIVE_RATIO_MEASURE(7850.),#4291);
#4300=MEASURE_REPRESENTATION_ITEM('density measure',
POSITIVE_RATIO_MEASURE(7850.),#4292);
#4301=PROPERTY_DEFINITION_REPRESENTATION(#4341,#4317);
#4302=PROPERTY_DEFINITION_REPRESENTATION(#4342,#4318);
#4303=PROPERTY_DEFINITION_REPRESENTATION(#4343,#4319);
#4304=PROPERTY_DEFINITION_REPRESENTATION(#4344,#4320);
#4305=PROPERTY_DEFINITION_REPRESENTATION(#4345,#4321);
#4306=PROPERTY_DEFINITION_REPRESENTATION(#4346,#4322);
#4307=PROPERTY_DEFINITION_REPRESENTATION(#4347,#4323);
#4308=PROPERTY_DEFINITION_REPRESENTATION(#4348,#4324);
#4309=PROPERTY_DEFINITION_REPRESENTATION(#4349,#4325);
#4310=PROPERTY_DEFINITION_REPRESENTATION(#4350,#4326);
#4311=PROPERTY_DEFINITION_REPRESENTATION(#4351,#4327);
#4312=PROPERTY_DEFINITION_REPRESENTATION(#4352,#4328);
#4313=PROPERTY_DEFINITION_REPRESENTATION(#4353,#4329);
#4314=PROPERTY_DEFINITION_REPRESENTATION(#4354,#4330);
#4315=PROPERTY_DEFINITION_REPRESENTATION(#4355,#4331);
#4316=PROPERTY_DEFINITION_REPRESENTATION(#4356,#4332);
#4317=REPRESENTATION('material name',(#4333),#51545);
#4318=REPRESENTATION('density',(#4293),#51545);
#4319=REPRESENTATION('material name',(#4334),#51546);
#4320=REPRESENTATION('density',(#4294),#51546);
#4321=REPRESENTATION('material name',(#4335),#51547);
#4322=REPRESENTATION('density',(#4295),#51547);
#4323=REPRESENTATION('material name',(#4336),#51548);
#4324=REPRESENTATION('density',(#4296),#51548);
#4325=REPRESENTATION('material name',(#4337),#51549);
#4326=REPRESENTATION('density',(#4297),#51549);
#4327=REPRESENTATION('material name',(#4338),#51550);
#4328=REPRESENTATION('density',(#4298),#51550);
#4329=REPRESENTATION('material name',(#4339),#51551);
#4330=REPRESENTATION('density',(#4299),#51551);
#4331=REPRESENTATION('material name',(#4340),#51552);
#4332=REPRESENTATION('density',(#4300),#51552);
#4333=DESCRIPTIVE_REPRESENTATION_ITEM('Steel','Steel');
#4334=DESCRIPTIVE_REPRESENTATION_ITEM('Steel','Steel');
#4335=DESCRIPTIVE_REPRESENTATION_ITEM('Steel','Steel');
#4336=DESCRIPTIVE_REPRESENTATION_ITEM('Steel','Steel');
#4337=DESCRIPTIVE_REPRESENTATION_ITEM('Steel','Steel');
#4338=DESCRIPTIVE_REPRESENTATION_ITEM('Steel','Steel');
#4339=DESCRIPTIVE_REPRESENTATION_ITEM('Steel','Steel');
#4340=DESCRIPTIVE_REPRESENTATION_ITEM('Steel','Steel');
#4341=PROPERTY_DEFINITION('material property','material name',#51595);
#4342=PROPERTY_DEFINITION('material property','density of part',#51595);
#4343=PROPERTY_DEFINITION('material property','material name',#51596);
#4344=PROPERTY_DEFINITION('material property','density of part',#51596);
#4345=PROPERTY_DEFINITION('material property','material name',#51597);
#4346=PROPERTY_DEFINITION('material property','density of part',#51597);
#4347=PROPERTY_DEFINITION('material property','material name',#51598);
#4348=PROPERTY_DEFINITION('material property','density of part',#51598);
#4349=PROPERTY_DEFINITION('material property','material name',#51599);
#4350=PROPERTY_DEFINITION('material property','density of part',#51599);
#4351=PROPERTY_DEFINITION('material property','material name',#51600);
#4352=PROPERTY_DEFINITION('material property','density of part',#51600);
#4353=PROPERTY_DEFINITION('material property','material name',#51601);
#4354=PROPERTY_DEFINITION('material property','density of part',#51601);
#4355=PROPERTY_DEFINITION('material property','material name',#51602);
#4356=PROPERTY_DEFINITION('material property','density of part',#51602);
#4357=AXIS2_PLACEMENT_3D('',#5527,#4671,#4672);
#4358=AXIS2_PLACEMENT_3D('',#5528,#4673,#4674);
#4359=AXIS2_PLACEMENT_3D('',#5529,#4675,#4676);
#4360=AXIS2_PLACEMENT_3D('',#5539,#4678,#4679);
#4361=AXIS2_PLACEMENT_3D('',#5543,#4681,#4682);
#4362=AXIS2_PLACEMENT_3D('',#5546,#4684,#4685);
#4363=AXIS2_PLACEMENT_3D('',#5547,#4686,#4687);
#4364=AXIS2_PLACEMENT_3D('',#5555,#4691,#4692);
#4365=AXIS2_PLACEMENT_3D('',#5557,#4694,#4695);
#4366=AXIS2_PLACEMENT_3D('',#5563,#4698,#4699);
#4367=AXIS2_PLACEMENT_3D('',#5565,#4700,#4701);
#4368=AXIS2_PLACEMENT_3D('',#5567,#4702,#4703);
#4369=AXIS2_PLACEMENT_3D('',#5571,#4705,#4706);
#4370=AXIS2_PLACEMENT_3D('',#5574,#4708,#4709);
#4371=AXIS2_PLACEMENT_3D('',#5575,#4710,#4711);
#4372=AXIS2_PLACEMENT_3D('',#5579,#4714,#4715);
#4373=AXIS2_PLACEMENT_3D('',#5581,#4716,#4717);
#4374=AXIS2_PLACEMENT_3D('',#5585,#4719,#4720);
#4375=AXIS2_PLACEMENT_3D('',#5587,#4721,#4722);
#4376=AXIS2_PLACEMENT_3D('',#5589,#4723,#4724);
#4377=AXIS2_PLACEMENT_3D('',#5592,#4726,#4727);
#4378=AXIS2_PLACEMENT_3D('',#5593,#4728,#4729);
#4379=AXIS2_PLACEMENT_3D('',#5595,#4730,#4731);
#4380=AXIS2_PLACEMENT_3D('',#5597,#4733,#4734);
#4381=AXIS2_PLACEMENT_3D('',#5600,#4737,#4738);
#4382=AXIS2_PLACEMENT_3D('',#5602,#4740,#4741);
#4383=AXIS2_PLACEMENT_3D('',#5604,#4743,#4744);
#4384=AXIS2_PLACEMENT_3D('',#5606,#4746,#4747);
#4385=AXIS2_PLACEMENT_3D('',#5607,#4748,#4749);
#4386=AXIS2_PLACEMENT_3D('',#5609,#4751,#4752);
#4387=AXIS2_PLACEMENT_3D('',#5613,#4755,#4756);
#4388=AXIS2_PLACEMENT_3D('',#5615,#4757,#4758);
#4389=AXIS2_PLACEMENT_3D('',#5618,#4760,#4761);
#4390=AXIS2_PLACEMENT_3D('',#5619,#4762,#4763);
#4391=AXIS2_PLACEMENT_3D('',#5628,#4768,#4769);
#4392=AXIS2_PLACEMENT_3D('',#5630,#4770,#4771);
#4393=AXIS2_PLACEMENT_3D('',#5633,#4773,#4774);
#4394=AXIS2_PLACEMENT_3D('',#5634,#4775,#4776);
#4395=AXIS2_PLACEMENT_3D('',#5640,#4780,#4781);
#4396=AXIS2_PLACEMENT_3D('',#5642,#4782,#4783);
#4397=AXIS2_PLACEMENT_3D('',#5645,#4785,#4786);
#4398=AXIS2_PLACEMENT_3D('',#5646,#4787,#4788);
#4399=AXIS2_PLACEMENT_3D('',#5652,#4792,#4793);
#4400=AXIS2_PLACEMENT_3D('',#5654,#4794,#4795);
#4401=AXIS2_PLACEMENT_3D('',#5657,#4797,#4798);
#4402=AXIS2_PLACEMENT_3D('',#5658,#4799,#4800);
#4403=AXIS2_PLACEMENT_3D('',#5664,#4804,#4805);
#4404=AXIS2_PLACEMENT_3D('',#5665,#4806,#4807);
#4405=AXIS2_PLACEMENT_3D('',#5666,#4808,#4809);
#4406=AXIS2_PLACEMENT_3D('',#5667,#4810,#4811);
#4407=AXIS2_PLACEMENT_3D('',#5670,#4812,#4813);
#4408=AXIS2_PLACEMENT_3D('',#5674,#4815,#4816);
#4409=AXIS2_PLACEMENT_3D('',#5676,#4818,#4819);
#4410=AXIS2_PLACEMENT_3D('',#5677,#4820,#4821);
#4411=AXIS2_PLACEMENT_3D('',#5678,#4822,#4823);
#4412=AXIS2_PLACEMENT_3D('',#5679,#4824,#4825);
#4413=AXIS2_PLACEMENT_3D('',#5681,#4826,#4827);
#4414=AXIS2_PLACEMENT_3D('',#5684,#4829,#4830);
#4415=AXIS2_PLACEMENT_3D('',#5685,#4831,#4832);
#4416=AXIS2_PLACEMENT_3D('',#5691,#4836,#4837);
#4417=AXIS2_PLACEMENT_3D('',#5693,#4838,#4839);
#4418=AXIS2_PLACEMENT_3D('',#5696,#4841,#4842);
#4419=AXIS2_PLACEMENT_3D('',#5697,#4843,#4844);
#4420=AXIS2_PLACEMENT_3D('',#5703,#4848,#4849);
#4421=AXIS2_PLACEMENT_3D('',#5705,#4850,#4851);
#4422=AXIS2_PLACEMENT_3D('',#5708,#4853,#4854);
#4423=AXIS2_PLACEMENT_3D('',#5709,#4855,#4856);
#4424=AXIS2_PLACEMENT_3D('',#5715,#4860,#4861);
#4425=AXIS2_PLACEMENT_3D('',#5717,#4862,#4863);
#4426=AXIS2_PLACEMENT_3D('',#5720,#4865,#4866);
#4427=AXIS2_PLACEMENT_3D('',#5721,#4867,#4868);
#4428=AXIS2_PLACEMENT_3D('',#5724,#4871,#4872);
#4429=AXIS2_PLACEMENT_3D('',#5725,#4873,#4874);
#4430=AXIS2_PLACEMENT_3D('',#5726,#4875,#4876);
#4431=AXIS2_PLACEMENT_3D('',#5727,#4877,#4878);
#4432=AXIS2_PLACEMENT_3D('',#5764,#4880,#4881);
#4433=AXIS2_PLACEMENT_3D('',#5859,#4882,#4883);
#4434=AXIS2_PLACEMENT_3D('',#6293,#4885,#4886);
#4435=AXIS2_PLACEMENT_3D('',#6703,#4888,#4889);
#4436=AXIS2_PLACEMENT_3D('',#7180,#4891,#4892);
#4437=AXIS2_PLACEMENT_3D('',#7715,#4894,#4895);
#4438=AXIS2_PLACEMENT_3D('',#8147,#4897,#4898);
#4439=AXIS2_PLACEMENT_3D('',#8596,#4900,#4901);
#4440=AXIS2_PLACEMENT_3D('',#9056,#4903,#4904);
#4441=AXIS2_PLACEMENT_3D('',#9515,#4906,#4907);
#4442=AXIS2_PLACEMENT_3D('',#9943,#4909,#4910);
#4443=AXIS2_PLACEMENT_3D('',#10386,#4912,#4913);
#4444=AXIS2_PLACEMENT_3D('',#10837,#4915,#4916);
#4445=AXIS2_PLACEMENT_3D('',#11293,#4918,#4919);
#4446=AXIS2_PLACEMENT_3D('',#11750,#4921,#4922);
#4447=AXIS2_PLACEMENT_3D('',#12289,#4924,#4925);
#4448=AXIS2_PLACEMENT_3D('',#12746,#4927,#4928);
#4449=AXIS2_PLACEMENT_3D('',#12758,#4929,#4930);
#4450=AXIS2_PLACEMENT_3D('',#12881,#4944,#4945);
#4451=AXIS2_PLACEMENT_3D('',#12982,#4946,#4947);
#4452=AXIS2_PLACEMENT_3D('',#12994,#4948,#4949);
#4453=AXIS2_PLACEMENT_3D('',#13085,#4950,#4951);
#4454=AXIS2_PLACEMENT_3D('',#13090,#4952,#4953);
#4455=AXIS2_PLACEMENT_3D('',#15199,#4954,#4955);
#4456=AXIS2_PLACEMENT_3D('',#17487,#4956,#4957);
#4457=AXIS2_PLACEMENT_3D('',#17805,#4958,#4959);
#4458=AXIS2_PLACEMENT_3D('',#17822,#4960,#4961);
#4459=AXIS2_PLACEMENT_3D('',#20880,#4962,#4963);
#4460=AXIS2_PLACEMENT_3D('',#21087,#4964,#4965);
#4461=AXIS2_PLACEMENT_3D('',#21258,#4966,#4967);
#4462=AXIS2_PLACEMENT_3D('',#21411,#4968,#4969);
#4463=AXIS2_PLACEMENT_3D('',#23902,#4970,#4971);
#4464=AXIS2_PLACEMENT_3D('',#23944,#4972,#4973);
#4465=AXIS2_PLACEMENT_3D('',#25099,#4974,#4975);
#4466=AXIS2_PLACEMENT_3D('',#25100,#4976,#4977);
#4467=AXIS2_PLACEMENT_3D('',#25101,#4978,#4979);
#4468=AXIS2_PLACEMENT_3D('',#25112,#4981,#4982);
#4469=AXIS2_PLACEMENT_3D('',#25117,#4983,#4984);
#4470=AXIS2_PLACEMENT_3D('',#25338,#4986,#4987);
#4471=AXIS2_PLACEMENT_3D('',#25760,#4989,#4990);
#4472=AXIS2_PLACEMENT_3D('',#25833,#4992,#4993);
#4473=AXIS2_PLACEMENT_3D('',#26043,#4995,#4996);
#4474=AXIS2_PLACEMENT_3D('',#26132,#4997,#4998);
#4475=AXIS2_PLACEMENT_3D('',#26480,#5000,#5001);
#4476=AXIS2_PLACEMENT_3D('',#26835,#5003,#5004);
#4477=AXIS2_PLACEMENT_3D('',#27184,#5006,#5007);
#4478=AXIS2_PLACEMENT_3D('',#27229,#5008,#5009);
#4479=AXIS2_PLACEMENT_3D('',#27240,#5010,#5011);
#4480=AXIS2_PLACEMENT_3D('',#27420,#5012,#5013);
#4481=AXIS2_PLACEMENT_3D('',#28046,#5014,#5015);
#4482=AXIS2_PLACEMENT_3D('',#28059,#5022,#5023);
#4483=AXIS2_PLACEMENT_3D('',#28065,#5027,#5028);
#4484=AXIS2_PLACEMENT_3D('',#28069,#5031,#5032);
#4485=AXIS2_PLACEMENT_3D('',#28073,#5035,#5036);
#4486=AXIS2_PLACEMENT_3D('',#28077,#5039,#5040);
#4487=AXIS2_PLACEMENT_3D('',#28081,#5043,#5044);
#4488=AXIS2_PLACEMENT_3D('',#28083,#5046,#5047);
#4489=AXIS2_PLACEMENT_3D('',#28084,#5048,#5049);
#4490=AXIS2_PLACEMENT_3D('',#28085,#5050,#5051);
#4491=AXIS2_PLACEMENT_3D('',#28087,#5052,#5053);
#4492=AXIS2_PLACEMENT_3D('',#28090,#5055,#5056);
#4493=AXIS2_PLACEMENT_3D('',#28091,#5057,#5058);
#4494=AXIS2_PLACEMENT_3D('',#28093,#5059,#5060);
#4495=AXIS2_PLACEMENT_3D('',#28096,#5062,#5063);
#4496=AXIS2_PLACEMENT_3D('',#28097,#5064,#5065);
#4497=AXIS2_PLACEMENT_3D('',#28099,#5066,#5067);
#4498=AXIS2_PLACEMENT_3D('',#28100,#5068,#5069);
#4499=AXIS2_PLACEMENT_3D('',#28101,#5070,#5071);
#4500=AXIS2_PLACEMENT_3D('',#28102,#5072,#5073);
#4501=AXIS2_PLACEMENT_3D('',#28104,#5074,#5075);
#4502=AXIS2_PLACEMENT_3D('',#28105,#5076,#5077);
#4503=AXIS2_PLACEMENT_3D('',#28107,#5078,#5079);
#4504=AXIS2_PLACEMENT_3D('',#28108,#5080,#5081);
#4505=AXIS2_PLACEMENT_3D('',#28109,#5082,#5083);
#4506=AXIS2_PLACEMENT_3D('',#28110,#5084,#5085);
#4507=AXIS2_PLACEMENT_3D('',#28111,#5086,#5087);
#4508=AXIS2_PLACEMENT_3D('',#28112,#5088,#5089);
#4509=AXIS2_PLACEMENT_3D('',#28124,#5091,#5092);
#4510=AXIS2_PLACEMENT_3D('',#28222,#5093,#5094);
#4511=AXIS2_PLACEMENT_3D('',#28594,#5096,#5097);
#4512=AXIS2_PLACEMENT_3D('',#29039,#5099,#5100);
#4513=AXIS2_PLACEMENT_3D('',#29171,#5102,#5103);
#4514=AXIS2_PLACEMENT_3D('',#29319,#5104,#5105);
#4515=AXIS2_PLACEMENT_3D('',#29411,#5107,#5108);
#4516=AXIS2_PLACEMENT_3D('',#29500,#5109,#5110);
#4517=AXIS2_PLACEMENT_3D('',#29853,#5112,#5113);
#4518=AXIS2_PLACEMENT_3D('',#30203,#5115,#5116);
#4519=AXIS2_PLACEMENT_3D('',#30276,#5118,#5119);
#4520=AXIS2_PLACEMENT_3D('',#30401,#5120,#5121);
#4521=AXIS2_PLACEMENT_3D('',#30784,#5122,#5123);
#4522=AXIS2_PLACEMENT_3D('',#31861,#5124,#5125);
#4523=AXIS2_PLACEMENT_3D('',#31874,#5132,#5133);
#4524=AXIS2_PLACEMENT_3D('',#31880,#5137,#5138);
#4525=AXIS2_PLACEMENT_3D('',#31884,#5141,#5142);
#4526=AXIS2_PLACEMENT_3D('',#31888,#5145,#5146);
#4527=AXIS2_PLACEMENT_3D('',#31892,#5149,#5150);
#4528=AXIS2_PLACEMENT_3D('',#31896,#5153,#5154);
#4529=AXIS2_PLACEMENT_3D('',#31898,#5156,#5157);
#4530=AXIS2_PLACEMENT_3D('',#31899,#5158,#5159);
#4531=AXIS2_PLACEMENT_3D('',#31900,#5160,#5161);
#4532=AXIS2_PLACEMENT_3D('',#32015,#5163,#5164);
#4533=AXIS2_PLACEMENT_3D('',#32092,#5165,#5166);
#4534=AXIS2_PLACEMENT_3D('',#32524,#5168,#5169);
#4535=AXIS2_PLACEMENT_3D('',#32993,#5171,#5172);
#4536=AXIS2_PLACEMENT_3D('',#33436,#5174,#5175);
#4537=AXIS2_PLACEMENT_3D('',#33895,#5177,#5178);
#4538=AXIS2_PLACEMENT_3D('',#34346,#5180,#5181);
#4539=AXIS2_PLACEMENT_3D('',#34781,#5183,#5184);
#4540=AXIS2_PLACEMENT_3D('',#35228,#5186,#5187);
#4541=AXIS2_PLACEMENT_3D('',#35663,#5189,#5190);
#4542=AXIS2_PLACEMENT_3D('',#36106,#5192,#5193);
#4543=AXIS2_PLACEMENT_3D('',#36547,#5195,#5196);
#4544=AXIS2_PLACEMENT_3D('',#37010,#5198,#5199);
#4545=AXIS2_PLACEMENT_3D('',#37481,#5201,#5202);
#4546=AXIS2_PLACEMENT_3D('',#37924,#5204,#5205);
#4547=AXIS2_PLACEMENT_3D('',#38367,#5207,#5208);
#4548=AXIS2_PLACEMENT_3D('',#38834,#5210,#5211);
#4549=AXIS2_PLACEMENT_3D('',#39295,#5213,#5214);
#4550=AXIS2_PLACEMENT_3D('',#39734,#5216,#5217);
#4551=AXIS2_PLACEMENT_3D('',#40178,#5219,#5220);
#4552=AXIS2_PLACEMENT_3D('',#40617,#5222,#5223);
#4553=AXIS2_PLACEMENT_3D('',#40694,#5224,#5225);
#4554=AXIS2_PLACEMENT_3D('',#45218,#5226,#5227);
#4555=AXIS2_PLACEMENT_3D('',#49543,#5228,#5229);
#4556=AXIS2_PLACEMENT_3D('',#49708,#5230,#5231);
#4557=AXIS2_PLACEMENT_3D('',#51249,#5232,#5233);
#4558=AXIS2_PLACEMENT_3D('',#51250,#5234,#5235);
#4559=AXIS2_PLACEMENT_3D('',#51251,#5236,#5237);
#4560=AXIS2_PLACEMENT_3D('',#51252,#5238,#5239);
#4561=AXIS2_PLACEMENT_3D('',#51255,#5240,#5241);
#4562=AXIS2_PLACEMENT_3D('',#51259,#5243,#5244);
#4563=AXIS2_PLACEMENT_3D('',#51263,#5246,#5247);
#4564=AXIS2_PLACEMENT_3D('',#51270,#5249,#5250);
#4565=AXIS2_PLACEMENT_3D('',#51274,#5252,#5253);
#4566=AXIS2_PLACEMENT_3D('',#51280,#5257,#5258);
#4567=AXIS2_PLACEMENT_3D('',#51284,#5260,#5261);
#4568=AXIS2_PLACEMENT_3D('',#51288,#5263,#5264);
#4569=AXIS2_PLACEMENT_3D('',#51290,#5265,#5266);
#4570=AXIS2_PLACEMENT_3D('',#51292,#5267,#5268);
#4571=AXIS2_PLACEMENT_3D('',#51297,#5271,#5272);
#4572=AXIS2_PLACEMENT_3D('',#51298,#5273,#5274);
#4573=AXIS2_PLACEMENT_3D('',#51302,#5277,#5278);
#4574=AXIS2_PLACEMENT_3D('',#51306,#5280,#5281);
#4575=AXIS2_PLACEMENT_3D('',#51308,#5282,#5283);
#4576=AXIS2_PLACEMENT_3D('',#51310,#5284,#5285);
#4577=AXIS2_PLACEMENT_3D('',#51313,#5287,#5288);
#4578=AXIS2_PLACEMENT_3D('',#51315,#5289,#5290);
#4579=AXIS2_PLACEMENT_3D('',#51316,#5291,#5292);
#4580=AXIS2_PLACEMENT_3D('',#51318,#5293,#5294);
#4581=AXIS2_PLACEMENT_3D('',#51320,#5296,#5297);
#4582=AXIS2_PLACEMENT_3D('',#51323,#5300,#5301);
#4583=AXIS2_PLACEMENT_3D('',#51325,#5303,#5304);
#4584=AXIS2_PLACEMENT_3D('',#51327,#5306,#5307);
#4585=AXIS2_PLACEMENT_3D('',#51329,#5309,#5310);
#4586=AXIS2_PLACEMENT_3D('',#51330,#5311,#5312);
#4587=AXIS2_PLACEMENT_3D('',#51332,#5314,#5315);
#4588=AXIS2_PLACEMENT_3D('',#51336,#5318,#5319);
#4589=AXIS2_PLACEMENT_3D('',#51338,#5320,#5321);
#4590=AXIS2_PLACEMENT_3D('',#51341,#5323,#5324);
#4591=AXIS2_PLACEMENT_3D('',#51342,#5325,#5326);
#4592=AXIS2_PLACEMENT_3D('',#51351,#5331,#5332);
#4593=AXIS2_PLACEMENT_3D('',#51353,#5333,#5334);
#4594=AXIS2_PLACEMENT_3D('',#51355,#5335,#5336);
#4595=AXIS2_PLACEMENT_3D('',#51357,#5338,#5339);
#4596=AXIS2_PLACEMENT_3D('',#51363,#5343,#5344);
#4597=AXIS2_PLACEMENT_3D('',#51365,#5345,#5346);
#4598=AXIS2_PLACEMENT_3D('',#51367,#5347,#5348);
#4599=AXIS2_PLACEMENT_3D('',#51369,#5350,#5351);
#4600=AXIS2_PLACEMENT_3D('',#51375,#5355,#5356);
#4601=AXIS2_PLACEMENT_3D('',#51377,#5357,#5358);
#4602=AXIS2_PLACEMENT_3D('',#51379,#5359,#5360);
#4603=AXIS2_PLACEMENT_3D('',#51381,#5362,#5363);
#4604=AXIS2_PLACEMENT_3D('',#51387,#5367,#5368);
#4605=AXIS2_PLACEMENT_3D('',#51388,#5369,#5370);
#4606=AXIS2_PLACEMENT_3D('',#51389,#5371,#5372);
#4607=AXIS2_PLACEMENT_3D('',#51390,#5373,#5374);
#4608=AXIS2_PLACEMENT_3D('',#51393,#5375,#5376);
#4609=AXIS2_PLACEMENT_3D('',#51397,#5378,#5379);
#4610=AXIS2_PLACEMENT_3D('',#51399,#5381,#5382);
#4611=AXIS2_PLACEMENT_3D('',#51400,#5383,#5384);
#4612=AXIS2_PLACEMENT_3D('',#51401,#5385,#5386);
#4613=AXIS2_PLACEMENT_3D('',#51402,#5387,#5388);
#4614=AXIS2_PLACEMENT_3D('',#51404,#5389,#5390);
#4615=AXIS2_PLACEMENT_3D('',#51406,#5391,#5392);
#4616=AXIS2_PLACEMENT_3D('',#51408,#5394,#5395);
#4617=AXIS2_PLACEMENT_3D('',#51414,#5399,#5400);
#4618=AXIS2_PLACEMENT_3D('',#51416,#5401,#5402);
#4619=AXIS2_PLACEMENT_3D('',#51418,#5403,#5404);
#4620=AXIS2_PLACEMENT_3D('',#51420,#5406,#5407);
#4621=AXIS2_PLACEMENT_3D('',#51426,#5411,#5412);
#4622=AXIS2_PLACEMENT_3D('',#51428,#5413,#5414);
#4623=AXIS2_PLACEMENT_3D('',#51430,#5415,#5416);
#4624=AXIS2_PLACEMENT_3D('',#51432,#5418,#5419);
#4625=AXIS2_PLACEMENT_3D('',#51438,#5423,#5424);
#4626=AXIS2_PLACEMENT_3D('',#51440,#5425,#5426);
#4627=AXIS2_PLACEMENT_3D('',#51442,#5427,#5428);
#4628=AXIS2_PLACEMENT_3D('',#51444,#5430,#5431);
#4629=AXIS2_PLACEMENT_3D('',#51447,#5434,#5435);
#4630=AXIS2_PLACEMENT_3D('',#51448,#5436,#5437);
#4631=AXIS2_PLACEMENT_3D('',#51449,#5438,#5439);
#4632=AXIS2_PLACEMENT_3D('',#51450,#5440,#5441);
#4633=AXIS2_PLACEMENT_3D('',#51455,#5443,#5444);
#4634=AXIS2_PLACEMENT_3D('',#51457,#5445,#5446);
#4635=AXIS2_PLACEMENT_3D('',#51461,#5449,#5450);
#4636=AXIS2_PLACEMENT_3D('',#51463,#5451,#5452);
#4637=AXIS2_PLACEMENT_3D('',#51482,#5454,#5455);
#4638=AXIS2_PLACEMENT_3D('',#51483,#5456,#5457);
#4639=AXIS2_PLACEMENT_3D('',#51484,#5458,#5459);
#4640=AXIS2_PLACEMENT_3D('',#51486,#5460,#5461);
#4641=AXIS2_PLACEMENT_3D('',#51487,#5462,#5463);
#4642=AXIS2_PLACEMENT_3D('',#51489,#5464,#5465);
#4643=AXIS2_PLACEMENT_3D('',#51491,#5467,#5468);
#4644=AXIS2_PLACEMENT_3D('',#51495,#5470,#5471);
#4645=AXIS2_PLACEMENT_3D('',#51496,#5472,#5473);
#4646=AXIS2_PLACEMENT_3D('',#51497,#5474,#5475);
#4647=AXIS2_PLACEMENT_3D('',#51499,#5476,#5477);
#4648=AXIS2_PLACEMENT_3D('',#51500,#5478,#5479);
#4649=AXIS2_PLACEMENT_3D('',#51502,#5480,#5481);
#4650=AXIS2_PLACEMENT_3D('',#51505,#5483,#5484);
#4651=AXIS2_PLACEMENT_3D('',#51506,#5485,#5486);
#4652=AXIS2_PLACEMENT_3D('',#51509,#5487,#5488);
#4653=AXIS2_PLACEMENT_3D('',#51510,#5489,#5490);
#4654=AXIS2_PLACEMENT_3D('',#51512,#5491,#5492);
#4655=AXIS2_PLACEMENT_3D('',#51514,#5493,#5494);
#4656=AXIS2_PLACEMENT_3D('',#51515,#5495,#5496);
#4657=AXIS2_PLACEMENT_3D('',#51518,#5498,#5499);
#4658=AXIS2_PLACEMENT_3D('',#51519,#5500,#5501);
#4659=AXIS2_PLACEMENT_3D('',#51521,#5502,#5503);
#4660=AXIS2_PLACEMENT_3D('',#51522,#5504,#5505);
#4661=AXIS2_PLACEMENT_3D('',#51524,#5507,#5508);
#4662=AXIS2_PLACEMENT_3D('',#51525,#5509,#5510);
#4663=AXIS2_PLACEMENT_3D('',#51526,#5511,#5512);
#4664=AXIS2_PLACEMENT_3D('',#51527,#5513,#5514);
#4665=AXIS2_PLACEMENT_3D('',#51528,#5515,#5516);
#4666=AXIS2_PLACEMENT_3D('',#51529,#5517,#5518);
#4667=AXIS2_PLACEMENT_3D('',#51530,#5519,#5520);
#4668=AXIS2_PLACEMENT_3D('',#51531,#5521,#5522);
#4669=AXIS2_PLACEMENT_3D('',#51532,#5523,#5524);
#4670=AXIS2_PLACEMENT_3D('',#51533,#5525,#5526);
#4671=DIRECTION('axis',(0.,0.,1.));
#4672=DIRECTION('refdir',(1.,0.,0.));
#4673=DIRECTION('axis',(0.,0.,1.));
#4674=DIRECTION('refdir',(1.,0.,0.));
#4675=DIRECTION('center_axis',(-1.,-1.22464679914735E-16,2.71926214689378E-32));
#4676=DIRECTION('ref_axis',(-8.65956056235492E-17,0.707106781186548,-0.707106781186547));
#4677=DIRECTION('',(-1.,-1.22464679914735E-16,2.71926214689378E-32));
#4678=DIRECTION('center_axis',(1.,1.22464679914735E-16,-2.71926214689378E-32));
#4679=DIRECTION('ref_axis',(-8.65956056235492E-17,0.707106781186548,-0.707106781186547));
#4680=DIRECTION('',(-1.,-1.22464679914735E-16,2.71926214689378E-32));
#4681=DIRECTION('center_axis',(1.,1.22464679914734E-16,-4.44089209850062E-15));
#4682=DIRECTION('ref_axis',(-3.22678052299109E-15,0.707106781186548,-0.707106781186547));
#4683=DIRECTION('',(1.,1.22464679914735E-16,-2.71926214689378E-32));
#4684=DIRECTION('center_axis',(-1.,-1.22464679914735E-16,6.9563080245457E-32));
#4685=DIRECTION('ref_axis',(-8.65956056235492E-17,0.707106781186548,-0.707106781186547));
#4686=DIRECTION('center_axis',(-1.,-1.22464679914735E-16,2.71926214689378E-32));
#4687=DIRECTION('ref_axis',(-8.75811540203011E-47,-2.22044604925031E-16,
-1.));
#4688=DIRECTION('',(0.,-2.22044604925031E-16,-1.));
#4689=DIRECTION('',(1.22464679914735E-16,-1.,2.22044604925031E-16));
#4690=DIRECTION('',(0.,-2.22044604925031E-16,-1.));
#4691=DIRECTION('center_axis',(-1.,-1.22464679914735E-16,2.71926214689378E-32));
#4692=DIRECTION('ref_axis',(-8.65956056235493E-17,0.707106781186549,-0.707106781186547));
#4693=DIRECTION('',(1.22464679914735E-16,-1.,2.22044604925031E-16));
#4694=DIRECTION('center_axis',(0.,-2.22044604925031E-16,-1.));
#4695=DIRECTION('ref_axis',(1.,1.22464679914735E-16,-2.71926214689377E-32));
#4696=DIRECTION('',(-1.,-1.22464679914735E-16,2.71926214689378E-32));
#4697=DIRECTION('',(1.22464679914735E-16,-1.,2.22044604925031E-16));
#4698=DIRECTION('center_axis',(0.,2.22044604925031E-16,1.));
#4699=DIRECTION('ref_axis',(-0.785839144811216,-0.61843094883938,1.37319255708452E-16));
#4700=DIRECTION('center_axis',(0.,2.22044604925031E-16,1.));
#4701=DIRECTION('ref_axis',(0.126759996397889,0.991933416774134,-2.20253463639549E-16));
#4702=DIRECTION('center_axis',(0.,2.22044604925031E-16,1.));
#4703=DIRECTION('ref_axis',(-1.22464679914735E-16,1.,-2.22044604925031E-16));
#4704=DIRECTION('',(1.,1.22464679914735E-16,-2.71926214689378E-32));
#4705=DIRECTION('center_axis',(0.,2.22044604925031E-16,1.));
#4706=DIRECTION('ref_axis',(0.707106781186548,-0.707106781186547,1.57009245868377E-16));
#4707=DIRECTION('',(-1.22464679914735E-16,1.,-2.22044604925031E-16));
#4708=DIRECTION('center_axis',(0.,2.22044604925031E-16,1.));
#4709=DIRECTION('ref_axis',(1.,1.22464679914735E-16,-2.71926214689377E-32));
#4710=DIRECTION('center_axis',(-1.,-1.22464679914734E-16,4.44089209850062E-15));
#4711=DIRECTION('ref_axis',(-4.44089209850062E-15,-2.22044604925032E-16,
-1.));
#4712=DIRECTION('',(-4.44089209850062E-15,-2.22044604925032E-16,-1.));
#4713=DIRECTION('',(1.22464679914735E-16,-1.,2.22044604925031E-16));
#4714=DIRECTION('center_axis',(0.,2.22044604925031E-16,1.));
#4715=DIRECTION('ref_axis',(-1.,-1.22464679914735E-16,2.71926214689377E-32));
#4716=DIRECTION('center_axis',(0.,-2.22044604925031E-16,-1.));
#4717=DIRECTION('ref_axis',(0.707106781186548,-0.707106781186547,1.57009245868377E-16));
#4718=DIRECTION('',(-1.,-1.22464679914735E-16,2.71926214689378E-32));
#4719=DIRECTION('center_axis',(0.,-2.22044604925031E-16,-1.));
#4720=DIRECTION('ref_axis',(-1.22464679914735E-16,1.,-2.22044604925031E-16));
#4721=DIRECTION('center_axis',(0.,-2.22044604925031E-16,-1.));
#4722=DIRECTION('ref_axis',(0.126759996397889,0.991933416774134,-2.20253463639549E-16));
#4723=DIRECTION('center_axis',(0.,-2.22044604925031E-16,-1.));
#4724=DIRECTION('ref_axis',(-0.785839144811216,-0.61843094883938,1.37319255708452E-16));
#4725=DIRECTION('',(-1.22464679914735E-16,1.,-2.22044604925031E-16));
#4726=DIRECTION('center_axis',(0.,-2.22044604925031E-16,-1.));
#4727=DIRECTION('ref_axis',(1.,1.22464679914735E-16,-2.71926214689377E-32));
#4728=DIRECTION('center_axis',(1.,1.22464679914735E-16,-2.71926214689378E-32));
#4729=DIRECTION('ref_axis',(-8.65956056235493E-17,0.707106781186549,-0.707106781186547));
#4730=DIRECTION('center_axis',(1.,1.22464679914735E-16,-6.9563080245457E-32));
#4731=DIRECTION('ref_axis',(-8.65956056235493E-17,0.707106781186549,-0.707106781186547));
#4732=DIRECTION('',(1.,1.22464679914735E-16,-2.71926214689378E-32));
#4733=DIRECTION('center_axis',(0.,2.22044604925031E-16,1.));
#4734=DIRECTION('ref_axis',(-0.785839144811216,-0.61843094883938,1.37319255708452E-16));
#4735=DIRECTION('',(0.,-2.22044604925031E-16,-1.));
#4736=DIRECTION('',(4.23704587765192E-32,2.22044604925031E-16,1.));
#4737=DIRECTION('center_axis',(0.,2.22044604925031E-16,1.));
#4738=DIRECTION('ref_axis',(0.126759996397889,0.991933416774134,-2.20253463639549E-16));
#4739=DIRECTION('',(0.,2.22044604925031E-16,1.));
#4740=DIRECTION('center_axis',(4.44089209850062E-15,2.22044604925032E-16,
1.));
#4741=DIRECTION('ref_axis',(0.707106781186548,-0.707106781186547,-2.98317567149917E-15));
#4742=DIRECTION('',(4.44089209850062E-15,2.22044604925032E-16,1.));
#4743=DIRECTION('center_axis',(-1.22464679914735E-16,1.,-2.22044604925031E-16));
#4744=DIRECTION('ref_axis',(1.,1.22464679914735E-16,-2.71926214689378E-32));
#4745=DIRECTION('',(0.,-2.22044604925031E-16,-1.));
#4746=DIRECTION('center_axis',(0.,-2.22044604925031E-16,-1.));
#4747=DIRECTION('ref_axis',(-1.22464679914735E-16,1.,-2.22044604925031E-16));
#4748=DIRECTION('center_axis',(0.,2.22044604925031E-16,1.));
#4749=DIRECTION('ref_axis',(1.,1.22464679914735E-16,-2.71926214689377E-32));
#4750=DIRECTION('',(0.,2.22044604925031E-16,1.));
#4751=DIRECTION('center_axis',(1.,1.22464679914735E-16,-6.9563080245457E-32));
#4752=DIRECTION('ref_axis',(4.23704587765193E-32,2.22044604925031E-16,1.));
#4753=DIRECTION('',(-4.23704587765192E-32,-2.22044604925031E-16,-1.));
#4754=DIRECTION('',(1.22464679914735E-16,-1.,2.22044604925031E-16));
#4755=DIRECTION('center_axis',(-1.22464679914735E-16,1.,-2.22044604925031E-16));
#4756=DIRECTION('ref_axis',(1.,1.22464679914735E-16,-2.71926214689378E-32));
#4757=DIRECTION('center_axis',(1.22464679914735E-16,-1.,2.22044604925031E-16));
#4758=DIRECTION('ref_axis',(1.,1.22464679914735E-16,-2.71926214689378E-32));
#4759=DIRECTION('',(-1.22464679914735E-16,1.,-2.22044604925031E-16));
#4760=DIRECTION('center_axis',(1.22464679914735E-16,-1.,2.22044604925031E-16));
#4761=DIRECTION('ref_axis',(1.,1.22464679914735E-16,-2.71926214689378E-32));
#4762=DIRECTION('center_axis',(1.,1.22464679914735E-16,-2.71926214689378E-32));
#4763=DIRECTION('ref_axis',(8.75811540203011E-47,2.22044604925031E-16,1.));
#4764=DIRECTION('',(0.,2.22044604925031E-16,1.));
#4765=DIRECTION('',(1.22464679914735E-16,-1.,2.22044604925031E-16));
#4766=DIRECTION('',(0.,2.22044604925031E-16,1.));
#4767=DIRECTION('',(1.22464679914735E-16,-1.,2.22044604925031E-16));
#4768=DIRECTION('center_axis',(-1.22464679914735E-16,1.,-2.22044604925031E-16));
#4769=DIRECTION('ref_axis',(1.,1.22464679914735E-16,2.77555756156289E-16));
#4770=DIRECTION('center_axis',(1.22464679914735E-16,-1.,2.22044604925031E-16));
#4771=DIRECTION('ref_axis',(1.,1.22464679914735E-16,2.77555756156289E-16));
#4772=DIRECTION('',(1.22464679914735E-16,-1.,2.22044604925031E-16));
#4773=DIRECTION('center_axis',(1.22464679914735E-16,-1.,2.22044604925031E-16));
#4774=DIRECTION('ref_axis',(1.,1.22464679914735E-16,2.77555756156289E-16));
#4775=DIRECTION('center_axis',(1.29472072842584E-15,-2.22044604925031E-16,
-1.));
#4776=DIRECTION('ref_axis',(1.,1.22464679914736E-16,1.29472072842584E-15));
#4777=DIRECTION('',(1.,1.22464679914736E-16,1.29472072842584E-15));
#4778=DIRECTION('',(1.22464679914735E-16,-1.,2.22044604925031E-16));
#4779=DIRECTION('',(1.,1.22464679914736E-16,1.29472072842584E-15));
#4780=DIRECTION('center_axis',(-1.22464679914735E-16,1.,-2.22044604925031E-16));
#4781=DIRECTION('ref_axis',(2.08890553820447E-48,-2.22044604925031E-16,
-1.));
#4782=DIRECTION('center_axis',(1.22464679914735E-16,-1.,2.22044604925031E-16));
#4783=DIRECTION('ref_axis',(2.08890553820447E-48,-2.22044604925031E-16,
-1.));
#4784=DIRECTION('',(1.22464679914735E-16,-1.,2.22044604925031E-16));
#4785=DIRECTION('center_axis',(1.22464679914735E-16,-1.,2.22044604925031E-16));
#4786=DIRECTION('ref_axis',(2.08890553820447E-48,-2.22044604925031E-16,
-1.));
#4787=DIRECTION('center_axis',(-1.,-1.22464679914735E-16,2.71926214689378E-32));
#4788=DIRECTION('ref_axis',(-8.75811540203011E-47,-2.22044604925031E-16,
-1.));
#4789=DIRECTION('',(0.,-2.22044604925031E-16,-1.));
#4790=DIRECTION('',(1.22464679914735E-16,-1.,2.22044604925031E-16));
#4791=DIRECTION('',(0.,-2.22044604925031E-16,-1.));
#4792=DIRECTION('center_axis',(-1.22464679914735E-16,1.,-2.22044604925031E-16));
#4793=DIRECTION('ref_axis',(-1.,-1.22464679914735E-16,1.66533453693773E-15));
#4794=DIRECTION('center_axis',(1.22464679914735E-16,-1.,2.22044604925031E-16));
#4795=DIRECTION('ref_axis',(-1.,-1.22464679914735E-16,1.66533453693773E-15));
#4796=DIRECTION('',(1.22464679914735E-16,-1.,2.22044604925031E-16));
#4797=DIRECTION('center_axis',(1.22464679914735E-16,-1.,2.22044604925031E-16));
#4798=DIRECTION('ref_axis',(-1.,-1.22464679914735E-16,1.66533453693773E-15));
#4799=DIRECTION('center_axis',(8.09200455266149E-16,2.22044604925031E-16,
1.));
#4800=DIRECTION('ref_axis',(-1.,-1.22464679914735E-16,8.09200455266149E-16));
#4801=DIRECTION('',(-1.,-1.22464679914735E-16,8.09200455266149E-16));
#4802=DIRECTION('',(1.22464679914735E-16,-1.,2.22044604925031E-16));
#4803=DIRECTION('',(-1.,-1.22464679914735E-16,8.09200455266149E-16));
#4804=DIRECTION('center_axis',(-1.22464679914735E-16,1.,-2.22044604925031E-16));
#4805=DIRECTION('ref_axis',(2.22044604925031E-15,2.22044604925031E-16,1.));
#4806=DIRECTION('center_axis',(1.22464679914735E-16,-1.,2.22044604925031E-16));
#4807=DIRECTION('ref_axis',(2.22044604925031E-15,2.22044604925031E-16,1.));
#4808=DIRECTION('center_axis',(1.22464679914735E-16,-1.,2.22044604925031E-16));
#4809=DIRECTION('ref_axis',(2.22044604925031E-15,2.22044604925031E-16,1.));
#4810=DIRECTION('center_axis',(-1.22464679914735E-16,1.,-2.22044604925031E-16));
#4811=DIRECTION('ref_axis',(1.58603289232165E-16,-2.22044604925031E-16,
-1.));
#4812=DIRECTION('center_axis',(-1.22464679914735E-16,1.,-2.22044604925031E-16));
#4813=DIRECTION('ref_axis',(1.58603289232165E-16,-2.22044604925031E-16,
-1.));
#4814=DIRECTION('',(1.22464679914735E-16,-1.,2.22044604925031E-16));
#4815=DIRECTION('center_axis',(-1.22464679914735E-16,1.,-2.22044604925031E-16));
#4816=DIRECTION('ref_axis',(1.58603289232165E-16,-2.22044604925031E-16,
-1.));
#4817=DIRECTION('',(1.22464679914735E-16,-1.,2.22044604925031E-16));
#4818=DIRECTION('center_axis',(-1.22464679914735E-16,1.,-2.22044604925031E-16));
#4819=DIRECTION('ref_axis',(0.559779357098146,2.52548619278702E-16,0.828641702647644));
#4820=DIRECTION('center_axis',(1.22464679914735E-16,-1.,2.22044604925031E-16));
#4821=DIRECTION('ref_axis',(0.559779357098146,2.52548619278702E-16,0.828641702647644));
#4822=DIRECTION('center_axis',(-1.22464679914735E-16,1.,-2.22044604925031E-16));
#4823=DIRECTION('ref_axis',(0.559779357098146,2.52548619278702E-16,0.828641702647644));
#4824=DIRECTION('center_axis',(-1.22464679914735E-16,1.,-2.22044604925031E-16));
#4825=DIRECTION('ref_axis',(-1.,-1.22464679914735E-16,2.71926214689378E-32));
#4826=DIRECTION('center_axis',(-1.22464679914735E-16,1.,-2.22044604925031E-16));
#4827=DIRECTION('ref_axis',(-1.,-1.22464679914735E-16,2.71926214689378E-32));
#4828=DIRECTION('',(1.22464679914735E-16,-1.,2.22044604925031E-16));
#4829=DIRECTION('center_axis',(1.22464679914735E-16,-1.,2.22044604925031E-16));
#4830=DIRECTION('ref_axis',(-1.,-1.22464679914735E-16,2.71926214689378E-32));
#4831=DIRECTION('center_axis',(-1.90049007730895E-14,-2.22044604925034E-16,
-1.));
#4832=DIRECTION('ref_axis',(1.,1.22464679914731E-16,-1.90049007730895E-14));
#4833=DIRECTION('',(1.,1.22464679914731E-16,-1.90049007730895E-14));
#4834=DIRECTION('',(1.22464679914735E-16,-1.,2.22044604925031E-16));
#4835=DIRECTION('',(1.,1.22464679914731E-16,-1.90049007730895E-14));
#4836=DIRECTION('center_axis',(-1.22464679914735E-16,1.,-2.22044604925031E-16));
#4837=DIRECTION('ref_axis',(1.,1.22464679914735E-16,-2.71926214689378E-32));
#4838=DIRECTION('center_axis',(-1.22464679914735E-16,1.,-2.22044604925031E-16));
#4839=DIRECTION('ref_axis',(1.,1.22464679914735E-16,-2.71926214689378E-32));
#4840=DIRECTION('',(1.22464679914735E-16,-1.,2.22044604925031E-16));
#4841=DIRECTION('center_axis',(-1.22464679914735E-16,1.,-2.22044604925031E-16));
#4842=DIRECTION('ref_axis',(1.,1.22464679914735E-16,-2.71926214689378E-32));
#4843=DIRECTION('center_axis',(-1.,-1.22464679914735E-16,2.71926214689378E-32));
#4844=DIRECTION('ref_axis',(-8.75811540203011E-47,-2.22044604925031E-16,
-1.));
#4845=DIRECTION('',(0.,-2.22044604925031E-16,-1.));
#4846=DIRECTION('',(1.22464679914735E-16,-1.,2.22044604925031E-16));
#4847=DIRECTION('',(0.,-2.22044604925031E-16,-1.));
#4848=DIRECTION('center_axis',(-1.22464679914735E-16,1.,-2.22044604925031E-16));
#4849=DIRECTION('ref_axis',(-1.48029736616688E-15,2.22044604925031E-16,
1.));
#4850=DIRECTION('center_axis',(-1.22464679914735E-16,1.,-2.22044604925031E-16));
#4851=DIRECTION('ref_axis',(-1.48029736616688E-15,2.22044604925031E-16,
1.));
#4852=DIRECTION('',(1.22464679914735E-16,-1.,2.22044604925031E-16));
#4853=DIRECTION('center_axis',(-1.22464679914735E-16,1.,-2.22044604925031E-16));
#4854=DIRECTION('ref_axis',(-1.48029736616688E-15,2.22044604925031E-16,
1.));
#4855=DIRECTION('center_axis',(0.,-2.22044604925031E-16,-1.));
#4856=DIRECTION('ref_axis',(1.,1.22464679914735E-16,-2.71926214689377E-32));
#4857=DIRECTION('',(1.,1.22464679914735E-16,-2.71926214689378E-32));
#4858=DIRECTION('',(1.22464679914735E-16,-1.,2.22044604925031E-16));
#4859=DIRECTION('',(1.,1.22464679914735E-16,-2.71926214689378E-32));
#4860=DIRECTION('center_axis',(-1.22464679914735E-16,1.,-2.22044604925031E-16));
#4861=DIRECTION('ref_axis',(-1.,-1.22464679914735E-16,2.71926214689378E-32));
#4862=DIRECTION('center_axis',(-1.22464679914735E-16,1.,-2.22044604925031E-16));
#4863=DIRECTION('ref_axis',(-1.,-1.22464679914735E-16,2.71926214689378E-32));
#4864=DIRECTION('',(1.22464679914735E-16,-1.,2.22044604925031E-16));
#4865=DIRECTION('center_axis',(-1.22464679914735E-16,1.,-2.22044604925031E-16));
#4866=DIRECTION('ref_axis',(-1.,-1.22464679914735E-16,2.71926214689378E-32));
#4867=DIRECTION('center_axis',(1.,1.22464679914735E-16,-1.44006500428221E-15));
#4868=DIRECTION('ref_axis',(1.44006500428221E-15,2.22044604925031E-16,1.));
#4869=DIRECTION('',(1.44006500428221E-15,2.22044604925031E-16,1.));
#4870=DIRECTION('',(1.44006500428221E-15,2.22044604925031E-16,1.));
#4871=DIRECTION('center_axis',(-1.22464679914735E-16,1.,-2.22044604925031E-16));
#4872=DIRECTION('ref_axis',(1.,1.22464679914735E-16,-2.71926214689378E-32));
#4873=DIRECTION('center_axis',(-1.22464679914735E-16,1.,-2.22044604925031E-16));
#4874=DIRECTION('ref_axis',(1.,1.22464679914735E-16,-2.71926214689378E-32));
#4875=DIRECTION('axis',(0.,0.,1.));
#4876=DIRECTION('refdir',(1.,0.,0.));
#4877=DIRECTION('center_axis',(0.,-2.22044604925031E-16,-1.));
#4878=DIRECTION('ref_axis',(-1.,1.08690987399046E-13,-2.41342473559327E-29));
#4879=DIRECTION('',(0.,2.22044604925031E-16,1.));
#4880=DIRECTION('center_axis',(0.,-2.22044604925031E-16,-1.));
#4881=DIRECTION('ref_axis',(-1.,1.08690987399046E-13,-2.41342473559327E-29));
#4882=DIRECTION('center_axis',(0.,-2.22044604925031E-16,-1.));
#4883=DIRECTION('ref_axis',(-1.,1.08690987399046E-13,-2.41342473559327E-29));
#4884=DIRECTION('',(0.,2.22044604925031E-16,1.));
#4885=DIRECTION('center_axis',(0.,-2.22044604925031E-16,-1.));
#4886=DIRECTION('ref_axis',(-1.,1.08690987399046E-13,-2.41342473559327E-29));
#4887=DIRECTION('',(0.,2.22044604925031E-16,1.));
#4888=DIRECTION('center_axis',(0.,-2.22044604925031E-16,-1.));
#4889=DIRECTION('ref_axis',(-1.,1.08690987399046E-13,-2.41342473559327E-29));
#4890=DIRECTION('',(0.,2.22044604925031E-16,1.));
#4891=DIRECTION('center_axis',(0.,-2.22044604925031E-16,-1.));
#4892=DIRECTION('ref_axis',(-1.,1.08690987399046E-13,-2.41342473559327E-29));
#4893=DIRECTION('',(0.,2.22044604925031E-16,1.));
#4894=DIRECTION('center_axis',(0.,-2.22044604925031E-16,-1.));
#4895=DIRECTION('ref_axis',(-1.,1.08690987399046E-13,-2.41342473559327E-29));
#4896=DIRECTION('',(0.,2.22044604925031E-16,1.));
#4897=DIRECTION('center_axis',(0.,-2.22044604925031E-16,-1.));
#4898=DIRECTION('ref_axis',(-1.,1.08690987399046E-13,-2.41342473559327E-29));
#4899=DIRECTION('',(0.,2.22044604925031E-16,1.));
#4900=DIRECTION('center_axis',(0.,-2.22044604925031E-16,-1.));
#4901=DIRECTION('ref_axis',(-1.,1.08690987399046E-13,-2.41342473559327E-29));
#4902=DIRECTION('',(0.,2.22044604925031E-16,1.));
#4903=DIRECTION('center_axis',(0.,-2.22044604925031E-16,-1.));
#4904=DIRECTION('ref_axis',(-1.,1.08690987399046E-13,-2.41342473559327E-29));
#4905=DIRECTION('',(0.,2.22044604925031E-16,1.));
#4906=DIRECTION('center_axis',(0.,-2.22044604925031E-16,-1.));
#4907=DIRECTION('ref_axis',(-1.,1.08690987399046E-13,-2.41342473559327E-29));
#4908=DIRECTION('',(0.,2.22044604925031E-16,1.));
#4909=DIRECTION('center_axis',(0.,-2.22044604925031E-16,-1.));
#4910=DIRECTION('ref_axis',(-1.,1.08690987399046E-13,-2.41342473559327E-29));
#4911=DIRECTION('',(0.,2.22044604925031E-16,1.));
#4912=DIRECTION('center_axis',(0.,-2.22044604925031E-16,-1.));
#4913=DIRECTION('ref_axis',(-1.,1.08690987399046E-13,-2.41342473559327E-29));
#4914=DIRECTION('',(0.,2.22044604925031E-16,1.));
#4915=DIRECTION('center_axis',(0.,-2.22044604925031E-16,-1.));
#4916=DIRECTION('ref_axis',(-1.,1.08690987399046E-13,-2.41342473559327E-29));
#4917=DIRECTION('',(0.,2.22044604925031E-16,1.));
#4918=DIRECTION('center_axis',(0.,-2.22044604925031E-16,-1.));
#4919=DIRECTION('ref_axis',(-1.,1.08690987399046E-13,-2.41342473559327E-29));
#4920=DIRECTION('',(0.,2.22044604925031E-16,1.));
#4921=DIRECTION('center_axis',(0.,-2.22044604925031E-16,-1.));
#4922=DIRECTION('ref_axis',(-1.,1.08690987399046E-13,-2.41342473559327E-29));
#4923=DIRECTION('',(0.,2.22044604925031E-16,1.));
#4924=DIRECTION('center_axis',(0.,-2.22044604925031E-16,-1.));
#4925=DIRECTION('ref_axis',(-1.,1.08690987399046E-13,-2.41342473559327E-29));
#4926=DIRECTION('',(0.,2.22044604925031E-16,1.));
#4927=DIRECTION('center_axis',(1.,0.,0.));
#4928=DIRECTION('ref_axis',(0.,1.,0.));
#4929=DIRECTION('center_axis',(-1.,0.,0.));
#4930=DIRECTION('ref_axis',(0.,1.,0.));
#4931=DIRECTION('',(0.,2.22044604925031E-16,1.));
#4932=DIRECTION('',(0.,2.22044604925031E-16,1.));
#4933=DIRECTION('',(0.,2.22044604925031E-16,1.));
#4934=DIRECTION('',(0.,2.22044604925031E-16,1.));
#4935=DIRECTION('',(0.,2.22044604925031E-16,1.));
#4936=DIRECTION('',(0.,2.22044604925031E-16,1.));
#4937=DIRECTION('',(0.,-1.,2.22044604925031E-16));
#4938=DIRECTION('',(0.,-2.22044604925031E-16,-1.));
#4939=DIRECTION('',(0.,-2.22044604925031E-16,-1.));
#4940=DIRECTION('',(0.,-2.22044604925031E-16,-1.));
#4941=DIRECTION('',(0.,-2.22044604925031E-16,-1.));
#4942=DIRECTION('',(0.,-2.22044604925031E-16,-1.));
#4943=DIRECTION('',(0.,-2.22044604925031E-16,-1.));
#4944=DIRECTION('center_axis',(-1.,0.,0.));
#4945=DIRECTION('ref_axis',(0.,1.,0.));
#4946=DIRECTION('center_axis',(0.,2.22044604925031E-16,1.));
#4947=DIRECTION('ref_axis',(-1.,0.,0.));
#4948=DIRECTION('center_axis',(0.,2.22044604925031E-16,1.));
#4949=DIRECTION('ref_axis',(-1.,1.08690987399046E-13,-2.41342473559327E-29));
#4950=DIRECTION('center_axis',(0.,-2.22044604925031E-16,-1.));
#4951=DIRECTION('ref_axis',(-1.,0.,0.));
#4952=DIRECTION('center_axis',(0.,-2.22044604925031E-16,-1.));
#4953=DIRECTION('ref_axis',(-1.,0.,0.));
#4954=DIRECTION('center_axis',(0.,-2.22044604925031E-16,-1.));
#4955=DIRECTION('ref_axis',(-1.,0.,0.));
#4956=DIRECTION('center_axis',(0.,-2.22044604925031E-16,-1.));
#4957=DIRECTION('ref_axis',(-1.,0.,0.));
#4958=DIRECTION('center_axis',(0.,-2.22044604925031E-16,-1.));
#4959=DIRECTION('ref_axis',(-1.,0.,0.));
#4960=DIRECTION('center_axis',(0.,-2.22044604925031E-16,-1.));
#4961=DIRECTION('ref_axis',(-1.,0.,0.));
#4962=DIRECTION('center_axis',(0.,-2.22044604925031E-16,-1.));
#4963=DIRECTION('ref_axis',(-1.,1.08690987399046E-13,-2.41342473559327E-29));
#4964=DIRECTION('center_axis',(0.,-2.22044604925031E-16,-1.));
#4965=DIRECTION('ref_axis',(-1.,1.08690987399046E-13,-2.41342473559327E-29));
#4966=DIRECTION('center_axis',(0.,-2.22044604925031E-16,-1.));
#4967=DIRECTION('ref_axis',(-1.,1.08690987399046E-13,-2.41342473559327E-29));
#4968=DIRECTION('center_axis',(0.,-2.22044604925031E-16,-1.));
#4969=DIRECTION('ref_axis',(-1.,1.08690987399046E-13,-2.41342473559327E-29));
#4970=DIRECTION('center_axis',(0.,-2.22044604925031E-16,-1.));
#4971=DIRECTION('ref_axis',(-1.,0.,0.));
#4972=DIRECTION('center_axis',(0.,-2.22044604925031E-16,-1.));
#4973=DIRECTION('ref_axis',(-1.,1.08690987399046E-13,-2.41342473559327E-29));
#4974=DIRECTION('center_axis',(0.,2.22044604925031E-16,1.));
#4975=DIRECTION('ref_axis',(-1.,0.,0.));
#4976=DIRECTION('axis',(0.,0.,1.));
#4977=DIRECTION('refdir',(1.,0.,0.));
#4978=DIRECTION('center_axis',(0.,-2.22044604925031E-16,-1.));
#4979=DIRECTION('ref_axis',(-0.793396157953295,-0.608705623881487,1.35159799770409E-16));
#4980=DIRECTION('',(0.,-2.22044604925031E-16,-1.));
#4981=DIRECTION('center_axis',(0.,-2.22044604925031E-16,-1.));
#4982=DIRECTION('ref_axis',(-1.,3.91712146416972E-15,-8.69775687954924E-31));
#4983=DIRECTION('center_axis',(0.,-2.22044604925031E-16,-1.));
#4984=DIRECTION('ref_axis',(-0.793396157953295,-0.608705623881487,1.35159799770409E-16));
#4985=DIRECTION('',(0.,-2.22044604925031E-16,-1.));
#4986=DIRECTION('center_axis',(0.,-2.22044604925031E-16,-1.));
#4987=DIRECTION('ref_axis',(-0.793396157953295,-0.608705623881487,1.35159799770409E-16));
#4988=DIRECTION('',(0.,-2.22044604925031E-16,-1.));
#4989=DIRECTION('center_axis',(0.,-2.22044604925031E-16,-1.));
#4990=DIRECTION('ref_axis',(-0.793396157953295,-0.608705623881487,1.35159799770409E-16));
#4991=DIRECTION('',(0.,-2.22044604925031E-16,-1.));
#4992=DIRECTION('center_axis',(0.,-2.22044604925031E-16,-1.));
#4993=DIRECTION('ref_axis',(-0.862028396347557,0.506859984503077,-1.12545525011293E-16));
#4994=DIRECTION('',(0.,-2.22044604925031E-16,-1.));
#4995=DIRECTION('center_axis',(0.,2.22044604925031E-16,1.));
#4996=DIRECTION('ref_axis',(-1.,0.,0.));
#4997=DIRECTION('center_axis',(0.,-2.22044604925031E-16,-1.));
#4998=DIRECTION('ref_axis',(-0.937789548385183,0.34720420927678,-7.70948214771704E-17));
#4999=DIRECTION('',(0.,-2.22044604925031E-16,-1.));
#5000=DIRECTION('center_axis',(0.,-2.22044604925031E-16,-1.));
#5001=DIRECTION('ref_axis',(-0.937789548385183,0.34720420927678,-7.70948214771704E-17));
#5002=DIRECTION('',(0.,-2.22044604925031E-16,-1.));
#5003=DIRECTION('center_axis',(0.,-2.22044604925031E-16,-1.));
#5004=DIRECTION('ref_axis',(-0.937789548385183,0.34720420927678,-7.70948214771704E-17));
#5005=DIRECTION('',(0.,-2.22044604925031E-16,-1.));
#5006=DIRECTION('center_axis',(0.,-2.22044604925031E-16,-1.));
#5007=DIRECTION('ref_axis',(-0.937789548385183,0.34720420927678,-7.70948214771704E-17));
#5008=DIRECTION('center_axis',(0.,2.22044604925031E-16,1.));
#5009=DIRECTION('ref_axis',(-1.,0.,0.));
#5010=DIRECTION('center_axis',(0.,-2.22044604925031E-16,-1.));
#5011=DIRECTION('ref_axis',(-0.793396157953295,-0.608705623881487,1.35159799770409E-16));
#5012=DIRECTION('center_axis',(0.,2.22044604925031E-16,1.));
#5013=DIRECTION('ref_axis',(-1.,3.91712146416972E-15,-8.69775687954924E-31));
#5014=DIRECTION('center_axis',(0.,2.22044604925031E-16,1.));
#5015=DIRECTION('ref_axis',(-1.,0.,0.));
#5016=DIRECTION('',(0.,-1.,2.22044604925031E-16));
#5017=DIRECTION('',(-0.866025403784439,-0.5,1.11022302462516E-16));
#5018=DIRECTION('',(-0.866025403784439,0.5,-1.11022302462516E-16));
#5019=DIRECTION('',(0.,1.,-2.22044604925031E-16));
#5020=DIRECTION('',(0.866025403784439,0.5,-1.11022302462516E-16));
#5021=DIRECTION('',(0.866025403784439,-0.5,1.11022302462516E-16));
#5022=DIRECTION('center_axis',(0.5,0.866025403784439,-1.92296268638356E-16));
#5023=DIRECTION('ref_axis',(-0.866025403784439,0.5,-1.11022302462516E-16));
#5024=DIRECTION('',(0.,2.22044604925031E-16,1.));
#5025=DIRECTION('',(-0.866025403784439,0.5,-1.11022302462516E-16));
#5026=DIRECTION('',(0.,2.22044604925031E-16,1.));
#5027=DIRECTION('center_axis',(-0.5,0.866025403784439,-1.92296268638356E-16));
#5028=DIRECTION('ref_axis',(-0.866025403784439,-0.5,1.11022302462516E-16));
#5029=DIRECTION('',(0.,2.22044604925031E-16,1.));
#5030=DIRECTION('',(-0.866025403784439,-0.5,1.11022302462516E-16));
#5031=DIRECTION('center_axis',(-1.,0.,0.));
#5032=DIRECTION('ref_axis',(0.,-1.,2.22044604925031E-16));
#5033=DIRECTION('',(0.,2.22044604925031E-16,1.));
#5034=DIRECTION('',(0.,-1.,2.22044604925031E-16));
#5035=DIRECTION('center_axis',(-0.5,-0.866025403784439,1.92296268638356E-16));
#5036=DIRECTION('ref_axis',(0.866025403784439,-0.5,1.11022302462516E-16));
#5037=DIRECTION('',(0.,2.22044604925031E-16,1.));
#5038=DIRECTION('',(0.866025403784439,-0.5,1.11022302462516E-16));
#5039=DIRECTION('center_axis',(0.5,-0.866025403784439,1.92296268638356E-16));
#5040=DIRECTION('ref_axis',(0.866025403784439,0.5,-1.11022302462516E-16));
#5041=DIRECTION('',(0.,2.22044604925031E-16,1.));
#5042=DIRECTION('',(0.866025403784439,0.5,-1.11022302462516E-16));
#5043=DIRECTION('center_axis',(1.,0.,0.));
#5044=DIRECTION('ref_axis',(0.,1.,-2.22044604925031E-16));
#5045=DIRECTION('',(0.,1.,-2.22044604925031E-16));
#5046=DIRECTION('center_axis',(0.,2.22044604925031E-16,1.));
#5047=DIRECTION('ref_axis',(-1.,0.,0.));
#5048=DIRECTION('axis',(0.,0.,1.));
#5049=DIRECTION('refdir',(1.,0.,0.));
#5050=DIRECTION('center_axis',(-1.,0.,0.));
#5051=DIRECTION('ref_axis',(0.,1.,0.));
#5052=DIRECTION('center_axis',(-1.,0.,0.));
#5053=DIRECTION('ref_axis',(0.,1.,0.));
#5054=DIRECTION('',(-1.,0.,0.));
#5055=DIRECTION('center_axis',(1.,0.,0.));
#5056=DIRECTION('ref_axis',(0.,1.,0.));
#5057=DIRECTION('center_axis',(1.,0.,0.));
#5058=DIRECTION('ref_axis',(0.,0.,-1.));
#5059=DIRECTION('center_axis',(1.,0.,0.));
#5060=DIRECTION('ref_axis',(0.,0.,-1.));
#5061=DIRECTION('',(-1.,0.,0.));
#5062=DIRECTION('center_axis',(1.,0.,0.));
#5063=DIRECTION('ref_axis',(0.,0.,-1.));
#5064=DIRECTION('center_axis',(1.,0.,0.));
#5065=DIRECTION('ref_axis',(0.,0.,-1.));
#5066=DIRECTION('center_axis',(1.,0.,0.));
#5067=DIRECTION('ref_axis',(0.,0.,-1.));
#5068=DIRECTION('center_axis',(0.,-1.,-1.22464679914735E-16));
#5069=DIRECTION('ref_axis',(0.,-1.22464679914735E-16,1.));
#5070=DIRECTION('center_axis',(1.,0.,0.));
#5071=DIRECTION('ref_axis',(0.,0.,-1.));
#5072=DIRECTION('center_axis',(-1.,0.,0.));
#5073=DIRECTION('ref_axis',(0.,0.,1.));
#5074=DIRECTION('center_axis',(1.,0.,0.));
#5075=DIRECTION('ref_axis',(0.,0.,-1.));
#5076=DIRECTION('center_axis',(1.,0.,0.));
#5077=DIRECTION('ref_axis',(0.,0.,-1.));
#5078=DIRECTION('center_axis',(1.,0.,0.));
#5079=DIRECTION('ref_axis',(0.,0.,-1.));
#5080=DIRECTION('center_axis',(0.,-1.,-1.22464679914735E-16));
#5081=DIRECTION('ref_axis',(0.,-1.22464679914735E-16,1.));
#5082=DIRECTION('center_axis',(1.,0.,0.));
#5083=DIRECTION('ref_axis',(0.,0.,-1.));
#5084=DIRECTION('center_axis',(0.,-1.,-1.22464679914735E-16));
#5085=DIRECTION('ref_axis',(0.,-1.22464679914735E-16,1.));
#5086=DIRECTION('axis',(0.,0.,1.));
#5087=DIRECTION('refdir',(1.,0.,0.));
#5088=DIRECTION('center_axis',(0.,-1.,0.));
#5089=DIRECTION('ref_axis',(-0.608635263423501,0.,0.793450134613011));
#5090=DIRECTION('',(0.,-1.,0.));
#5091=DIRECTION('center_axis',(0.,1.,0.));
#5092=DIRECTION('ref_axis',(1.,0.,3.91712146416972E-15));
#5093=DIRECTION('center_axis',(0.,-1.,0.));
#5094=DIRECTION('ref_axis',(-0.608635263423501,0.,0.793450134613011));
#5095=DIRECTION('',(0.,-1.,0.));
#5096=DIRECTION('center_axis',(0.,-1.,0.));
#5097=DIRECTION('ref_axis',(-0.608635263423501,0.,0.793450134613011));
#5098=DIRECTION('',(0.,-1.,0.));
#5099=DIRECTION('center_axis',(0.,-1.,0.));
#5100=DIRECTION('ref_axis',(-0.608635263423501,0.,0.793450134613011));
#5101=DIRECTION('',(0.,-1.,0.));
#5102=DIRECTION('center_axis',(0.,-1.,0.));
#5103=DIRECTION('ref_axis',(1.,0.,3.91712146416972E-15));
#5104=DIRECTION('center_axis',(0.,-1.,0.));
#5105=DIRECTION('ref_axis',(-0.347608103729637,0.,-0.937639912877799));
#5106=DIRECTION('',(0.,-1.,0.));
#5107=DIRECTION('center_axis',(0.,1.,0.));
#5108=DIRECTION('ref_axis',(1.,0.,0.));
#5109=DIRECTION('center_axis',(0.,-1.,0.));
#5110=DIRECTION('ref_axis',(-0.347608103729637,0.,-0.937639912877799));
#5111=DIRECTION('',(0.,-1.,0.));
#5112=DIRECTION('center_axis',(0.,-1.,0.));
#5113=DIRECTION('ref_axis',(-0.347608103729637,0.,-0.937639912877799));
#5114=DIRECTION('',(0.,-1.,0.));
#5115=DIRECTION('center_axis',(0.,-1.,0.));
#5116=DIRECTION('ref_axis',(-0.347608103729637,0.,-0.937639912877799));
#5117=DIRECTION('',(0.,-1.,0.));
#5118=DIRECTION('center_axis',(0.,1.,0.));
#5119=DIRECTION('ref_axis',(1.,0.,0.));
#5120=DIRECTION('center_axis',(0.,-1.,0.));
#5121=DIRECTION('ref_axis',(-0.347608103729637,0.,-0.937639912877799));
#5122=DIRECTION('center_axis',(0.,-1.,0.));
#5123=DIRECTION('ref_axis',(-0.608635263423501,0.,0.793450134613011));
#5124=DIRECTION('center_axis',(0.,1.,0.));
#5125=DIRECTION('ref_axis',(1.,0.,0.));
#5126=DIRECTION('',(0.,0.,-1.));
#5127=DIRECTION('',(-0.866025403784439,0.,-0.5));
#5128=DIRECTION('',(-0.866025403784439,0.,0.5));
#5129=DIRECTION('',(0.,0.,1.));
#5130=DIRECTION('',(0.866025403784439,0.,0.5));
#5131=DIRECTION('',(0.866025403784439,0.,-0.5));
#5132=DIRECTION('center_axis',(0.5,0.,-0.866025403784439));
#5133=DIRECTION('ref_axis',(0.866025403784439,0.,0.5));
#5134=DIRECTION('',(0.,-1.,0.));
#5135=DIRECTION('',(0.866025403784439,0.,0.5));
#5136=DIRECTION('',(0.,-1.,0.));
#5137=DIRECTION('center_axis',(-0.5,0.,-0.866025403784439));
#5138=DIRECTION('ref_axis',(0.866025403784439,0.,-0.5));
#5139=DIRECTION('',(0.866025403784439,0.,-0.5));
#5140=DIRECTION('',(0.,-1.,0.));
#5141=DIRECTION('center_axis',(-1.,0.,0.));
#5142=DIRECTION('ref_axis',(0.,0.,-1.));
#5143=DIRECTION('',(0.,0.,-1.));
#5144=DIRECTION('',(0.,-1.,0.));
#5145=DIRECTION('center_axis',(-0.5,0.,0.866025403784439));
#5146=DIRECTION('ref_axis',(-0.866025403784439,0.,-0.5));
#5147=DIRECTION('',(-0.866025403784439,0.,-0.5));
#5148=DIRECTION('',(0.,-1.,0.));
#5149=DIRECTION('center_axis',(0.5,0.,0.866025403784439));
#5150=DIRECTION('ref_axis',(-0.866025403784439,0.,0.5));
#5151=DIRECTION('',(-0.866025403784439,0.,0.5));
#5152=DIRECTION('',(0.,-1.,0.));
#5153=DIRECTION('center_axis',(1.,0.,0.));
#5154=DIRECTION('ref_axis',(0.,0.,1.));
#5155=DIRECTION('',(0.,0.,1.));
#5156=DIRECTION('center_axis',(0.,1.,0.));
#5157=DIRECTION('ref_axis',(1.,0.,0.));
#5158=DIRECTION('axis',(0.,0.,1.));
#5159=DIRECTION('refdir',(1.,0.,0.));
#5160=DIRECTION('center_axis',(0.,-1.,0.));
#5161=DIRECTION('ref_axis',(0.853781898007399,0.,-0.520630839112401));
#5162=DIRECTION('',(0.,1.,0.));
#5163=DIRECTION('center_axis',(0.,1.,0.));
#5164=DIRECTION('ref_axis',(1.,0.,1.08690987399046E-13));
#5165=DIRECTION('center_axis',(0.,-1.,0.));
#5166=DIRECTION('ref_axis',(-0.457839658806139,0.,-0.889034783810104));
#5167=DIRECTION('',(0.,1.,0.));
#5168=DIRECTION('center_axis',(0.,-1.,0.));
#5169=DIRECTION('ref_axis',(-0.457839658806139,0.,-0.889034783810104));
#5170=DIRECTION('',(0.,1.,0.));
#5171=DIRECTION('center_axis',(0.,-1.,0.));
#5172=DIRECTION('ref_axis',(-0.457839658806139,0.,-0.889034783810104));
#5173=DIRECTION('',(0.,1.,0.));
#5174=DIRECTION('center_axis',(0.,-1.,0.));
#5175=DIRECTION('ref_axis',(-0.457839658806139,0.,-0.889034783810104));
#5176=DIRECTION('',(0.,1.,0.));
#5177=DIRECTION('center_axis',(0.,-1.,0.));
#5178=DIRECTION('ref_axis',(-0.457839658806139,0.,-0.889034783810104));
#5179=DIRECTION('',(0.,1.,0.));
#5180=DIRECTION('center_axis',(0.,-1.,0.));
#5181=DIRECTION('ref_axis',(-0.457839658806139,0.,-0.889034783810104));
#5182=DIRECTION('',(0.,1.,0.));
#5183=DIRECTION('center_axis',(0.,-1.,0.));
#5184=DIRECTION('ref_axis',(-0.457839658806139,0.,-0.889034783810104));
#5185=DIRECTION('',(0.,1.,0.));
#5186=DIRECTION('center_axis',(0.,-1.,0.));
#5187=DIRECTION('ref_axis',(-0.457839658806139,0.,-0.889034783810104));
#5188=DIRECTION('',(0.,1.,0.));
#5189=DIRECTION('center_axis',(0.,-1.,0.));
#5190=DIRECTION('ref_axis',(-0.457839658806139,0.,-0.889034783810104));
#5191=DIRECTION('',(0.,1.,0.));
#5192=DIRECTION('center_axis',(0.,-1.,0.));
#5193=DIRECTION('ref_axis',(-0.457839658806139,0.,-0.889034783810104));
#5194=DIRECTION('',(0.,1.,0.));
#5195=DIRECTION('center_axis',(0.,-1.,0.));
#5196=DIRECTION('ref_axis',(-0.457839658806139,0.,-0.889034783810104));
#5197=DIRECTION('',(0.,1.,0.));
#5198=DIRECTION('center_axis',(0.,-1.,0.));
#5199=DIRECTION('ref_axis',(-0.457839658806139,0.,-0.889034783810104));
#5200=DIRECTION('',(0.,1.,0.));
#5201=DIRECTION('center_axis',(0.,-1.,0.));
#5202=DIRECTION('ref_axis',(-0.457839658806139,0.,-0.889034783810104));
#5203=DIRECTION('',(0.,1.,0.));
#5204=DIRECTION('center_axis',(0.,-1.,0.));
#5205=DIRECTION('ref_axis',(-0.457839658806139,0.,-0.889034783810104));
#5206=DIRECTION('',(0.,1.,0.));
#5207=DIRECTION('center_axis',(0.,-1.,0.));
#5208=DIRECTION('ref_axis',(-0.457839658806139,0.,-0.889034783810104));
#5209=DIRECTION('',(0.,1.,0.));
#5210=DIRECTION('center_axis',(0.,-1.,0.));
#5211=DIRECTION('ref_axis',(-0.457839658806139,0.,-0.889034783810104));
#5212=DIRECTION('',(0.,1.,0.));
#5213=DIRECTION('center_axis',(0.,-1.,0.));
#5214=DIRECTION('ref_axis',(-0.457839658806139,0.,-0.889034783810104));
#5215=DIRECTION('',(0.,1.,0.));
#5216=DIRECTION('center_axis',(0.,-1.,0.));
#5217=DIRECTION('ref_axis',(-0.457839658806139,0.,-0.889034783810104));
#5218=DIRECTION('',(0.,1.,0.));
#5219=DIRECTION('center_axis',(0.,-1.,0.));
#5220=DIRECTION('ref_axis',(-0.457839658806139,0.,-0.889034783810104));
#5221=DIRECTION('',(0.,1.,0.));
#5222=DIRECTION('center_axis',(0.,-1.,0.));
#5223=DIRECTION('ref_axis',(1.,0.,0.));
#5224=DIRECTION('center_axis',(0.,-1.,0.));
#5225=DIRECTION('ref_axis',(1.,0.,0.));
#5226=DIRECTION('center_axis',(0.,-1.,0.));
#5227=DIRECTION('ref_axis',(1.,0.,0.));
#5228=DIRECTION('center_axis',(0.,-1.,0.));
#5229=DIRECTION('ref_axis',(-0.457839658806139,0.,-0.889034783810104));
#5230=DIRECTION('center_axis',(0.,-1.,0.));
#5231=DIRECTION('ref_axis',(1.,0.,1.08690987399046E-13));
#5232=DIRECTION('center_axis',(0.,1.,0.));
#5233=DIRECTION('ref_axis',(1.,0.,0.));
#5234=DIRECTION('center_axis',(0.,1.,0.));
#5235=DIRECTION('ref_axis',(1.,0.,0.));
#5236=DIRECTION('axis',(0.,0.,1.));
#5237=DIRECTION('refdir',(1.,0.,0.));
#5238=DIRECTION('center_axis',(1.,0.,0.));
#5239=DIRECTION('ref_axis',(0.,0.707106781186547,-0.707106781186548));
#5240=DIRECTION('center_axis',(1.,4.23704587765192E-32,0.));
#5241=DIRECTION('ref_axis',(-2.99604387228618E-32,0.707106781186547,-0.707106781186548));
#5242=DIRECTION('',(1.,0.,0.));
#5243=DIRECTION('center_axis',(-1.,-4.44089209850062E-15,0.));
#5244=DIRECTION('ref_axis',(-3.14018491736754E-15,0.707106781186547,-0.707106781186548));
#5245=DIRECTION('',(-1.,0.,0.));
#5246=DIRECTION('center_axis',(-1.,0.,0.));
#5247=DIRECTION('ref_axis',(0.,0.707106781186547,-0.707106781186548));
#5248=DIRECTION('',(-1.,0.,0.));
#5249=DIRECTION('center_axis',(1.,0.,0.));
#5250=DIRECTION('ref_axis',(0.,1.,0.));
#5251=DIRECTION('',(0.,0.,1.));
#5252=DIRECTION('center_axis',(1.,0.,0.));
#5253=DIRECTION('ref_axis',(0.,0.707106781186546,-0.707106781186549));
#5254=DIRECTION('',(0.,1.,0.));
#5255=DIRECTION('',(0.,0.,1.));
#5256=DIRECTION('',(0.,1.,0.));
#5257=DIRECTION('center_axis',(0.,-1.,0.));
#5258=DIRECTION('ref_axis',(1.,0.,0.));
#5259=DIRECTION('',(0.,0.,-1.));
#5260=DIRECTION('center_axis',(0.,1.,0.));
#5261=DIRECTION('ref_axis',(0.707106781186548,0.,0.707106781186548));
#5262=DIRECTION('',(1.,0.,0.));
#5263=DIRECTION('center_axis',(0.,1.,0.));
#5264=DIRECTION('ref_axis',(0.,0.,-1.));
#5265=DIRECTION('center_axis',(0.,1.,0.));
#5266=DIRECTION('ref_axis',(0.126759996397889,0.,-0.991933416774134));
#5267=DIRECTION('center_axis',(0.,1.,0.));
#5268=DIRECTION('ref_axis',(-0.785839144811216,0.,0.61843094883938));
#5269=DIRECTION('',(0.,0.,1.));
#5270=DIRECTION('',(-1.,0.,0.));
#5271=DIRECTION('center_axis',(0.,1.,0.));
#5272=DIRECTION('ref_axis',(1.,0.,0.));
#5273=DIRECTION('center_axis',(1.,4.44089209850062E-15,0.));
#5274=DIRECTION('ref_axis',(-4.44089209850062E-15,1.,0.));
#5275=DIRECTION('',(0.,0.,1.));
#5276=DIRECTION('',(-4.44089209850062E-15,1.,0.));
#5277=DIRECTION('center_axis',(0.,1.,0.));
#5278=DIRECTION('ref_axis',(-1.,0.,0.));
#5279=DIRECTION('',(0.,0.,-1.));
#5280=DIRECTION('center_axis',(0.,-1.,0.));
#5281=DIRECTION('ref_axis',(-0.785839144811216,0.,0.61843094883938));
#5282=DIRECTION('center_axis',(0.,-1.,0.));
#5283=DIRECTION('ref_axis',(0.126759996397889,0.,-0.991933416774134));
#5284=DIRECTION('center_axis',(0.,-1.,0.));
#5285=DIRECTION('ref_axis',(0.,0.,-1.));
#5286=DIRECTION('',(-1.,0.,0.));
#5287=DIRECTION('center_axis',(0.,-1.,0.));
#5288=DIRECTION('ref_axis',(0.707106781186548,0.,0.707106781186548));
#5289=DIRECTION('center_axis',(0.,-1.,0.));
#5290=DIRECTION('ref_axis',(1.,0.,0.));
#5291=DIRECTION('center_axis',(-1.,0.,0.));
#5292=DIRECTION('ref_axis',(0.,0.707106781186546,-0.707106781186549));
#5293=DIRECTION('center_axis',(-1.,-4.23704587765192E-32,0.));
#5294=DIRECTION('ref_axis',(-2.99604387228617E-32,0.707106781186546,-0.707106781186549));
#5295=DIRECTION('',(1.,0.,0.));
#5296=DIRECTION('center_axis',(0.,1.,0.));
#5297=DIRECTION('ref_axis',(-0.785839144811216,0.,0.61843094883938));
#5298=DIRECTION('',(4.23704587765192E-32,-1.,0.));
#5299=DIRECTION('',(0.,1.,0.));
#5300=DIRECTION('center_axis',(0.,1.,0.));
#5301=DIRECTION('ref_axis',(0.126759996397889,0.,-0.991933416774134));
#5302=DIRECTION('',(0.,-1.,0.));
#5303=DIRECTION('center_axis',(-4.44089209850062E-15,1.,0.));
#5304=DIRECTION('ref_axis',(0.707106781186548,3.14018491736755E-15,0.707106781186548));
#5305=DIRECTION('',(4.44089209850062E-15,-1.,0.));
#5306=DIRECTION('center_axis',(0.,0.,1.));
#5307=DIRECTION('ref_axis',(1.,0.,0.));
#5308=DIRECTION('',(0.,1.,0.));
#5309=DIRECTION('center_axis',(0.,-1.,0.));
#5310=DIRECTION('ref_axis',(0.,0.,-1.));
#5311=DIRECTION('center_axis',(0.,1.,0.));
#5312=DIRECTION('ref_axis',(1.,0.,0.));
#5313=DIRECTION('',(0.,1.,0.));
#5314=DIRECTION('center_axis',(-1.,-4.23704587765192E-32,0.));
#5315=DIRECTION('ref_axis',(4.23704587765192E-32,-1.,0.));
#5316=DIRECTION('',(0.,0.,1.));
#5317=DIRECTION('',(-4.23704587765192E-32,1.,0.));
#5318=DIRECTION('center_axis',(0.,0.,1.));
#5319=DIRECTION('ref_axis',(1.,0.,0.));
#5320=DIRECTION('center_axis',(0.,0.,-1.));
#5321=DIRECTION('ref_axis',(1.,0.,0.));
#5322=DIRECTION('',(0.,0.,1.));
#5323=DIRECTION('center_axis',(0.,0.,-1.));
#5324=DIRECTION('ref_axis',(1.,0.,0.));
#5325=DIRECTION('center_axis',(-1.,0.,0.));
#5326=DIRECTION('ref_axis',(0.,-1.,0.));
#5327=DIRECTION('',(0.,-1.,0.));
#5328=DIRECTION('',(0.,0.,1.));
#5329=DIRECTION('',(0.,-1.,0.));
#5330=DIRECTION('',(0.,0.,1.));
#5331=DIRECTION('center_axis',(0.,0.,1.));
#5332=DIRECTION('ref_axis',(1.,-2.7755575615629E-16,0.));
#5333=DIRECTION('center_axis',(0.,0.,-1.));
#5334=DIRECTION('ref_axis',(1.,-2.7755575615629E-16,0.));
#5335=DIRECTION('center_axis',(0.,0.,-1.));
#5336=DIRECTION('ref_axis',(1.,-2.7755575615629E-16,0.));
#5337=DIRECTION('',(0.,0.,1.));
#5338=DIRECTION('center_axis',(-1.29472072842584E-15,-1.,0.));
#5339=DIRECTION('ref_axis',(1.,-1.29472072842584E-15,0.));
#5340=DIRECTION('',(1.,-1.29472072842584E-15,0.));
#5341=DIRECTION('',(1.,-1.29472072842584E-15,0.));
#5342=DIRECTION('',(0.,0.,1.));
#5343=DIRECTION('center_axis',(0.,0.,1.));
#5344=DIRECTION('ref_axis',(0.,1.,0.));
#5345=DIRECTION('center_axis',(0.,0.,-1.));
#5346=DIRECTION('ref_axis',(0.,1.,0.));
#5347=DIRECTION('center_axis',(0.,0.,-1.));
#5348=DIRECTION('ref_axis',(0.,1.,0.));
#5349=DIRECTION('',(0.,0.,1.));
#5350=DIRECTION('center_axis',(1.,0.,0.));
#5351=DIRECTION('ref_axis',(0.,1.,0.));
#5352=DIRECTION('',(0.,1.,0.));
#5353=DIRECTION('',(0.,1.,0.));
#5354=DIRECTION('',(0.,0.,1.));
#5355=DIRECTION('center_axis',(0.,0.,1.));
#5356=DIRECTION('ref_axis',(-1.,-1.66533453693773E-15,0.));
#5357=DIRECTION('center_axis',(0.,0.,-1.));
#5358=DIRECTION('ref_axis',(-1.,-1.66533453693773E-15,0.));
#5359=DIRECTION('center_axis',(0.,0.,-1.));
#5360=DIRECTION('ref_axis',(-1.,-1.66533453693773E-15,0.));
#5361=DIRECTION('',(0.,0.,1.));
#5362=DIRECTION('center_axis',(-8.09200455266149E-16,1.,0.));
#5363=DIRECTION('ref_axis',(-1.,-8.09200455266149E-16,0.));
#5364=DIRECTION('',(-1.,-8.09200455266149E-16,0.));
#5365=DIRECTION('',(-1.,-8.09200455266149E-16,0.));
#5366=DIRECTION('',(0.,0.,1.));
#5367=DIRECTION('center_axis',(0.,0.,1.));
#5368=DIRECTION('ref_axis',(2.22044604925031E-15,-1.,0.));
#5369=DIRECTION('center_axis',(0.,0.,-1.));
#5370=DIRECTION('ref_axis',(2.22044604925031E-15,-1.,0.));
#5371=DIRECTION('center_axis',(0.,0.,-1.));
#5372=DIRECTION('ref_axis',(2.22044604925031E-15,-1.,0.));
#5373=DIRECTION('center_axis',(0.,0.,1.));
#5374=DIRECTION('ref_axis',(1.58603289232165E-16,1.,0.));
#5375=DIRECTION('center_axis',(0.,0.,1.));
#5376=DIRECTION('ref_axis',(1.58603289232165E-16,1.,0.));
#5377=DIRECTION('',(0.,0.,1.));
#5378=DIRECTION('center_axis',(0.,0.,1.));
#5379=DIRECTION('ref_axis',(1.58603289232165E-16,1.,0.));
#5380=DIRECTION('',(0.,0.,1.));
#5381=DIRECTION('center_axis',(0.,0.,1.));
#5382=DIRECTION('ref_axis',(0.559779357098146,-0.828641702647644,0.));
#5383=DIRECTION('center_axis',(0.,0.,1.));
#5384=DIRECTION('ref_axis',(0.559779357098146,-0.828641702647644,0.));
#5385=DIRECTION('center_axis',(0.,0.,-1.));
#5386=DIRECTION('ref_axis',(0.559779357098146,-0.828641702647644,0.));
#5387=DIRECTION('center_axis',(0.,0.,1.));
#5388=DIRECTION('ref_axis',(-1.,0.,0.));
#5389=DIRECTION('center_axis',(0.,0.,1.));
#5390=DIRECTION('ref_axis',(-1.,0.,0.));
#5391=DIRECTION('center_axis',(0.,0.,-1.));
#5392=DIRECTION('ref_axis',(-1.,0.,0.));
#5393=DIRECTION('',(0.,0.,1.));
#5394=DIRECTION('center_axis',(1.90049007730895E-14,-1.,0.));
#5395=DIRECTION('ref_axis',(1.,1.90049007730895E-14,0.));
#5396=DIRECTION('',(1.,1.90049007730895E-14,0.));
#5397=DIRECTION('',(1.,1.90049007730895E-14,0.));
#5398=DIRECTION('',(0.,0.,1.));
#5399=DIRECTION('center_axis',(0.,0.,1.));
#5400=DIRECTION('ref_axis',(1.,0.,0.));
#5401=DIRECTION('center_axis',(0.,0.,1.));
#5402=DIRECTION('ref_axis',(1.,0.,0.));
#5403=DIRECTION('center_axis',(0.,0.,1.));
#5404=DIRECTION('ref_axis',(1.,0.,0.));
#5405=DIRECTION('',(0.,0.,1.));
#5406=DIRECTION('center_axis',(1.,0.,0.));
#5407=DIRECTION('ref_axis',(0.,1.,0.));
#5408=DIRECTION('',(0.,1.,0.));
#5409=DIRECTION('',(0.,1.,0.));
#5410=DIRECTION('',(0.,0.,1.));
#5411=DIRECTION('center_axis',(0.,0.,1.));
#5412=DIRECTION('ref_axis',(-1.48029736616688E-15,-1.,0.));
#5413=DIRECTION('center_axis',(0.,0.,1.));
#5414=DIRECTION('ref_axis',(-1.48029736616688E-15,-1.,0.));
#5415=DIRECTION('center_axis',(0.,0.,1.));
#5416=DIRECTION('ref_axis',(-1.48029736616688E-15,-1.,0.));
#5417=DIRECTION('',(0.,0.,1.));
#5418=DIRECTION('center_axis',(0.,-1.,0.));
#5419=DIRECTION('ref_axis',(1.,0.,0.));
#5420=DIRECTION('',(1.,0.,0.));
#5421=DIRECTION('',(1.,0.,0.));
#5422=DIRECTION('',(0.,0.,1.));
#5423=DIRECTION('center_axis',(0.,0.,1.));
#5424=DIRECTION('ref_axis',(-1.,0.,0.));
#5425=DIRECTION('center_axis',(0.,0.,1.));
#5426=DIRECTION('ref_axis',(-1.,0.,0.));
#5427=DIRECTION('center_axis',(0.,0.,1.));
#5428=DIRECTION('ref_axis',(-1.,0.,0.));
#5429=DIRECTION('',(0.,0.,1.));
#5430=DIRECTION('center_axis',(-1.,-1.44006500428221E-15,0.));
#5431=DIRECTION('ref_axis',(1.44006500428221E-15,-1.,0.));
#5432=DIRECTION('',(1.44006500428221E-15,-1.,0.));
#5433=DIRECTION('',(1.44006500428221E-15,-1.,0.));
#5434=DIRECTION('center_axis',(0.,0.,1.));
#5435=DIRECTION('ref_axis',(1.,0.,0.));
#5436=DIRECTION('center_axis',(0.,0.,1.));
#5437=DIRECTION('ref_axis',(1.,0.,0.));
#5438=DIRECTION('axis',(0.,0.,1.));
#5439=DIRECTION('refdir',(1.,0.,0.));
#5440=DIRECTION('center_axis',(1.,0.,0.));
#5441=DIRECTION('ref_axis',(0.,1.,0.));
#5442=DIRECTION('',(0.,-2.22044604925031E-16,-1.));
#5443=DIRECTION('center_axis',(-1.,0.,0.));
#5444=DIRECTION('ref_axis',(0.,1.,0.));
#5445=DIRECTION('center_axis',(-1.,0.,0.));
#5446=DIRECTION('ref_axis',(0.,1.,0.));
#5447=DIRECTION('',(0.,2.22044604925031E-16,1.));
#5448=DIRECTION('',(0.,1.,-2.22044604925031E-16));
#5449=DIRECTION('center_axis',(-1.,0.,0.));
#5450=DIRECTION('ref_axis',(0.,1.,0.));
#5451=DIRECTION('center_axis',(-1.,0.,0.));
#5452=DIRECTION('ref_axis',(0.,1.,0.));
#5453=DIRECTION('',(-1.,0.,0.));
#5454=DIRECTION('center_axis',(0.,2.22044604925031E-16,1.));
#5455=DIRECTION('ref_axis',(-1.,0.,0.));
#5456=DIRECTION('center_axis',(0.,2.22044604925031E-16,1.));
#5457=DIRECTION('ref_axis',(-1.,0.,0.));
#5458=DIRECTION('center_axis',(-1.,0.,0.));
#5459=DIRECTION('ref_axis',(0.,1.,-2.22044604925031E-16));
#5460=DIRECTION('center_axis',(1.,0.,0.));
#5461=DIRECTION('ref_axis',(0.,-1.,2.22044604925031E-16));
#5462=DIRECTION('center_axis',(0.,-2.22044604925031E-16,-1.));
#5463=DIRECTION('ref_axis',(-1.,0.,0.));
#5464=DIRECTION('center_axis',(0.,2.22044604925031E-16,1.));
#5465=DIRECTION('ref_axis',(-1.,0.,0.));
#5466=DIRECTION('',(0.,-2.22044604925031E-16,-1.));
#5467=DIRECTION('center_axis',(1.,0.,0.));
#5468=DIRECTION('ref_axis',(0.,-1.,2.22044604925031E-16));
#5469=DIRECTION('',(-1.,0.,0.));
#5470=DIRECTION('center_axis',(1.,0.,0.));
#5471=DIRECTION('ref_axis',(0.,-1.,2.22044604925031E-16));
#5472=DIRECTION('center_axis',(1.,0.,0.));
#5473=DIRECTION('ref_axis',(0.,-1.,2.22044604925031E-16));
#5474=DIRECTION('center_axis',(-1.,2.71926214689378E-32,1.22464679914735E-16));
#5475=DIRECTION('ref_axis',(1.1368907822176E-16,2.22044604925031E-16,1.));
#5476=DIRECTION('center_axis',(7.49879891330929E-33,-1.,3.44509284839766E-16));
#5477=DIRECTION('ref_axis',(-7.10556738886E-17,-3.44509284839766E-16,-1.));
#5478=DIRECTION('center_axis',(1.,0.,0.));
#5479=DIRECTION('ref_axis',(0.,0.,-1.));
#5480=DIRECTION('center_axis',(-1.,0.,0.));
#5481=DIRECTION('ref_axis',(0.,0.,-1.));
#5482=DIRECTION('',(-1.,0.,0.));
#5483=DIRECTION('center_axis',(1.,0.,0.));
#5484=DIRECTION('ref_axis',(0.,0.,-1.));
#5485=DIRECTION('center_axis',(1.,-1.22464679914736E-16,0.));
#5486=DIRECTION('ref_axis',(0.,-1.,0.));
#5487=DIRECTION('center_axis',(1.,0.,0.));
#5488=DIRECTION('ref_axis',(0.,0.,-1.));
#5489=DIRECTION('center_axis',(1.,0.,0.));
#5490=DIRECTION('ref_axis',(0.,0.,-1.));
#5491=DIRECTION('center_axis',(-7.4987989133093E-33,-1.22464679914735E-16,
1.));
#5492=DIRECTION('ref_axis',(0.,1.,1.22464679914735E-16));
#5493=DIRECTION('center_axis',(0.,1.,0.));
#5494=DIRECTION('ref_axis',(1.,0.,0.));
#5495=DIRECTION('center_axis',(1.,0.,0.));
#5496=DIRECTION('ref_axis',(0.,0.,-1.));
#5497=DIRECTION('',(-1.,0.,0.));
#5498=DIRECTION('center_axis',(1.,0.,0.));
#5499=DIRECTION('ref_axis',(0.,0.,-1.));
#5500=DIRECTION('center_axis',(0.,1.,0.));
#5501=DIRECTION('ref_axis',(1.,0.,0.));
#5502=DIRECTION('center_axis',(0.,1.,0.));
#5503=DIRECTION('ref_axis',(1.,0.,0.));
#5504=DIRECTION('center_axis',(0.,-1.,0.));
#5505=DIRECTION('ref_axis',(1.,0.,0.));
#5506=DIRECTION('',(0.,-1.,0.));
#5507=DIRECTION('center_axis',(-1.,0.,0.));
#5508=DIRECTION('ref_axis',(0.,0.,1.));
#5509=DIRECTION('center_axis',(1.,0.,0.));
#5510=DIRECTION('ref_axis',(0.,1.,0.));
#5511=DIRECTION('',(0.,0.,1.));
#5512=DIRECTION('',(1.,0.,0.));
#5513=DIRECTION('',(0.,0.,1.));
#5514=DIRECTION('',(1.,0.,0.));
#5515=DIRECTION('',(0.,0.,1.));
#5516=DIRECTION('',(1.,0.,0.));
#5517=DIRECTION('',(0.,0.,1.));
#5518=DIRECTION('',(1.,0.,0.));
#5519=DIRECTION('',(0.,0.,1.));
#5520=DIRECTION('',(1.,0.,0.));
#5521=DIRECTION('',(0.,0.,1.));
#5522=DIRECTION('',(1.,0.,0.));
#5523=DIRECTION('',(0.,0.,1.));
#5524=DIRECTION('',(1.,0.,0.));
#5525=DIRECTION('',(0.,0.,1.));
#5526=DIRECTION('',(1.,0.,0.));
#5527=CARTESIAN_POINT('',(0.,0.,0.));
#5528=CARTESIAN_POINT('',(0.,0.,0.));
#5529=CARTESIAN_POINT('Origin',(9.94695118785088,27.0570908269895,11.9861373773513));
#5530=CARTESIAN_POINT('',(-26.6569870402034,30.0570908269895,11.9861373773513));
#5531=CARTESIAN_POINT('',(-26.6064009422907,29.8855179517357,10.9861373773513));
#5532=CARTESIAN_POINT('Ctrl Pts',(-26.6569870402035,30.0570908269895,11.9861373773513));
#5533=CARTESIAN_POINT('Ctrl Pts',(-26.6238975552776,30.0570908269895,11.6599132580678));
#5534=CARTESIAN_POINT('Ctrl Pts',(-26.6064009422907,30.0012679867952,11.3135279162041));
#5535=CARTESIAN_POINT('Ctrl Pts',(-26.6064009422907,29.8855179517357,10.9861373773513));
#5536=CARTESIAN_POINT('',(14.3037866333901,30.0570908269895,11.9861373773513));
#5537=CARTESIAN_POINT('',(9.94695118785088,30.0570908269895,11.9861373773513));
#5538=CARTESIAN_POINT('',(14.3037866333901,29.8855179517357,10.9861373773513));
#5539=CARTESIAN_POINT('Origin',(14.3037866333901,27.0570908269895,11.9861373773513));
#5540=CARTESIAN_POINT('',(14.3039511878509,29.8855179517357,10.9861373773513));
#5541=CARTESIAN_POINT('',(9.94695118785088,29.8855179517357,10.9861373773513));
#5542=CARTESIAN_POINT('',(14.3039511878509,27.0570908269895,8.98613737735134));
#5543=CARTESIAN_POINT('Origin',(14.3039511878509,27.0570908269895,11.9861373773513));
#5544=CARTESIAN_POINT('',(-26.6060488121491,27.0570908269895,8.98613737735134));
#5545=CARTESIAN_POINT('',(9.94695118785088,27.0570908269895,8.98613737735134));
#5546=CARTESIAN_POINT('Origin',(-26.6060488121491,27.0570908269895,11.9861373773513));
#5547=CARTESIAN_POINT('Origin',(14.3037866333901,30.0570908269895,15.0708658676184));
#5548=CARTESIAN_POINT('',(14.3037866333901,30.0570908269895,15.0708658676184));
#5549=CARTESIAN_POINT('',(14.3037866333901,30.0570908269895,15.0708658676184));
#5550=CARTESIAN_POINT('',(14.3037866333901,28.0570908269895,15.0708658676184));
#5551=CARTESIAN_POINT('',(14.3037866333901,30.0570908269895,15.0708658676184));
#5552=CARTESIAN_POINT('',(14.3037866333901,28.0570908269895,11.4861373773513));
#5553=CARTESIAN_POINT('',(14.3037866333901,28.0570908269895,15.0708658676184));
#5554=CARTESIAN_POINT('',(14.3037866333901,27.5570908269895,10.9861373773513));
#5555=CARTESIAN_POINT('Origin',(14.3037866333901,27.5570908269895,11.4861373773513));
#5556=CARTESIAN_POINT('',(14.3037866333901,30.0570908269895,10.9861373773513));
#5557=CARTESIAN_POINT('Origin',(-35.7730488121491,30.0570908269895,10.9861373773513));
#5558=CARTESIAN_POINT('',(-26.6060488121491,27.5570908269895,10.9861373773513));
#5559=CARTESIAN_POINT('',(-20.5330488121491,27.5570908269895,10.9861373773513));
#5560=CARTESIAN_POINT('',(-26.6060488121491,25.1429698676036,10.9861373773513));
#5561=CARTESIAN_POINT('',(-26.6060488121491,30.0570908269895,10.9861373773513));
#5562=CARTESIAN_POINT('',(-23.9288509427725,21.7410591318785,10.9861373773513));
#5563=CARTESIAN_POINT('Origin',(-23.1060488121491,25.1429698676036,10.9861373773513));
#5564=CARTESIAN_POINT('',(-5.04779768493513,-1.21054870903725,10.9861373773513));
#5565=CARTESIAN_POINT('Origin',(-29.7388199751065,-2.28050728087887,10.9861373773513));
#5566=CARTESIAN_POINT('',(3.94376397208333,-9.82090917301047,10.9861373773513));
#5567=CARTESIAN_POINT('Origin',(3.94376397208333,-0.820909173010468,10.9861373773513));
#5568=CARTESIAN_POINT('',(5.30395118785094,-9.82090917301047,10.9861373773513));
#5569=CARTESIAN_POINT('',(25.1869511878509,-9.82090917301046,10.9861373773513));
#5570=CARTESIAN_POINT('',(14.3039511878509,-0.820909173010467,10.9861373773513));
#5571=CARTESIAN_POINT('Origin',(5.30395118785094,-0.820909173010468,10.9861373773512));
#5572=CARTESIAN_POINT('',(14.3039511878509,30.0570908269895,10.9861373773513));
#5573=CARTESIAN_POINT('',(0.0114691062182715,3.00528005601026E-15,10.9861373773513));
#5574=CARTESIAN_POINT('Origin',(4.45646910621825,3.54963555823125E-15,10.9861373773513));
#5575=CARTESIAN_POINT('Origin',(14.3039511878509,30.0570908269895,10.9861373773514));
#5576=CARTESIAN_POINT('',(14.3039511878509,-0.820909173010467,8.98613737735134));
#5577=CARTESIAN_POINT('',(14.3039511878509,-0.820909173010467,10.4861373773513));
#5578=CARTESIAN_POINT('',(14.3039511878509,30.0570908269895,8.98613737735134));
#5579=CARTESIAN_POINT('Origin',(25.1869511878509,30.0570908269895,8.98613737735134));
#5580=CARTESIAN_POINT('',(5.30395118785094,-9.82090917301047,8.98613737735135));
#5581=CARTESIAN_POINT('Origin',(5.30395118785094,-0.820909173010468,8.98613737735143));
#5582=CARTESIAN_POINT('',(3.94376397208333,-9.82090917301047,8.98613737735135));
#5583=CARTESIAN_POINT('',(-35.7730488121491,-9.82090917301047,8.98613737735135));
#5584=CARTESIAN_POINT('',(-5.04779768493513,-1.21054870903725,8.98613737735134));
#5585=CARTESIAN_POINT('Origin',(3.94376397208333,-0.820909173010468,8.98613737735134));
#5586=CARTESIAN_POINT('',(-23.9288509427725,21.7410591318785,8.98613737735134));
#5587=CARTESIAN_POINT('Origin',(-29.7388199751065,-2.28050728087887,8.98613737735134));
#5588=CARTESIAN_POINT('',(-26.6060488121491,25.1429698676036,8.98613737735134));
#5589=CARTESIAN_POINT('Origin',(-23.1060488121491,25.1429698676036,8.98613737735134));
#5590=CARTESIAN_POINT('',(-26.6060488121491,30.0570908269895,8.98613737735134));
#5591=CARTESIAN_POINT('',(0.0114691062182715,2.5611908461602E-15,8.98613737735134));
#5592=CARTESIAN_POINT('Origin',(4.45646910621825,3.10554634838119E-15,8.98613737735134));
#5593=CARTESIAN_POINT('Origin',(-20.5330488121491,27.5570908269895,11.4861373773513));
#5594=CARTESIAN_POINT('',(-26.6060488121491,28.0570908269895,11.4861373773513));
#5595=CARTESIAN_POINT('Origin',(-26.6060488121491,27.5570908269895,11.4861373773513));
#5596=CARTESIAN_POINT('',(-20.5330488121491,28.0570908269895,11.4861373773513));
#5597=CARTESIAN_POINT('Origin',(-23.1060488121491,25.1429698676036,10.9861373773513));
#5598=CARTESIAN_POINT('',(-23.9288509427725,21.7410591318785,10.9861373773513));
#5599=CARTESIAN_POINT('',(-26.6060488121491,25.1429698676036,10.9861373773513));
#5600=CARTESIAN_POINT('Origin',(-29.7388199751065,-2.28050728087887,10.9861373773513));
#5601=CARTESIAN_POINT('',(-5.04779768493513,-1.21054870903725,10.9861373773513));
#5602=CARTESIAN_POINT('Origin',(5.30395118785094,-0.820909173010468,10.4861373773514));
#5603=CARTESIAN_POINT('',(5.30395118785094,-9.82090917301047,10.4861373773514));
#5604=CARTESIAN_POINT('Origin',(-5.29304881214905,-9.82090917301047,9.98613737735135));
#5605=CARTESIAN_POINT('',(3.94376397208333,-9.82090917301047,10.9861373773513));
#5606=CARTESIAN_POINT('Origin',(3.94376397208333,-0.820909173010468,10.9861373773513));
#5607=CARTESIAN_POINT('Origin',(4.45646910621825,3.54963555823125E-15,10.9861373773513));
#5608=CARTESIAN_POINT('',(0.0114691062182498,2.46092455378925E-15,10.9861373773513));
#5609=CARTESIAN_POINT('Origin',(-26.6060488121491,30.0570908269895,8.98613737735134));
#5610=CARTESIAN_POINT('',(-26.6064009422907,28.0570908269895,10.9861373773513));
#5611=CARTESIAN_POINT('',(-26.6060488121491,28.0570908269895,15.8361373773513));
#5612=CARTESIAN_POINT('',(-26.6064009422907,30.0570908269895,10.9861373773513));
#5613=CARTESIAN_POINT('Origin',(-27.075934518241,30.0570908269895,26.9411392547891));
#5614=CARTESIAN_POINT('',(-31.5209345182411,28.0570908269895,26.9411392547891));
#5615=CARTESIAN_POINT('Origin',(-27.075934518241,28.0570908269895,26.9411392547891));
#5616=CARTESIAN_POINT('',(-31.5209345182411,30.0570908269895,26.9411392547891));
#5617=CARTESIAN_POINT('',(-31.520934518241,30.0570908269895,26.9411392547891));
#5618=CARTESIAN_POINT('Origin',(-27.075934518241,30.0570908269895,26.9411392547891));
#5619=CARTESIAN_POINT('Origin',(21.2986430042118,30.0570908269895,26.4627140227474));
#5620=CARTESIAN_POINT('',(21.2986430042118,30.0570908269895,26.4627140227474));
#5621=CARTESIAN_POINT('',(21.2986430042118,30.0570908269895,27.3527140227474));
#5622=CARTESIAN_POINT('',(21.2986430042118,30.0570908269895,26.4627140227474));
#5623=CARTESIAN_POINT('',(21.2986430042118,28.0570908269895,26.4627140227474));
#5624=CARTESIAN_POINT('',(21.2986430042118,30.0570908269895,26.4627140227474));
#5625=CARTESIAN_POINT('',(21.2986430042118,28.0570908269895,27.3527140227474));
#5626=CARTESIAN_POINT('',(21.2986430042118,28.0570908269895,26.4627140227474));
#5627=CARTESIAN_POINT('',(21.2986430042118,30.0570908269895,27.3527140227474));
#5628=CARTESIAN_POINT('Origin',(17.2986430042118,30.0570908269895,26.4627140227474));
#5629=CARTESIAN_POINT('',(17.2986430042118,30.0570908269895,22.4627140227474));
#5630=CARTESIAN_POINT('Origin',(17.2986430042118,30.0570908269895,26.4627140227474));
#5631=CARTESIAN_POINT('',(17.2986430042118,28.0570908269895,22.4627140227474));
#5632=CARTESIAN_POINT('',(17.2986430042118,30.0570908269895,22.4627140227474));
#5633=CARTESIAN_POINT('Origin',(17.2986430042118,28.0570908269895,26.4627140227474));
#5634=CARTESIAN_POINT('Origin',(13.8686430042118,30.0570908269895,22.4627140227474));
#5635=CARTESIAN_POINT('',(13.8686430042118,30.0570908269895,22.4627140227474));
#5636=CARTESIAN_POINT('',(13.8686430042118,30.0570908269895,22.4627140227474));
#5637=CARTESIAN_POINT('',(13.8686430042118,28.0570908269895,22.4627140227474));
#5638=CARTESIAN_POINT('',(13.8686430042118,30.0570908269895,22.4627140227474));
#5639=CARTESIAN_POINT('',(13.8686430042118,28.0570908269895,22.4627140227474));
#5640=CARTESIAN_POINT('Origin',(13.8686430042118,30.0570908269895,26.4627140227474));
#5641=CARTESIAN_POINT('',(9.86864300421174,30.0570908269895,26.4627140227474));
#5642=CARTESIAN_POINT('Origin',(13.8686430042118,30.0570908269895,26.4627140227474));
#5643=CARTESIAN_POINT('',(9.86864300421174,28.0570908269895,26.4627140227474));
#5644=CARTESIAN_POINT('',(9.86864300421174,30.0570908269895,26.4627140227474));
#5645=CARTESIAN_POINT('Origin',(13.8686430042118,28.0570908269895,26.4627140227474));
#5646=CARTESIAN_POINT('Origin',(9.86864300421174,30.0570908269895,27.3527140227474));
#5647=CARTESIAN_POINT('',(9.86864300421174,30.0570908269895,27.3527140227474));
#5648=CARTESIAN_POINT('',(9.86864300421174,30.0570908269895,27.3527140227474));
#5649=CARTESIAN_POINT('',(9.86864300421174,28.0570908269895,27.3527140227474));
#5650=CARTESIAN_POINT('',(9.86864300421174,30.0570908269895,27.3527140227474));
#5651=CARTESIAN_POINT('',(9.86864300421174,28.0570908269895,27.3527140227474));
#5652=CARTESIAN_POINT('Origin',(13.8686430042118,30.0570908269895,27.3527140227474));
#5653=CARTESIAN_POINT('',(13.8686430042118,30.0570908269895,31.3527140227474));
#5654=CARTESIAN_POINT('Origin',(13.8686430042118,30.0570908269895,27.3527140227474));
#5655=CARTESIAN_POINT('',(13.8686430042118,28.0570908269895,31.3527140227474));
#5656=CARTESIAN_POINT('',(13.8686430042118,30.0570908269895,31.3527140227474));
#5657=CARTESIAN_POINT('Origin',(13.8686430042118,28.0570908269895,27.3527140227474));
#5658=CARTESIAN_POINT('Origin',(17.2986430042118,30.0570908269895,31.3527140227474));
#5659=CARTESIAN_POINT('',(17.2986430042118,30.0570908269895,31.3527140227474));
#5660=CARTESIAN_POINT('',(17.2986430042118,30.0570908269895,31.3527140227474));
#5661=CARTESIAN_POINT('',(17.2986430042118,28.0570908269895,31.3527140227474));
#5662=CARTESIAN_POINT('',(17.2986430042118,30.0570908269895,31.3527140227474));
#5663=CARTESIAN_POINT('',(17.2986430042118,28.0570908269895,31.3527140227474));
#5664=CARTESIAN_POINT('Origin',(17.2986430042118,30.0570908269895,27.3527140227474));
#5665=CARTESIAN_POINT('Origin',(17.2986430042118,30.0570908269895,27.3527140227474));
#5666=CARTESIAN_POINT('Origin',(17.2986430042118,28.0570908269895,27.3527140227474));
#5667=CARTESIAN_POINT('Origin',(-28.773048812149,30.0570908269895,25.8442305588067));
#5668=CARTESIAN_POINT('',(-30.9687372874527,30.0570908269895,19.197505642021));
#5669=CARTESIAN_POINT('',(-35.7730488121491,30.0570908269895,25.8442305588067));
#5670=CARTESIAN_POINT('Origin',(-28.773048812149,30.0570908269895,25.8442305588067));
#5671=CARTESIAN_POINT('',(-30.9687372874527,28.0570908269895,19.197505642021));
#5672=CARTESIAN_POINT('',(-30.9687372874527,30.0570908269895,19.197505642021));
#5673=CARTESIAN_POINT('',(-35.7730488121491,28.0570908269895,25.8442305588067));
#5674=CARTESIAN_POINT('Origin',(-28.773048812149,28.0570908269895,25.8442305588067));
#5675=CARTESIAN_POINT('',(-35.7730488121491,30.0570908269895,25.8442305588067));
#5676=CARTESIAN_POINT('Origin',(-36.5158325318825,30.0570908269895,10.9861373773513));
#5677=CARTESIAN_POINT('Origin',(-36.5158325318825,28.0570908269895,10.9861373773513));
#5678=CARTESIAN_POINT('Origin',(-36.5158325318825,30.0570908269895,10.9861373773513));
#5679=CARTESIAN_POINT('Origin',(19.3037866333901,30.0570908269895,15.0708658676184));
#5680=CARTESIAN_POINT('',(19.3037866333901,30.0570908269895,20.0708658676184));
#5681=CARTESIAN_POINT('Origin',(19.3037866333901,30.0570908269895,15.0708658676184));
#5682=CARTESIAN_POINT('',(19.3037866333901,28.0570908269895,20.0708658676184));
#5683=CARTESIAN_POINT('',(19.3037866333901,30.0570908269895,20.0708658676184));
#5684=CARTESIAN_POINT('Origin',(19.3037866333901,28.0570908269895,15.0708658676184));
#5685=CARTESIAN_POINT('Origin',(19.1869511878509,30.0570908269895,20.0708658676184));
#5686=CARTESIAN_POINT('',(19.1869511878509,30.0570908269895,20.0708658676184));
#5687=CARTESIAN_POINT('',(19.1869511878509,30.0570908269895,20.0708658676184));
#5688=CARTESIAN_POINT('',(19.1869511878509,28.0570908269895,20.0708658676183));
#5689=CARTESIAN_POINT('',(19.1869511878509,30.0570908269895,20.0708658676184));
#5690=CARTESIAN_POINT('',(19.1869511878509,28.0570908269895,20.0708658676184));
#5691=CARTESIAN_POINT('Origin',(19.1869511878509,30.0570908269895,26.0708658676183));
#5692=CARTESIAN_POINT('',(25.1869511878509,30.0570908269895,26.0708658676183));
#5693=CARTESIAN_POINT('Origin',(19.1869511878509,30.0570908269895,26.0708658676183));
#5694=CARTESIAN_POINT('',(25.1869511878509,28.0570908269895,26.0708658676183));
#5695=CARTESIAN_POINT('',(25.1869511878509,30.0570908269895,26.0708658676183));
#5696=CARTESIAN_POINT('Origin',(19.1869511878509,28.0570908269895,26.0708658676183));
#5697=CARTESIAN_POINT('Origin',(25.1869511878509,30.0570908269895,28.3861373773513));
#5698=CARTESIAN_POINT('',(25.1869511878509,30.0570908269895,28.3861373773513));
#5699=CARTESIAN_POINT('',(25.1869511878509,30.0570908269895,34.3861373773513));
#5700=CARTESIAN_POINT('',(25.1869511878509,28.0570908269895,28.3861373773513));
#5701=CARTESIAN_POINT('',(25.1869511878509,30.0570908269895,28.3861373773513));
#5702=CARTESIAN_POINT('',(25.1869511878509,28.0570908269895,34.3861373773513));
#5703=CARTESIAN_POINT('Origin',(19.1869511878509,30.0570908269895,28.3861373773514));
#5704=CARTESIAN_POINT('',(19.1869511878509,30.0570908269895,34.3861373773513));
#5705=CARTESIAN_POINT('Origin',(19.1869511878509,30.0570908269895,28.3861373773514));
#5706=CARTESIAN_POINT('',(19.1869511878509,28.0570908269895,34.3861373773513));
#5707=CARTESIAN_POINT('',(19.1869511878509,30.0570908269895,34.3861373773513));
#5708=CARTESIAN_POINT('Origin',(19.1869511878509,28.0570908269895,28.3861373773513));
#5709=CARTESIAN_POINT('Origin',(-28.773048812149,30.0570908269895,34.3861373773513));
#5710=CARTESIAN_POINT('',(-28.773048812149,30.0570908269895,34.3861373773513));
#5711=CARTESIAN_POINT('',(-35.7730488121491,30.0570908269895,34.3861373773513));
#5712=CARTESIAN_POINT('',(-28.773048812149,28.0570908269895,34.3861373773513));
#5713=CARTESIAN_POINT('',(-28.773048812149,30.0570908269895,34.3861373773513));
#5714=CARTESIAN_POINT('',(-35.7730488121491,28.0570908269895,34.3861373773513));
#5715=CARTESIAN_POINT('Origin',(-28.773048812149,30.0570908269895,27.3861373773513));
#5716=CARTESIAN_POINT('',(-35.7730488121491,30.0570908269895,27.3861373773513));
#5717=CARTESIAN_POINT('Origin',(-28.773048812149,30.0570908269895,27.3861373773513));
#5718=CARTESIAN_POINT('',(-35.7730488121491,28.0570908269895,27.3861373773513));
#5719=CARTESIAN_POINT('',(-35.7730488121491,30.0570908269895,27.3861373773513));
#5720=CARTESIAN_POINT('Origin',(-28.773048812149,28.0570908269895,27.3861373773513));
#5721=CARTESIAN_POINT('Origin',(-35.7730488121491,30.0570908269895,25.8442305588067));
#5722=CARTESIAN_POINT('',(-35.7730488121491,30.0570908269895,25.8442305588067));
#5723=CARTESIAN_POINT('',(-35.7730488121491,28.0570908269895,25.8442305588067));
#5724=CARTESIAN_POINT('Origin',(-5.29304881214906,28.0570908269895,22.6861373773513));
#5725=CARTESIAN_POINT('Origin',(-5.29304881214906,30.0570908269895,22.6861373773513));
#5726=CARTESIAN_POINT('',(0.,0.,0.));
#5727=CARTESIAN_POINT('Origin',(4.45646910621825,-5.13094777615093E-16,
-2.31077344927308));
#5728=CARTESIAN_POINT('',(7.67921910621823,-7.83531977023612E-9,24.5634577632816));
#5729=CARTESIAN_POINT('',(7.67921909177343,0.00030512938119044,24.8107734493052));
#5730=CARTESIAN_POINT('',(7.67921910621823,-3.51191647465084E-13,-2.31077344927308));
#5731=CARTESIAN_POINT('',(6.32805563795728,-2.62360084935053,25.));
#5732=CARTESIAN_POINT('Ctrl Pts',(7.67921909177343,0.00030512938123435,
24.8107734493052));
#5733=CARTESIAN_POINT('Ctrl Pts',(7.67922866593268,-0.100816307841584,24.8170649336023));
#5734=CARTESIAN_POINT('Ctrl Pts',(7.67447455962406,-0.202100590921019,24.8233564178993));
#5735=CARTESIAN_POINT('Ctrl Pts',(7.66493680196462,-0.303071951608608,24.8296479021964));
#5736=CARTESIAN_POINT('Ctrl Pts',(7.65541369343921,-0.40388822940893,24.835929723342));
#5737=CARTESIAN_POINT('Ctrl Pts',(7.64112158799093,-0.504392131358855,24.8422115444877));
#5738=CARTESIAN_POINT('Ctrl Pts',(7.62209250725414,-0.604107643813442,24.8484933656333));
#5739=CARTESIAN_POINT('Ctrl Pts',(7.60296965583703,-0.704314530053787,24.8548061420653));
#5740=CARTESIAN_POINT('Ctrl Pts',(7.57906299733081,-0.803724810365966,24.8611189184972));
#5741=CARTESIAN_POINT('Ctrl Pts',(7.55045802283427,-0.901859271925004,24.8674316949291));
#5742=CARTESIAN_POINT('Ctrl Pts',(7.52206334493677,-0.999272273532457,24.8736980614119));
#5743=CARTESIAN_POINT('Ctrl Pts',(7.48903930758529,-1.09542774532358,24.8799644278946));
#5744=CARTESIAN_POINT('Ctrl Pts',(7.45152072289721,-1.18986695723875,24.8862307943773));
#5745=CARTESIAN_POINT('Ctrl Pts',(7.41402723871525,-1.28424298787894,24.8924929685651));
#5746=CARTESIAN_POINT('Ctrl Pts',(7.37204534178874,-1.3769046584151,24.898755142753));
#5747=CARTESIAN_POINT('Ctrl Pts',(7.32575909003815,-1.46741015099755,24.9050173169408));
#5748=CARTESIAN_POINT('Ctrl Pts',(7.27949302102046,-1.55787617941703,24.91127676056));
#5749=CARTESIAN_POINT('Ctrl Pts',(7.22892652098825,-1.64618753215808,24.9175362041791));
#5750=CARTESIAN_POINT('Ctrl Pts',(7.17429069621859,-1.73192475801575,24.9237956477983));
#5751=CARTESIAN_POINT('Ctrl Pts',(7.11886128045777,-1.81890732592385,24.9301460104818));
#5752=CARTESIAN_POINT('Ctrl Pts',(7.05924358165052,-1.90324000330923,24.9364963731652));
#5753=CARTESIAN_POINT('Ctrl Pts',(6.99572561601069,-1.98451352728485,24.9428467358487));
#5754=CARTESIAN_POINT('Ctrl Pts',(6.93311093007416,-2.06463127235786,24.9491067909529));
#5755=CARTESIAN_POINT('Ctrl Pts',(6.8667064827474,-2.1417760003413,24.955366846057));
#5756=CARTESIAN_POINT('Ctrl Pts',(6.79682929633059,-2.21558835144013,24.9616269011612));
#5757=CARTESIAN_POINT('Ctrl Pts',(6.72544003706848,-2.29099792843581,24.9680224176343));
#5758=CARTESIAN_POINT('Ctrl Pts',(6.65042630261387,-2.3629288987071,24.9744179341074));
#5759=CARTESIAN_POINT('Ctrl Pts',(6.57216557829183,-2.43103805000153,24.9808134505806));
#5760=CARTESIAN_POINT('Ctrl Pts',(6.49390485396981,-2.49914720129594,24.9872089670537));
#5761=CARTESIAN_POINT('Ctrl Pts',(6.41239751072598,-2.56343426068115,24.9936044835268));
#5762=CARTESIAN_POINT('Ctrl Pts',(6.3280556379573,-2.62360084935053,25.));
#5763=CARTESIAN_POINT('',(2.62314711761431,-2.65048072028474,25.));
#5764=CARTESIAN_POINT('Origin',(4.45646910621825,5.55111512312578E-15,25.));
#5765=CARTESIAN_POINT('Ctrl Pts',(2.62314711761429,-2.65048072028473,25.));
#5766=CARTESIAN_POINT('Ctrl Pts',(2.89144904079663,-2.8360635889283,24.9786416469637));
#5767=CARTESIAN_POINT('Ctrl Pts',(3.18648460629579,-2.97991334644022,24.9559344725635));
#5768=CARTESIAN_POINT('Ctrl Pts',(3.58512066923102,-3.10405331522512,24.928741492428));
#5769=CARTESIAN_POINT('Ctrl Pts',(3.67309955673177,-3.12741584059926,24.922921141824));
#5770=CARTESIAN_POINT('Ctrl Pts',(3.78661194416149,-3.15246672202482,24.915635611859));
#5771=CARTESIAN_POINT('Ctrl Pts',(3.81133084498954,-3.15761804725921,24.9140623241602));
#5772=CARTESIAN_POINT('Ctrl Pts',(3.85142009765253,-3.1654820695268,24.9115315157959));
#5773=CARTESIAN_POINT('Ctrl Pts',(3.86675371263984,-3.16837447333492,24.9105684001871));
#5774=CARTESIAN_POINT('Ctrl Pts',(3.89619116696891,-3.17370619888223,24.9087285488888));
#5775=CARTESIAN_POINT('Ctrl Pts',(3.91029139758291,-3.17616314550513,24.9078512832115));
#5776=CARTESIAN_POINT('Ctrl Pts',(3.94254820011921,-3.18156269199861,24.9058532878385));
#5777=CARTESIAN_POINT('Ctrl Pts',(3.96071463471363,-3.18444396812544,24.9047344846621));
#5778=CARTESIAN_POINT('Ctrl Pts',(4.01828094934606,-3.19306967907415,24.9012087320305));
#5779=CARTESIAN_POINT('Ctrl Pts',(4.05776401829735,-3.19823971799934,24.8988194688504));
#5780=CARTESIAN_POINT('Ctrl Pts',(4.33720985013774,-3.22957562514283,24.8820913837109));
#5781=CARTESIAN_POINT('Ctrl Pts',(4.5793490161818,-3.22944192584949,24.8686180366021));
#5782=CARTESIAN_POINT('Ctrl Pts',(4.99722054928059,-3.18210555296314,24.8449564574255));
#5783=CARTESIAN_POINT('Ctrl Pts',(5.17320613386012,-3.14713821540364,24.8348323999712));
#5784=CARTESIAN_POINT('Ctrl Pts',(5.3643396599289,-3.09229347408763,24.8228055157499));
#5785=CARTESIAN_POINT('Ctrl Pts',(5.38327855959523,-3.08667006112428,24.8216021234757));
#5786=CARTESIAN_POINT('Ctrl Pts',(5.41157107911454,-3.07798547988199,24.8197851945844));
#5787=CARTESIAN_POINT('Ctrl Pts',(5.4209647098772,-3.07505489670163,24.8191787521801));
#5788=CARTESIAN_POINT('Ctrl Pts',(5.43040894855634,-3.07206099395158,24.8185656896257));
#5789=CARTESIAN_POINT('Ctrl Pts',(5.43047326528825,-3.07204060278614,24.8185615144177));
#5790=CARTESIAN_POINT('Ctrl Pts',(5.43060308003227,-3.07199944145218,24.8185530870008));
#5791=CARTESIAN_POINT('Ctrl Pts',(5.43066857802779,-3.07197867120643,24.818548834787));
#5792=CARTESIAN_POINT('Ctrl Pts',(5.43080079736073,-3.07193673812383,24.8185402506102));
#5793=CARTESIAN_POINT('Ctrl Pts',(5.4308675186954,-3.07191557520083,24.8185359186411));
#5794=CARTESIAN_POINT('Ctrl Pts',(5.4310022287794,-3.07187284252112,24.8185271720733));
#5795=CARTESIAN_POINT('Ctrl Pts',(5.4310702175018,-3.07185127268109,24.8185227574699));
#5796=CARTESIAN_POINT('Ctrl Pts',(5.43120750855455,-3.07180771123408,24.8185138426144));
#5797=CARTESIAN_POINT('Ctrl Pts',(5.43127681082203,-3.07178571955001,24.8185093423595));
#5798=CARTESIAN_POINT('Ctrl Pts',(5.4314167773327,-3.07174129877255,24.8185002530393));
#5799=CARTESIAN_POINT('Ctrl Pts',(5.43148744156385,-3.07171886958039,24.8184956639675));
#5800=CARTESIAN_POINT('Ctrl Pts',(5.43163018276345,-3.07167355736409,24.8184863936949));
#5801=CARTESIAN_POINT('Ctrl Pts',(5.43170225968432,-3.07165067424653,24.8184817124895));
#5802=CARTESIAN_POINT('Ctrl Pts',(5.43184787952696,-3.07160443694051,24.818472254467));
#5803=CARTESIAN_POINT('Ctrl Pts',(5.43192142242619,-3.07158108264431,24.8184674776432));
#5804=CARTESIAN_POINT('Ctrl Pts',(5.43207003015147,-3.07153388487311,24.8184578247266));
#5805=CARTESIAN_POINT('Ctrl Pts',(5.43214509496395,-3.0715100412807,24.8184529486261));
#5806=CARTESIAN_POINT('Ctrl Pts',(5.43229680530598,-3.07146184587413,24.8184430933109));
#5807=CARTESIAN_POINT('Ctrl Pts',(5.4323734508071,-3.07143749393993,24.818438114089));
#5808=CARTESIAN_POINT('Ctrl Pts',(5.43252838438359,-3.07138826180528,24.8184280484846));
#5809=CARTESIAN_POINT('Ctrl Pts',(5.43260667236773,-3.07136338149683,24.8184229620984));
#5810=CARTESIAN_POINT('Ctrl Pts',(5.44012829660415,-3.06897265549072,24.8179342582337));
#5811=CARTESIAN_POINT('Ctrl Pts',(5.44756277903329,-3.06657983646212,24.8174490996786));
#5812=CARTESIAN_POINT('Ctrl Pts',(5.46410833260847,-3.06118812759831,24.816364558583));
#5813=CARTESIAN_POINT('Ctrl Pts',(5.47321457565503,-3.05817563393195,24.8157644199452));
#5814=CARTESIAN_POINT('Ctrl Pts',(5.49964614648011,-3.04930053683947,24.8140133288337));
#5815=CARTESIAN_POINT('Ctrl Pts',(5.51693485844124,-3.04333114430815,24.8128564985214));
#5816=CARTESIAN_POINT('Ctrl Pts',(5.65146370021255,-2.99559595550017,24.8037702655541));
#5817=CARTESIAN_POINT('Ctrl Pts',(5.76623462366233,-2.94722153919545,24.7955186803279));
#5818=CARTESIAN_POINT('Ctrl Pts',(6.0362565760378,-2.81451939040535,24.7753119021079));
#5819=CARTESIAN_POINT('Ctrl Pts',(6.18795618391751,-2.723821825785,24.7632960451225));
#5820=CARTESIAN_POINT('Ctrl Pts',(6.41266011586314,-2.56308392031462,24.7449139354335));
#5821=CARTESIAN_POINT('Ctrl Pts',(6.49111351955375,-2.50126119380454,24.7383650553318));
#5822=CARTESIAN_POINT('Ctrl Pts',(6.59873347582763,-2.40803467484539,24.7292122340131));
#5823=CARTESIAN_POINT('Ctrl Pts',(6.63033702006829,-2.37954327292256,24.7265016329432));
#5824=CARTESIAN_POINT('Ctrl Pts',(6.68572408421306,-2.32758566401385,24.7217089657711));
#5825=CARTESIAN_POINT('Ctrl Pts',(6.70972391047598,-2.30436015006208,24.7196174031608));
#5826=CARTESIAN_POINT('Ctrl Pts',(6.74555005361194,-2.26859487589108,24.7164713455871));
#5827=CARTESIAN_POINT('Ctrl Pts',(6.75764337791683,-2.25632694533578,24.7154051197527));
#5828=CARTESIAN_POINT('Ctrl Pts',(6.77939841895775,-2.23390095371312,24.7134790340792));
#5829=CARTESIAN_POINT('Ctrl Pts',(6.78909325922473,-2.22377576063541,24.7126177472709));
#5830=CARTESIAN_POINT('Ctrl Pts',(6.80983816047952,-2.20182505765355,24.710768189018));
#5831=CARTESIAN_POINT('Ctrl Pts',(6.82086586360541,-2.18997887628746,24.7097808865825));
#5832=CARTESIAN_POINT('Ctrl Pts',(6.85051913469938,-2.15763965010232,24.7071144303846));
#5833=CARTESIAN_POINT('Ctrl Pts',(6.86897082773634,-2.13698851527668,24.7054425923759));
#5834=CARTESIAN_POINT('Ctrl Pts',(6.96326059272684,-2.0286814509089,24.6968282102518));
#5835=CARTESIAN_POINT('Ctrl Pts',(7.03460001662489,-1.93721377370374,24.6900709408979));
#5836=CARTESIAN_POINT('Ctrl Pts',(7.1142092148304,-1.82293180691672,24.6821034185282));
#5837=CARTESIAN_POINT('Ctrl Pts',(7.12734823766184,-1.80362622181835,24.6807727284219));
#5838=CARTESIAN_POINT('Ctrl Pts',(7.25999626248985,-1.6040937323485,24.6671638089495));
#5839=CARTESIAN_POINT('Ctrl Pts',(7.36128014951148,-1.41242599409194,24.6553304067686));
#5840=CARTESIAN_POINT('Ctrl Pts',(7.46904534215338,-1.14692822079476,24.6389675339684));
#5841=CARTESIAN_POINT('Ctrl Pts',(7.49334556596313,-1.08094406249499,24.6348992717646));
#5842=CARTESIAN_POINT('Ctrl Pts',(7.52851055709442,-0.974882875378807,24.6282812163858));
#5843=CARTESIAN_POINT('Ctrl Pts',(7.54079298548282,-0.935297352539703,24.6257940318784));
#5844=CARTESIAN_POINT('Ctrl Pts',(7.55595310793775,-0.882886501311716,24.6224653033926));
#5845=CARTESIAN_POINT('Ctrl Pts',(7.55952115770807,-0.870262950628422,24.6216608497017));
#5846=CARTESIAN_POINT('Ctrl Pts',(7.56524483441555,-0.849530127301381,24.6203346659984));
#5847=CARTESIAN_POINT('Ctrl Pts',(7.56744607541187,-0.84143345476036,24.6198155245752));
#5848=CARTESIAN_POINT('Ctrl Pts',(7.57167915405762,-0.825619527948426,24.6187989987597));
#5849=CARTESIAN_POINT('Ctrl Pts',(7.57371397129826,-0.817903229437207,24.6183017863248));
#5850=CARTESIAN_POINT('Ctrl Pts',(7.57819466377029,-0.800652234048019,24.6171876034298));
#5851=CARTESIAN_POINT('Ctrl Pts',(7.58062555277428,-0.791113739003178,24.6165697888871));
#5852=CARTESIAN_POINT('Ctrl Pts',(7.58888124715934,-0.758087941053018,24.6144249827482));
#5853=CARTESIAN_POINT('Ctrl Pts',(7.59448502020283,-0.734546927917138,24.6128861970076));
#5854=CARTESIAN_POINT('Ctrl Pts',(7.65056119171044,-0.486613497735651,24.5965914733977));
#5855=CARTESIAN_POINT('Ctrl Pts',(7.67713536569223,-0.257511450764323,24.580829062891));
#5856=CARTESIAN_POINT('Ctrl Pts',(7.6791798551556,-0.0183668891246562,24.5646956232636));
#5857=CARTESIAN_POINT('Ctrl Pts',(7.67921910619591,-0.00918318951676182,
24.5640764582002));
#5858=CARTESIAN_POINT('Ctrl Pts',(7.67921910621823,-7.83531977023612E-9,
24.5634577632816));
#5859=CARTESIAN_POINT('Origin',(4.45646910621825,-5.13094777615093E-16,
-2.31077344927308));
#5860=CARTESIAN_POINT('',(7.67921904725112,0.000460467671602397,23.3113459957337));
#5861=CARTESIAN_POINT('',(7.67921772993528,-0.00297839383558276,23.5607734493065));
#5862=CARTESIAN_POINT('',(7.67921910621823,-3.51191647465084E-13,-2.31077344927308));
#5863=CARTESIAN_POINT('Ctrl Pts',(7.67921772993528,-0.00297839383558212,
23.5607734493065));
#5864=CARTESIAN_POINT('Ctrl Pts',(7.67909389703478,-0.136970851418603,23.5690424041084));
#5865=CARTESIAN_POINT('Ctrl Pts',(7.67060927382305,-0.27059027499549,23.5773113589104));
#5866=CARTESIAN_POINT('Ctrl Pts',(7.65392828640833,-0.402954530335666,23.5855803137124));
#5867=CARTESIAN_POINT('Ctrl Pts',(7.63724729899361,-0.535318785675873,23.5938492685144));
#5868=CARTESIAN_POINT('Ctrl Pts',(7.61237013154434,-0.666428332467331,23.6021182233164));
#5869=CARTESIAN_POINT('Ctrl Pts',(7.57951436673159,-0.79542810063828,23.6103871781184));
#5870=CARTESIAN_POINT('Ctrl Pts',(7.55497886149549,-0.891760494830071,23.6165621366073));
#5871=CARTESIAN_POINT('Ctrl Pts',(7.52593914343194,-0.987124984549361,23.6227370950963));
#5872=CARTESIAN_POINT('Ctrl Pts',(7.49248746935389,-1.08106894377883,23.6289120535852));
#5873=CARTESIAN_POINT('Ctrl Pts',(7.45908096997117,-1.17488603671971,23.6350786731233));
#5874=CARTESIAN_POINT('Ctrl Pts',(7.42127450157948,-1.26728600695842,23.6412452926613));
#5875=CARTESIAN_POINT('Ctrl Pts',(7.3792108548205,-1.3578284992875,23.6474119121993));
#5876=CARTESIAN_POINT('Ctrl Pts',(7.33719161516261,-1.44827540481132,23.6535720215624));
#5877=CARTESIAN_POINT('Ctrl Pts',(7.29092431440421,-1.53686833969911,23.6597321309256));
#5878=CARTESIAN_POINT('Ctrl Pts',(7.24060053819386,-1.623185057837,23.6658922402887));
#5879=CARTESIAN_POINT('Ctrl Pts',(7.19031343251127,-1.70943887768212,23.6720478608301));
#5880=CARTESIAN_POINT('Ctrl Pts',(7.13597594635355,-1.79341940481737,23.6782034813714));
#5881=CARTESIAN_POINT('Ctrl Pts',(7.07782606176562,-1.87472805337289,23.6843591019128));
#5882=CARTESIAN_POINT('Ctrl Pts',(7.01969813170893,-1.95600600378896,23.6905123983952));
#5883=CARTESIAN_POINT('Ctrl Pts',(6.95776091550689,-2.03461372753706,23.6966656948775));
#5884=CARTESIAN_POINT('Ctrl Pts',(6.89229577913865,-2.11018150451315,23.7028189913599));
#5885=CARTESIAN_POINT('Ctrl Pts',(6.82683788981856,-2.1857409160699,23.7089716066669));
#5886=CARTESIAN_POINT('Ctrl Pts',(6.75785314097224,-2.25826072196952,23.7151242219739));
#5887=CARTESIAN_POINT('Ctrl Pts',(6.68566260354822,-2.3274049742066,23.7212768372809));
#5888=CARTESIAN_POINT('Ctrl Pts',(6.61346079385243,-2.39656002304986,23.7274304132949));
#5889=CARTESIAN_POINT('Ctrl Pts',(6.53805251472234,-2.46233817112081,23.7335839893089));
#5890=CARTESIAN_POINT('Ctrl Pts',(6.45979429750234,-2.52444166905603,23.7397375653229));
#5891=CARTESIAN_POINT('Ctrl Pts',(6.3814529974721,-2.58661109914914,23.7458976742788));
#5892=CARTESIAN_POINT('Ctrl Pts',(6.3002560581271,-2.6450978186819,23.7520577832347));
#5893=CARTESIAN_POINT('Ctrl Pts',(6.21659147482746,-2.69964568231117,23.7582178921907));
#5894=CARTESIAN_POINT('Ctrl Pts',(6.13288026769513,-2.75422394387428,23.7643814339957));
#5895=CARTESIAN_POINT('Ctrl Pts',(6.04669905209313,-2.80485875824551,23.7705449758007));
#5896=CARTESIAN_POINT('Ctrl Pts',(5.9584612529553,-2.85133953671605,23.7767085176057));
#5897=CARTESIAN_POINT('Ctrl Pts',(5.87007756186255,-2.89789716628332,23.7828822501812));
#5898=CARTESIAN_POINT('Ctrl Pts',(5.7796308883881,-2.94028685690416,23.7890559827568));
#5899=CARTESIAN_POINT('Ctrl Pts',(5.6875556021465,-2.97834578282021,23.7952297153323));
#5900=CARTESIAN_POINT('Ctrl Pts',(5.6195795009656,-3.00644341362332,23.7997875753982));
#5901=CARTESIAN_POINT('Ctrl Pts',(5.55071616800071,-3.03218162616531,23.8043454354641));
#5902=CARTESIAN_POINT('Ctrl Pts',(5.48114496854143,-3.05551254942147,23.8089032955301));
#5903=CARTESIAN_POINT('Ctrl Pts',(5.38688697092628,-3.08712226904296,23.8150784767338));
#5904=CARTESIAN_POINT('Ctrl Pts',(5.2910007126141,-3.11442140077743,23.8212536579376));
#5905=CARTESIAN_POINT('Ctrl Pts',(5.19391666630963,-3.13724220592148,23.8274288391413));
#5906=CARTESIAN_POINT('Ctrl Pts',(5.09696332521211,-3.16003228719099,23.8335957066379));
#5907=CARTESIAN_POINT('Ctrl Pts',(4.9988158201432,-3.17835592755096,23.8397625741344));
#5908=CARTESIAN_POINT('Ctrl Pts',(4.89992168927485,-3.19209451130136,23.8459294416309));
#5909=CARTESIAN_POINT('Ctrl Pts',(4.8011315641874,-3.20581864634668,23.8520898235063));
#5910=CARTESIAN_POINT('Ctrl Pts',(4.70159680186188,-3.21496725239346,23.8582502053816));
#5911=CARTESIAN_POINT('Ctrl Pts',(4.6017761575287,-3.21947253806261,23.864410587257));
#5912=CARTESIAN_POINT('Ctrl Pts',(4.502027676094,-3.22397456674545,23.8705665156346));
#5913=CARTESIAN_POINT('Ctrl Pts',(4.40199415571737,-3.22383992953218,23.8767224440122));
#5914=CARTESIAN_POINT('Ctrl Pts',(4.30213960679824,-3.21905265072018,23.8828783723899));
#5915=CARTESIAN_POINT('Ctrl Pts',(4.2023224068897,-3.21426716251391,23.8890319982401));
#5916=CARTESIAN_POINT('Ctrl Pts',(4.10268447833616,-3.20483251145545,23.8951856240904));
#5917=CARTESIAN_POINT('Ctrl Pts',(4.00368907718172,-3.19078482630928,23.9013392499406));
#5918=CARTESIAN_POINT('Ctrl Pts',(3.90470429658175,-3.17673864824528,23.9074922156095));
#5919=CARTESIAN_POINT('Ctrl Pts',(3.80636233590325,-3.15808048105445,23.9136451812784));
#5920=CARTESIAN_POINT('Ctrl Pts',(3.70911958060973,-3.1348981241936,23.9197981469472));
#5921=CARTESIAN_POINT('Ctrl Pts',(3.61186131853573,-3.11171207056667,23.9259520937965));
#5922=CARTESIAN_POINT('Ctrl Pts',(3.51570303210624,-3.08400049486412,23.9321060406459));
#5923=CARTESIAN_POINT('Ctrl Pts',(3.4210882167591,-3.05190169832559,23.9382599874952));
#5924=CARTESIAN_POINT('Ctrl Pts',(3.32637251284984,-3.01976867457416,23.944420496349));
#5925=CARTESIAN_POINT('Ctrl Pts',(3.23320397815096,-2.98323922807735,23.9505810052029));
#5926=CARTESIAN_POINT('Ctrl Pts',(3.14200819326913,-2.94250064924866,23.9567415140567));
#5927=CARTESIAN_POINT('Ctrl Pts',(3.05076134279166,-2.9017392586223,23.9629054725224));
#5928=CARTESIAN_POINT('Ctrl Pts',(2.96148982956291,-2.85676423698174,23.969069430988));
#5929=CARTESIAN_POINT('Ctrl Pts',(2.87459472566633,-2.80780893343071,23.9752333894537));
#5930=CARTESIAN_POINT('Ctrl Pts',(2.78755563881885,-2.75877251220157,23.9814075614398));
#5931=CARTESIAN_POINT('Ctrl Pts',(2.70290119425992,-2.7057428660593,23.987581733426));
#5932=CARTESIAN_POINT('Ctrl Pts',(2.62100367301257,-2.64899683012399,23.9937559054122));
#5933=CARTESIAN_POINT('Ctrl Pts',(2.56059031444356,-2.60713697204629,23.998310407922));
#5934=CARTESIAN_POINT('Ctrl Pts',(2.50167653506242,-2.56325571668601,24.0028649104318));
#5935=CARTESIAN_POINT('Ctrl Pts',(2.44439945696367,-2.51747756475572,24.0074194129417));
#5936=CARTESIAN_POINT('Ctrl Pts',(2.36686852340884,-2.45551171430765,24.0135844416614));
#5937=CARTESIAN_POINT('Ctrl Pts',(2.29206481509825,-2.38985060767553,24.0197494703812));
#5938=CARTESIAN_POINT('Ctrl Pts',(2.22036215039852,-2.32076350467566,24.025914499101));
#5939=CARTESIAN_POINT('Ctrl Pts',(2.1487566290135,-2.25177000140764,24.032071175393));
#5940=CARTESIAN_POINT('Ctrl Pts',(2.08024411192564,-2.17936002632762,24.0382278516851));
#5941=CARTESIAN_POINT('Ctrl Pts',(2.01516648640477,-2.10384388227637,24.0443845279771));
#5942=CARTESIAN_POINT('Ctrl Pts',(1.95015768402078,-2.02840760066442,24.0505346932483));
#5943=CARTESIAN_POINT('Ctrl Pts',(1.88857683437181,-1.94987200854449,24.0566848585195));
#5944=CARTESIAN_POINT('Ctrl Pts',(1.83072926894333,-1.86858445606488,24.0628350237907));
#5945=CARTESIAN_POINT('Ctrl Pts',(1.7729235628409,-1.78735572442136,24.0689807387144));
#5946=CARTESIAN_POINT('Ctrl Pts',(1.718846022187,-1.7033793449688,24.075126453638));
#5947=CARTESIAN_POINT('Ctrl Pts',(1.66876133744719,-1.61703523722687,24.0812721685616));
#5948=CARTESIAN_POINT('Ctrl Pts',(1.61869537709102,-1.53072340961621,24.0874155858822));
#5949=CARTESIAN_POINT('Ctrl Pts',(1.57261952503715,-1.44204598873221,24.0935590032028));
#5950=CARTESIAN_POINT('Ctrl Pts',(1.53075430939148,-1.35141055572641,24.0997024205234));
#5951=CARTESIAN_POINT('Ctrl Pts',(1.48889347922091,-1.26078461698518,24.1058451943072));
#5952=CARTESIAN_POINT('Ctrl Pts',(1.45124259119734,-1.16820146922694,24.1119879680911));
#5953=CARTESIAN_POINT('Ctrl Pts',(1.41797504454764,-1.0740909643472,24.118130741875));
#5954=CARTESIAN_POINT('Ctrl Pts',(1.38470203039162,-0.979964992448368,24.1242745252209));
#5955=CARTESIAN_POINT('Ctrl Pts',(1.35581393362782,-0.884311575459887,24.1304183085669));
#5956=CARTESIAN_POINT('Ctrl Pts',(1.33143473289778,-0.78757712515373,24.1365620919129));
#5957=CARTESIAN_POINT('Ctrl Pts',(1.30702907208843,-0.690737683660381,24.1427125434428));
#5958=CARTESIAN_POINT('Ctrl Pts',(1.28714218588264,-0.592815289057748,24.1488629949727));
#5959=CARTESIAN_POINT('Ctrl Pts',(1.27184717551692,-0.494267863608402,24.1550134465026));
#5960=CARTESIAN_POINT('Ctrl Pts',(1.25654347924464,-0.395664473912563,24.1611673908217));
#5961=CARTESIAN_POINT('Ctrl Pts',(1.24583689809394,-0.296435779492924,24.1673213351408));
#5962=CARTESIAN_POINT('Ctrl Pts',(1.23974853920379,-0.197044046461753,24.1734752794599));
#5963=CARTESIAN_POINT('Ctrl Pts',(1.23364990326623,-0.097484541856869,24.1796396115336));
#5964=CARTESIAN_POINT('Ctrl Pts',(1.23218506639979,0.00223811550083505,
24.1858039436072));
#5965=CARTESIAN_POINT('Ctrl Pts',(1.23532298439493,0.101662305514315,24.1919682756808));
#5966=CARTESIAN_POINT('Ctrl Pts',(1.23769296810425,0.176754679186507,24.1966240272384));
#5967=CARTESIAN_POINT('Ctrl Pts',(1.24268744706056,0.251676815485055,24.2012797787959));
#5968=CARTESIAN_POINT('Ctrl Pts',(1.25027362877931,0.326233233975295,24.2059355303534));
#5969=CARTESIAN_POINT('Ctrl Pts',(1.26035222960196,0.425284958358905,24.2121209162587));
#5970=CARTESIAN_POINT('Ctrl Pts',(1.27504260668428,0.524039787490354,24.218306302164));
#5971=CARTESIAN_POINT('Ctrl Pts',(1.29431956327251,0.62203523256157,24.2244916880692));
#5972=CARTESIAN_POINT('Ctrl Pts',(1.31357045045947,0.719898152430063,24.2306687091008));
#5973=CARTESIAN_POINT('Ctrl Pts',(1.33739550453645,0.817003309036331,24.2368457301323));
#5974=CARTESIAN_POINT('Ctrl Pts',(1.36571774450379,0.912892974318512,24.2430227511639));
#5975=CARTESIAN_POINT('Ctrl Pts',(1.39400995495996,1.00868096968411,24.2491932228222));
#5976=CARTESIAN_POINT('Ctrl Pts',(1.42678974872925,1.10325562373446,24.2553636944804));
#5977=CARTESIAN_POINT('Ctrl Pts',(1.46392922433137,1.19616997864699,24.2615341661387));
#5978=CARTESIAN_POINT('Ctrl Pts',(1.50104107533489,1.28901522322026,24.2677000481575));
#5979=CARTESIAN_POINT('Ctrl Pts',(1.54250599988026,1.38020222406898,24.2738659301763));
#5980=CARTESIAN_POINT('Ctrl Pts',(1.58814673392486,1.46930062652308,24.2800318121951));
#5981=CARTESIAN_POINT('Ctrl Pts',(1.63376978006936,1.55836449921611,24.2861953046488));
#5982=CARTESIAN_POINT('Ctrl Pts',(1.68356522275971,1.64534099769534,24.2923587971025));
#5983=CARTESIAN_POINT('Ctrl Pts',(1.73730863917843,1.72982193216171,24.2985222895562));
#5984=CARTESIAN_POINT('Ctrl Pts',(1.79104544092444,1.81429246881996,24.304685023415));
#5985=CARTESIAN_POINT('Ctrl Pts',(1.84872901811546,1.89626768742934,24.3108477572737));
#5986=CARTESIAN_POINT('Ctrl Pts',(1.91009069429663,1.97536693953287,24.3170104911324));
#5987=CARTESIAN_POINT('Ctrl Pts',(1.97146104600473,2.05447737496341,24.3231740962999));
#5988=CARTESIAN_POINT('Ctrl Pts',(2.036510264532,2.130710694613,24.3293377014673));
#5989=CARTESIAN_POINT('Ctrl Pts',(2.10492895072005,2.20371877960402,24.3355013066348));
#5990=CARTESIAN_POINT('Ctrl Pts',(2.17341794194965,2.2768018855686,24.3416712453427));
#5991=CARTESIAN_POINT('Ctrl Pts',(2.24528301873515,2.34665282264687,24.3478411840506));
#5992=CARTESIAN_POINT('Ctrl Pts',(2.32017750797366,2.41295996024995,24.3540111227586));
#5993=CARTESIAN_POINT('Ctrl Pts',(2.39511249935403,2.47930295604664,24.3601843981036));
#5994=CARTESIAN_POINT('Ctrl Pts',(2.47307982966312,2.54209806376006,24.3663576734486));
#5995=CARTESIAN_POINT('Ctrl Pts',(2.55370089840971,2.60107491431004,24.3725309487937));
#5996=CARTESIAN_POINT('Ctrl Pts',(2.6344517129546,2.66014667799717,24.3787141589678));
#5997=CARTESIAN_POINT('Ctrl Pts',(2.71786443605039,2.71538767138475,24.3848973691419));
#5998=CARTESIAN_POINT('Ctrl Pts',(2.80353265476014,2.76657164193175,24.391080579316));
#5999=CARTESIAN_POINT('Ctrl Pts',(2.86528459180756,2.80346641311598,24.3955376021323));
#6000=CARTESIAN_POINT('Ctrl Pts',(2.92820790224037,2.83825413743604,24.3999946249486));
#6001=CARTESIAN_POINT('Ctrl Pts',(2.99214374432667,2.87086551357269,24.404451647765));
#6002=CARTESIAN_POINT('Ctrl Pts',(3.08081877140353,2.91609545921145,24.4106332605509));
#6003=CARTESIAN_POINT('Ctrl Pts',(3.17174214636608,2.9572900072321,24.4168148733368));
#6004=CARTESIAN_POINT('Ctrl Pts',(3.26451146915699,2.99422019129376,24.4229964861227));
#6005=CARTESIAN_POINT('Ctrl Pts',(3.35715775456585,3.03110139587569,24.4291699004069));
#6006=CARTESIAN_POINT('Ctrl Pts',(3.45164472248631,3.06372932025985,24.4353433146911));
#6007=CARTESIAN_POINT('Ctrl Pts',(3.54754596933506,3.0919211331692,24.4415167289753));
#6008=CARTESIAN_POINT('Ctrl Pts',(3.64334809226331,3.12008380690557,24.4476837623933));
#6009=CARTESIAN_POINT('Ctrl Pts',(3.740561174617,3.14381936444606,24.4538507958112));
#6010=CARTESIAN_POINT('Ctrl Pts',(3.83874033576257,3.16299363398841,24.4600178292292));
#6011=CARTESIAN_POINT('Ctrl Pts',(3.9368506262569,3.18215445317719,24.4661805366007));
#6012=CARTESIAN_POINT('Ctrl Pts',(4.03592522462356,3.19676026336572,24.4723432439723));
#6013=CARTESIAN_POINT('Ctrl Pts',(4.135506506055,3.20672739280974,24.4785059513438));
#6014=CARTESIAN_POINT('Ctrl Pts',(4.23505180336641,3.2166909205891,24.4846664317949));
#6015=CARTESIAN_POINT('Ctrl Pts',(4.3351029897508,3.22201905553797,24.4908269122459));
#6016=CARTESIAN_POINT('Ctrl Pts',(4.43519559393369,3.22267978554727,24.4969873926969));
#6017=CARTESIAN_POINT('Ctrl Pts',(4.53527855446147,3.223340451897,24.503147279602));
#6018=CARTESIAN_POINT('Ctrl Pts',(4.63540249211706,3.21933460465401,24.5093071665072));
#6019=CARTESIAN_POINT('Ctrl Pts',(4.73510218792276,3.21068235244157,24.5154670534124));
#6020=CARTESIAN_POINT('Ctrl Pts',(4.83481869861019,3.20202864098098,24.5216279792151));
#6021=CARTESIAN_POINT('Ctrl Pts',(4.9341103941629,3.18872700520829,24.5277889050178));
#6022=CARTESIAN_POINT('Ctrl Pts',(5.03251741807506,3.17084939801732,24.5339498308205));
#6023=CARTESIAN_POINT('Ctrl Pts',(5.13102996180132,3.15295262103835,24.5401173628564));
#6024=CARTESIAN_POINT('Ctrl Pts',(5.22865551306772,3.13047015211669,24.5462848948923));
#6025=CARTESIAN_POINT('Ctrl Pts',(5.32494475491672,3.10352502972309,24.5524524269282));
#6026=CARTESIAN_POINT('Ctrl Pts',(5.42128840259861,3.07656468266058,24.5586234437741));
#6027=CARTESIAN_POINT('Ctrl Pts',(5.51629382624657,3.04513679608577,24.56479446062));
#6028=CARTESIAN_POINT('Ctrl Pts',(5.60952918659088,3.00941356638647,24.570965477466));
#6029=CARTESIAN_POINT('Ctrl Pts',(5.70291860022974,2.97363131099987,24.5771466907167));
#6030=CARTESIAN_POINT('Ctrl Pts',(5.79453171212724,2.93353970981319,24.5833279039674));
#6031=CARTESIAN_POINT('Ctrl Pts',(5.88395876826429,2.88935820334752,24.5895091172182));
#6032=CARTESIAN_POINT('Ctrl Pts',(5.94886335455936,2.85729204213281,24.5939953332044));
#6033=CARTESIAN_POINT('Ctrl Pts',(6.01261690397324,2.82307246632287,24.5984815491906));
#6034=CARTESIAN_POINT('Ctrl Pts',(6.07507241288918,2.786797606238,24.6029677651768));
#6035=CARTESIAN_POINT('Ctrl Pts',(6.16010017957156,2.73741252566994,24.6090753597314));
#6036=CARTESIAN_POINT('Ctrl Pts',(6.24303275959794,2.68403523352434,24.615182954286));
#6037=CARTESIAN_POINT('Ctrl Pts',(6.32346502031454,2.62686958550433,24.6212905488406));
#6038=CARTESIAN_POINT('Ctrl Pts',(6.40378701967242,2.5697823035773,24.6273897707389));
#6039=CARTESIAN_POINT('Ctrl Pts',(6.48161515029577,2.50891723703554,24.6334889926373));
#6040=CARTESIAN_POINT('Ctrl Pts',(6.55656931445129,2.44452381413629,24.6395882145356));
#6041=CARTESIAN_POINT('Ctrl Pts',(6.63144399715611,2.38019867406997,24.6456809688145));
#6042=CARTESIAN_POINT('Ctrl Pts',(6.70345043414893,2.31235289968939,24.6517737230935));
#6043=CARTESIAN_POINT('Ctrl Pts',(6.77223885675924,2.24127821231083,24.6578664773724));
#6044=CARTESIAN_POINT('Ctrl Pts',(6.84098018235994,2.17025218726681,24.6639550601571));
#6045=CARTESIAN_POINT('Ctrl Pts',(6.90650756235692,2.09600195888477,24.6700436429419));
#6046=CARTESIAN_POINT('Ctrl Pts',(6.96850635226542,2.01885770597426,24.6761322257266));
#6047=CARTESIAN_POINT('Ctrl Pts',(7.03048353194658,1.94174034237636,24.6822186862819));
#6048=CARTESIAN_POINT('Ctrl Pts',(7.08893428566251,1.86173130306404,24.6883051468372));
#6049=CARTESIAN_POINT('Ctrl Pts',(7.14358343474165,1.77919480325909,24.6943916073924));
#6050=CARTESIAN_POINT('Ctrl Pts',(7.19822887921723,1.69666389850942,24.7004776553535));
#6051=CARTESIAN_POINT('Ctrl Pts',(7.24907298573405,1.61160624405079,24.7065637033145));
#6052=CARTESIAN_POINT('Ctrl Pts',(7.29588385742796,1.52441511180931,24.7126497512756));
#6053=CARTESIAN_POINT('Ctrl Pts',(7.34270469983793,1.43720540785595,24.7187370955649));
#6054=CARTESIAN_POINT('Ctrl Pts',(7.38549039142958,1.34786171514762,24.7248244398542));
#6055=CARTESIAN_POINT('Ctrl Pts',(7.42405548868829,1.25680094886909,24.7309117841435));
#6056=CARTESIAN_POINT('Ctrl Pts',(7.46266779211284,1.16562871834078,24.7370065797348));
#6057=CARTESIAN_POINT('Ctrl Pts',(7.49704901294095,1.07273562774361,24.7431013753261));
#6058=CARTESIAN_POINT('Ctrl Pts',(7.52706235794148,0.978557430594477,24.7491961709173));
#6059=CARTESIAN_POINT('Ctrl Pts',(7.55709454086888,0.884320122340259,24.7552947919174));
#6060=CARTESIAN_POINT('Ctrl Pts',(7.58275327840586,0.788796531362502,24.7613934129174));
#6061=CARTESIAN_POINT('Ctrl Pts',(7.6039526371208,0.692434101700029,24.7674920339174));
#6062=CARTESIAN_POINT('Ctrl Pts',(7.62519206241875,0.595889547977125,24.7736021812522));
#6063=CARTESIAN_POINT('Ctrl Pts',(7.64195520212604,0.49850342701961,24.779712328587));
#6064=CARTESIAN_POINT('Ctrl Pts',(7.65420784391407,0.40072999381057,24.7858224759218));
#6065=CARTESIAN_POINT('Ctrl Pts',(7.66467641885284,0.31719302845427,24.7910429448106));
#6066=CARTESIAN_POINT('Ctrl Pts',(7.67185326443048,0.233373553073914,24.7962634136995));
#6067=CARTESIAN_POINT('Ctrl Pts',(7.67574717225487,0.149553656041532,24.8014838825884));
#6068=CARTESIAN_POINT('Ctrl Pts',(7.67805684450647,0.0998358663457391,24.8045804048166));
#6069=CARTESIAN_POINT('Ctrl Pts',(7.67921437958694,0.0500747491672077,24.8076769270449));
#6070=CARTESIAN_POINT('Ctrl Pts',(7.67921909177339,0.000305129896709012,
24.8107734492731));
#6071=CARTESIAN_POINT('Ctrl Pts',(7.67921910621823,-7.83532877468573E-9,
24.5634577632816));
#6072=CARTESIAN_POINT('Ctrl Pts',(7.67921910654256,0.133398137250487,24.55447038207));
#6073=CARTESIAN_POINT('Ctrl Pts',(7.67093661792531,0.266687541275268,24.5455903586593));
#6074=CARTESIAN_POINT('Ctrl Pts',(7.64446499824392,0.478801730918038,24.5317288342665));
#6075=CARTESIAN_POINT('Ctrl Pts',(7.63154154501361,0.558109087832411,24.5266057187726));
#6076=CARTESIAN_POINT('Ctrl Pts',(7.6109501571527,0.660254942829582,24.5200814270419));
#6077=CARTESIAN_POINT('Ctrl Pts',(7.60597344436133,0.68360058794858,24.5185952796626));
#6078=CARTESIAN_POINT('Ctrl Pts',(7.59743332482478,0.721587341298214,24.5161847776374));
#6079=CARTESIAN_POINT('Ctrl Pts',(7.59402587349456,0.73626222108192,24.5152554396569));
#6080=CARTESIAN_POINT('Ctrl Pts',(7.58724719352546,0.764554049600949,24.5134672049344));
#6081=CARTESIAN_POINT('Ctrl Pts',(7.58388972074766,0.778173911431171,24.5126078862052));
#6082=CARTESIAN_POINT('Ctrl Pts',(7.57594344365583,0.809526343791456,24.5106331327956));
#6083=CARTESIAN_POINT('Ctrl Pts',(7.57129215056274,0.827242689466017,24.5095197524271));
#6084=CARTESIAN_POINT('Ctrl Pts',(7.55579185650502,0.884296980967118,24.5059415058436));
#6085=CARTESIAN_POINT('Ctrl Pts',(7.54434644538047,0.923469775651678,24.503496061915));
#6086=CARTESIAN_POINT('Ctrl Pts',(7.45978181912304,1.1937215414841,24.4866818717166));
#6087=CARTESIAN_POINT('Ctrl Pts',(7.36154371908736,1.41612668337206,24.4732126560994));
#6088=CARTESIAN_POINT('Ctrl Pts',(7.17043897046691,1.74330707275403,24.4520424700107));
#6089=CARTESIAN_POINT('Ctrl Pts',(7.09417473773427,1.85667861022511,24.4443951695889));
#6090=CARTESIAN_POINT('Ctrl Pts',(6.98524905950513,1.99829124616426,24.4339826033436));
#6091=CARTESIAN_POINT('Ctrl Pts',(6.95888555596945,2.03120839320807,24.4314961089902));
#6092=CARTESIAN_POINT('Ctrl Pts',(6.91357926587741,2.08555616652858,24.4272601994819));
#6093=CARTESIAN_POINT('Ctrl Pts',(6.89498281490939,2.10726970834283,24.4255314657325));
#6094=CARTESIAN_POINT('Ctrl Pts',(6.86862376262849,2.13723082725154,24.4230900734091));
#6095=CARTESIAN_POINT('Ctrl Pts',(6.86110221523411,2.14568993506357,24.4223944134373));
#6096=CARTESIAN_POINT('Ctrl Pts',(6.848205306685,2.16004146334287,24.4212029132762));
#6097=CARTESIAN_POINT('Ctrl Pts',(6.84285237837223,2.16595384375363,24.4207087515198));
#6098=CARTESIAN_POINT('Ctrl Pts',(6.8324400903726,2.17736889792201,24.4197481527618));
#6099=CARTESIAN_POINT('Ctrl Pts',(6.82738360139083,2.1828737684702,24.4192819575488));
#6100=CARTESIAN_POINT('Ctrl Pts',(6.81366528474199,2.19770465287964,24.4180180885247));
#6101=CARTESIAN_POINT('Ctrl Pts',(6.8049673911384,2.20699690946801,24.4172177393123));
#6102=CARTESIAN_POINT('Ctrl Pts',(6.77208273732516,2.24171418989512,24.4141963364709));
#6103=CARTESIAN_POINT('Ctrl Pts',(6.74753723499033,2.26679412232575,24.4119502400114));
#6104=CARTESIAN_POINT('Ctrl Pts',(6.56568147246832,2.44663822679667,24.3954075287975));
#6105=CARTESIAN_POINT('Ctrl Pts',(6.3932617278536,2.58527373241151,24.38029358379));
#6106=CARTESIAN_POINT('Ctrl Pts',(6.03496079596833,2.81726784732446,24.351531859574));
#6107=CARTESIAN_POINT('Ctrl Pts',(5.85149780740907,2.91248285752567,24.3379201401605));
#6108=CARTESIAN_POINT('Ctrl Pts',(5.63206400410108,3.00083517689787,24.3230280181732));
#6109=CARTESIAN_POINT('Ctrl Pts',(5.60380605825753,3.01175250340107,24.3211342891187));
#6110=CARTESIAN_POINT('Ctrl Pts',(5.55987354177247,3.02801754343669,24.3182262270692));
#6111=CARTESIAN_POINT('Ctrl Pts',(5.54430521039196,3.03364536795737,24.3172026307065));
#6112=CARTESIAN_POINT('Ctrl Pts',(5.51682990130281,3.04333876243206,24.3154081157189));
#6113=CARTESIAN_POINT('Ctrl Pts',(5.5049412920116,3.04745499087098,24.3146355361345));
#6114=CARTESIAN_POINT('Ctrl Pts',(5.47773917230597,3.05669523508705,24.3128765762331));
#6115=CARTESIAN_POINT('Ctrl Pts',(5.46241056544166,3.06177401247868,24.3118917004727));
#6116=CARTESIAN_POINT('Ctrl Pts',(5.42073155492803,3.07523658993525,24.3092304530469));
#6117=CARTESIAN_POINT('Ctrl Pts',(5.39431000938255,3.08339693622049,24.3075613902145));
#6118=CARTESIAN_POINT('Ctrl Pts',(5.2563240840812,3.12407636399447,24.2989331680923));
#6119=CARTESIAN_POINT('Ctrl Pts',(5.14315948960798,3.15088585056849,24.2921602930875));
#6120=CARTESIAN_POINT('Ctrl Pts',(4.80502376972901,3.21190383241823,24.2725051494874));
#6121=CARTESIAN_POINT('Ctrl Pts',(4.57763074893569,3.22848741839149,24.260068817103));
#6122=CARTESIAN_POINT('Ctrl Pts',(4.23942743565147,3.21734935897173,24.2407925493243));
#6123=CARTESIAN_POINT('Ctrl Pts',(4.1287377143078,3.20796365079108,24.2343483313036));
#6124=CARTESIAN_POINT('Ctrl Pts',(4.0013995304929,3.19050724816095,24.2265566520593));
#6125=CARTESIAN_POINT('Ctrl Pts',(3.98405336392011,3.18798496772045,24.2254870362918));
#6126=CARTESIAN_POINT('Ctrl Pts',(3.95746644239923,3.18389725471876,24.2238337873915));
#6127=CARTESIAN_POINT('Ctrl Pts',(3.94821019534125,3.18243275835619,24.2232556304219));
#6128=CARTESIAN_POINT('Ctrl Pts',(3.93121500973005,3.17966779377962,24.2221891328721));
#6129=CARTESIAN_POINT('Ctrl Pts',(3.92347431360627,3.17837941287616,24.2217014723261));
#6130=CARTESIAN_POINT('Ctrl Pts',(3.90597365221809,3.17540082966504,24.2205946120525));
#6131=CARTESIAN_POINT('Ctrl Pts',(3.89621681671857,3.17369391087221,24.2199744976119));
#6132=CARTESIAN_POINT('Ctrl Pts',(3.87095563806481,3.16915445350731,24.2183614013051));
#6133=CARTESIAN_POINT('Ctrl Pts',(3.8554641348447,3.16625314414301,24.2173647581553));
#6134=CARTESIAN_POINT('Ctrl Pts',(3.75207556233731,3.14610405004485,24.2106665182324));
#6135=CARTESIAN_POINT('Ctrl Pts',(3.6649167069486,3.12531322144643,24.2047943217843));
#6136=CARTESIAN_POINT('Ctrl Pts',(3.49824257715581,3.0781357105749,24.1932634380833));
#6137=CARTESIAN_POINT('Ctrl Pts',(3.41865995070935,3.05222357901309,24.1876202786106));
#6138=CARTESIAN_POINT('Ctrl Pts',(3.21783871704433,2.97807318543374,24.1731462931991));
#6139=CARTESIAN_POINT('Ctrl Pts',(3.09834806755375,2.92551452563916,24.1643134491597));
#6140=CARTESIAN_POINT('Ctrl Pts',(2.84947139525583,2.79750066554015,24.1456798039763));
#6141=CARTESIAN_POINT('Ctrl Pts',(2.72147695377286,2.71997515267977,24.135951483536));
#6142=CARTESIAN_POINT('Ctrl Pts',(2.57750302450599,2.61845680374688,24.1248663022953));
#6143=CARTESIAN_POINT('Ctrl Pts',(2.55588693723755,2.60280945461253,24.1231975441654));
#6144=CARTESIAN_POINT('Ctrl Pts',(2.52058378264626,2.57658004411053,24.120464163127));
#6145=CARTESIAN_POINT('Ctrl Pts',(2.50678347132565,2.56615327942101,24.1193936036624));
#6146=CARTESIAN_POINT('Ctrl Pts',(2.48199734095253,2.54711085223847,24.1174668350946));
#6147=CARTESIAN_POINT('Ctrl Pts',(2.47098237457753,2.53853400481894,24.1166091328642));
#6148=CARTESIAN_POINT('Ctrl Pts',(2.44747082321841,2.5199799902538,24.1147750609654));
#6149=CARTESIAN_POINT('Ctrl Pts',(2.43499202460595,2.50998081173809,24.1137995971346));
#6150=CARTESIAN_POINT('Ctrl Pts',(2.40105431348308,2.48236947813517,24.1111407177066));
#6151=CARTESIAN_POINT('Ctrl Pts',(2.37974741680168,2.46457203058154,24.1094647950051));
#6152=CARTESIAN_POINT('Ctrl Pts',(2.25928453500097,2.36127895894633,24.0999461889107));
#6153=CARTESIAN_POINT('Ctrl Pts',(2.1651753804256,2.2700742779802,24.0923460839043));
#6154=CARTESIAN_POINT('Ctrl Pts',(1.97934575504301,2.06661287841548,24.0766597395672));
#6155=CARTESIAN_POINT('Ctrl Pts',(1.88911904706794,1.95339294522926,24.0686244308601));
#6156=CARTESIAN_POINT('Ctrl Pts',(1.71200680732183,1.69757953819521,24.0511990055546));
#6157=CARTESIAN_POINT('Ctrl Pts',(1.62797877074432,1.55353743329028,24.0418132318677));
#6158=CARTESIAN_POINT('Ctrl Pts',(1.54371469093157,1.37938646720165,24.0302157365546));
#6159=CARTESIAN_POINT('Ctrl Pts',(1.53227074438938,1.35495724740963,24.0285832605212));
#6160=CARTESIAN_POINT('Ctrl Pts',(1.51687343786853,1.32098503059886,24.0263014524716));
#6161=CARTESIAN_POINT('Ctrl Pts',(1.5126569081527,1.3115616189237,24.025667286771));
#6162=CARTESIAN_POINT('Ctrl Pts',(1.50549537042113,1.2953479658597,24.0245737901254));
#6163=CARTESIAN_POINT('Ctrl Pts',(1.50252831256744,1.2885674708854,24.0241157857353));
#6164=CARTESIAN_POINT('Ctrl Pts',(1.49637046501007,1.27436215665442,24.0231546543602));
#6165=CARTESIAN_POINT('Ctrl Pts',(1.49318422720338,1.26693551241192,24.0226512461872));
#6166=CARTESIAN_POINT('Ctrl Pts',(1.48544866632388,1.24871625556839,24.0214141498326));
#6167=CARTESIAN_POINT('Ctrl Pts',(1.48093020615531,1.23791073403787,24.0206786362247));
#6168=CARTESIAN_POINT('Ctrl Pts',(1.46473141899791,1.19857155675043,24.0179949465732));
#6169=CARTESIAN_POINT('Ctrl Pts',(1.45340223066768,1.16989629621508,24.0160274460453));
#6170=CARTESIAN_POINT('Ctrl Pts',(1.42598684590726,1.09748188724091,24.0110384707653));
#6171=CARTESIAN_POINT('Ctrl Pts',(1.41043507441013,1.05354898319761,24.0079933141749));
#6172=CARTESIAN_POINT('Ctrl Pts',(1.29247241423753,0.695834836972181,23.9831331591239));
#6173=CARTESIAN_POINT('Ctrl Pts',(1.23785653150625,0.368329752488542,23.9602364645673));
#6174=CARTESIAN_POINT('Ctrl Pts',(1.23312726365507,-0.0308683449592165,
23.9344779737535));
#6175=CARTESIAN_POINT('Ctrl Pts',(1.23452847054092,-0.0999259677591112,
23.9300870358221));
#6176=CARTESIAN_POINT('Ctrl Pts',(1.23937946453772,-0.192365335190156,23.924293281993));
#6177=CARTESIAN_POINT('Ctrl Pts',(1.240868255887,-0.215827253189526,23.9228299757338));
#6178=CARTESIAN_POINT('Ctrl Pts',(1.24373087264865,-0.25427748434757,23.9204431962415));
#6179=CARTESIAN_POINT('Ctrl Pts',(1.24495318439968,-0.269275867196935,23.9195150117187));
#6180=CARTESIAN_POINT('Ctrl Pts',(1.24752954412871,-0.298370516814858,23.9177197841499));
#6181=CARTESIAN_POINT('Ctrl Pts',(1.24887153732137,-0.312467477605069,23.9168523844858));
#6182=CARTESIAN_POINT('Ctrl Pts',(1.25223585301616,-0.345498768004624,23.9148254069702));
#6183=CARTESIAN_POINT('Ctrl Pts',(1.25433317167555,-0.364425054633693,23.9136682106925));
#6184=CARTESIAN_POINT('Ctrl Pts',(1.26175909587514,-0.426413100473815,23.9098911097947));
#6185=CARTESIAN_POINT('Ctrl Pts',(1.26778971827805,-0.469387061127087,23.9072932539876));
#6186=CARTESIAN_POINT('Ctrl Pts',(1.28416572602259,-0.571109189977421,23.90118383744));
#6187=CARTESIAN_POINT('Ctrl Pts',(1.29527791424737,-0.62971842405922,23.8976957423725));
#6188=CARTESIAN_POINT('Ctrl Pts',(1.34480149666502,-0.856354511157959,23.8842799581829));
#6189=CARTESIAN_POINT('Ctrl Pts',(1.39503996703573,-1.02150610204247,23.8746768723953));
#6190=CARTESIAN_POINT('Ctrl Pts',(1.5261409338791,-1.35409448013365,23.8546853918375));
#6191=CARTESIAN_POINT('Ctrl Pts',(1.60874442609311,-1.52014528492112,23.8443239016441));
#6192=CARTESIAN_POINT('Ctrl Pts',(1.71905233573639,-1.70099443381679,23.8316230827937));
#6193=CARTESIAN_POINT('Ctrl Pts',(1.73326007906393,-1.72364878329798,23.8300047026801));
#6194=CARTESIAN_POINT('Ctrl Pts',(1.75332135546355,-1.75476939506296,23.8277394906023));
#6195=CARTESIAN_POINT('Ctrl Pts',(1.7589364456938,-1.76338904697531,23.827107554198));
#6196=CARTESIAN_POINT('Ctrl Pts',(1.76865465225191,-1.77815230001433,23.8260171369178));
#6197=CARTESIAN_POINT('Ctrl Pts',(1.77273784267574,-1.78430901009029,23.825559970107));
#6198=CARTESIAN_POINT('Ctrl Pts',(1.78133944053119,-1.79718234012883,23.8245988331067));
#6199=CARTESIAN_POINT('Ctrl Pts',(1.78586202119365,-1.80389602929368,23.8240945717922));
#6200=CARTESIAN_POINT('Ctrl Pts',(1.79701588126895,-1.82031985352653,23.822853725263));
#6201=CARTESIAN_POINT('Ctrl Pts',(1.80367506272029,-1.83001081350776,23.8221152945784));
#6202=CARTESIAN_POINT('Ctrl Pts',(1.82813767841435,-1.86519661730689,23.8194119433302));
#6203=CARTESIAN_POINT('Ctrl Pts',(1.84625619688889,-1.89046896743857,23.8174273643497));
#6204=CARTESIAN_POINT('Ctrl Pts',(1.89274839673714,-1.95337524221768,23.8123865199626));
#6205=CARTESIAN_POINT('Ctrl Pts',(1.92158668453334,-1.99065551233131,23.8093060134129));
#6206=CARTESIAN_POINT('Ctrl Pts',(2.1674461520701,-2.29447846049972,23.7835024547909));
#6207=CARTESIAN_POINT('Ctrl Pts',(2.4250974826434,-2.52544595311274,23.7596454164184));
#6208=CARTESIAN_POINT('Ctrl Pts',(2.76308037760481,-2.74260887281112,23.7338807711373));
#6209=CARTESIAN_POINT('Ctrl Pts',(2.81262017722566,-2.77258547351449,23.7302143476471));
#6210=CARTESIAN_POINT('Ctrl Pts',(2.88204548641158,-2.8120794446459,23.7252226884356));
#6211=CARTESIAN_POINT('Ctrl Pts',(2.90125864001196,-2.82275060566896,23.7238562924268));
#6212=CARTESIAN_POINT('Ctrl Pts',(2.93223923746065,-2.839545167929,23.7216765816477));
#6213=CARTESIAN_POINT('Ctrl Pts',(2.94393767903226,-2.84579376337713,23.7208588301228));
#6214=CARTESIAN_POINT('Ctrl Pts',(2.9682186639187,-2.85857116657437,23.7191723551825));
#6215=CARTESIAN_POINT('Ctrl Pts',(2.98080639658954,-2.86508953977177,23.7183040139281));
#6216=CARTESIAN_POINT('Ctrl Pts',(3.01039774288975,-2.88016623145105,23.7162764050665));
#6217=CARTESIAN_POINT('Ctrl Pts',(3.02743510150431,-2.88865742968223,23.7151195061843));
#6218=CARTESIAN_POINT('Ctrl Pts',(3.0834384156425,-2.91595200733911,23.7113500450175));
#6219=CARTESIAN_POINT('Ctrl Pts',(3.12270889400311,-2.93412224520004,23.7087593442097));
#6220=CARTESIAN_POINT('Ctrl Pts',(3.21673579953138,-2.9753499504563,23.7026705067408));
#6221=CARTESIAN_POINT('Ctrl Pts',(3.27178795144855,-2.99769530742523,23.6991955545032));
#6222=CARTESIAN_POINT('Ctrl Pts',(3.48767360077728,-3.07844502793879,23.6858620576207));
#6223=CARTESIAN_POINT('Ctrl Pts',(3.65244420321299,-3.12552990617507,23.6763226324518));
#6224=CARTESIAN_POINT('Ctrl Pts',(4.00285808221847,-3.19610394970807,23.6563291487158));
#6225=CARTESIAN_POINT('Ctrl Pts',(4.18836302177209,-3.21697758626017,23.6459026342698));
#6226=CARTESIAN_POINT('Ctrl Pts',(4.40132462819749,-3.22238903636769,23.6331292496831));
#6227=CARTESIAN_POINT('Ctrl Pts',(4.4280516836664,-3.22273553989994,23.6315114958831));
#6228=CARTESIAN_POINT('Ctrl Pts',(4.46507406513482,-3.22275495599412,23.629246468284));
#6229=CARTESIAN_POINT('Ctrl Pts',(4.47536897418246,-3.22271102334964,23.6286140434918));
#6230=CARTESIAN_POINT('Ctrl Pts',(4.49306074250226,-3.22255075069525,23.6275225153997));
#6231=CARTESIAN_POINT('Ctrl Pts',(4.50045781112537,-3.22245826658705,23.6270647241671));
#6232=CARTESIAN_POINT('Ctrl Pts',(4.51595296662926,-3.22221117187929,23.6261026714121));
#6233=CARTESIAN_POINT('Ctrl Pts',(4.52405084167679,-3.22205150017221,23.6255981201071));
#6234=CARTESIAN_POINT('Ctrl Pts',(4.54391884716972,-3.22158481766088,23.6243559890034));
#6235=CARTESIAN_POINT('Ctrl Pts',(4.55568799583006,-3.22124382753291,23.6236165566525));
#6236=CARTESIAN_POINT('Ctrl Pts',(4.59863614834341,-3.21976389287901,23.6209055866183));
#6237=CARTESIAN_POINT('Ctrl Pts',(4.62979892885478,-3.2182367218773,23.6189142512396));
#6238=CARTESIAN_POINT('Ctrl Pts',(4.70818035143695,-3.21325385279514,23.6138525388621));
#6239=CARTESIAN_POINT('Ctrl Pts',(4.75535319884567,-3.20920967136437,23.6107576831234));
#6240=CARTESIAN_POINT('Ctrl Pts',(4.96993516516813,-3.18604135726999,23.5965064470594));
#6241=CARTESIAN_POINT('Ctrl Pts',(5.13577049462276,-3.15484598423149,23.5850257969416));
#6242=CARTESIAN_POINT('Ctrl Pts',(5.48946455598691,-3.05912033773592,23.5603031253992));
#6243=CARTESIAN_POINT('Ctrl Pts',(5.67538408925436,-2.98991072380797,23.5471700463777));
#6244=CARTESIAN_POINT('Ctrl Pts',(5.89076082274076,-2.88627911910194,23.5319977510812));
#6245=CARTESIAN_POINT('Ctrl Pts',(5.92737937704093,-2.86779063142463,23.5294180261197));
#6246=CARTESIAN_POINT('Ctrl Pts',(5.97884943753798,-2.84055838041974,23.5257903727994));
#6247=CARTESIAN_POINT('Ctrl Pts',(5.99399796960811,-2.83238747321706,23.524722472469));
#6248=CARTESIAN_POINT('Ctrl Pts',(6.0215879477259,-2.81721924808184,23.5227768774217));
#6249=CARTESIAN_POINT('Ctrl Pts',(6.03404967696782,-2.81025992268162,23.5218978601141));
#6250=CARTESIAN_POINT('Ctrl Pts',(6.05893793797852,-2.7961432069557,23.5201416554475));
#6251=CARTESIAN_POINT('Ctrl Pts',(6.07136375028342,-2.7889852078473,23.5192645158137));
#6252=CARTESIAN_POINT('Ctrl Pts',(6.10171875193144,-2.7712280563091,23.5171206939419));
#6253=CARTESIAN_POINT('Ctrl Pts',(6.11959391940449,-2.76053748822712,23.515857348859));
#6254=CARTESIAN_POINT('Ctrl Pts',(6.15771824562205,-2.73723181605482,23.5131601402178));
#6255=CARTESIAN_POINT('Ctrl Pts',(6.17793357841946,-2.72456359174508,23.5117282719134));
#6256=CARTESIAN_POINT('Ctrl Pts',(6.23441605057961,-2.6882884224586,23.5077210341611));
#6257=CARTESIAN_POINT('Ctrl Pts',(6.27035179322774,-2.66417338513943,23.5051638787774));
#6258=CARTESIAN_POINT('Ctrl Pts',(6.38973711359475,-2.58052294992327,23.4966269297175));
#6259=CARTESIAN_POINT('Ctrl Pts',(6.47083234999511,-2.51773051373397,23.4907599178561));
#6260=CARTESIAN_POINT('Ctrl Pts',(6.71728400119812,-2.30735854710629,23.4724404557752));
#6261=CARTESIAN_POINT('Ctrl Pts',(6.87047701246788,-2.14656494184902,23.4603327240357));
#6262=CARTESIAN_POINT('Ctrl Pts',(7.05503687824137,-1.90787831382013,23.4429224639934));
#6263=CARTESIAN_POINT('Ctrl Pts',(7.10172092246189,-1.84260541163386,23.438206228264));
#6264=CARTESIAN_POINT('Ctrl Pts',(7.15513887606974,-1.76169780647075,23.4323248179688));
#6265=CARTESIAN_POINT('Ctrl Pts',(7.16425139941566,-1.74765920967625,23.431303055027));
#6266=CARTESIAN_POINT('Ctrl Pts',(7.17824594712378,-1.72572724269762,23.4297038027168));
#6267=CARTESIAN_POINT('Ctrl Pts',(7.18320406840346,-1.71788245489541,23.4291311816741));
#6268=CARTESIAN_POINT('Ctrl Pts',(7.1922818181667,-1.70338123943199,23.4280713883739));
#6269=CARTESIAN_POINT('Ctrl Pts',(7.19641114036327,-1.69673111810703,23.4275848616532));
#6270=CARTESIAN_POINT('Ctrl Pts',(7.205732450304,-1.68159673090469,23.4264764708278));
#6271=CARTESIAN_POINT('Ctrl Pts',(7.21090938459066,-1.67310347773368,23.4258536574622));
#6272=CARTESIAN_POINT('Ctrl Pts',(7.2266227802468,-1.64705356325947,23.4239413060423));
#6273=CARTESIAN_POINT('Ctrl Pts',(7.23703107698062,-1.62942072360718,23.4226439583952));
#6274=CARTESIAN_POINT('Ctrl Pts',(7.33364807272611,-1.46211885016639,23.4103160654394));
#6275=CARTESIAN_POINT('Ctrl Pts',(7.40785270425699,-1.30586080326885,23.3986775301669));
#6276=CARTESIAN_POINT('Ctrl Pts',(7.54876386434284,-0.934913234746212,23.3718389061261));
#6277=CARTESIAN_POINT('Ctrl Pts',(7.60629135096761,-0.717633121003952,23.3567147696628));
#6278=CARTESIAN_POINT('Ctrl Pts',(7.65075569699311,-0.432238794097489,23.3381223317963));
#6279=CARTESIAN_POINT('Ctrl Pts',(7.65878419504358,-0.368070962752275,23.3340176750285));
#6280=CARTESIAN_POINT('Ctrl Pts',(7.66703629601794,-0.280892798517734,23.3285399692109));
#6281=CARTESIAN_POINT('Ctrl Pts',(7.66895205378973,-0.258061619725829,23.327114492367));
#6282=CARTESIAN_POINT('Ctrl Pts',(7.67171370172156,-0.220323813622921,23.3247728533729));
#6283=CARTESIAN_POINT('Ctrl Pts',(7.67269974243683,-0.205428572424087,23.323852333077));
#6284=CARTESIAN_POINT('Ctrl Pts',(7.67436883559197,-0.177245339782721,23.3221174958161));
#6285=CARTESIAN_POINT('Ctrl Pts',(7.67507315834198,-0.163958966835426,23.3213025309651));
#6286=CARTESIAN_POINT('Ctrl Pts',(7.67634338032585,-0.136819033873957,23.3196435440727));
#6287=CARTESIAN_POINT('Ctrl Pts',(7.67690219918881,-0.122965410292963,23.3187997592406));
#6288=CARTESIAN_POINT('Ctrl Pts',(7.6779647492397,-0.0915987252782205,23.3168959750869));
#6289=CARTESIAN_POINT('Ctrl Pts',(7.67841511027732,-0.0740842076861186,
23.315837646492));
#6290=CARTESIAN_POINT('Ctrl Pts',(7.67905843342729,-0.0374380329825862,
23.3136326381325));
#6291=CARTESIAN_POINT('Ctrl Pts',(7.67922390057638,-0.0183066048955584,
23.3124868338538));
#6292=CARTESIAN_POINT('Ctrl Pts',(7.6792190005175,0.000825405381727912,
23.3113459957337));
#6293=CARTESIAN_POINT('Origin',(4.45646910621825,-5.13094777615093E-16,
-2.31077344927308));
#6294=CARTESIAN_POINT('',(7.67921910621823,-2.19646041259736E-11,22.0659612921829));
#6295=CARTESIAN_POINT('',(7.67921900305864,0.000815423282546346,22.3107734492731));
#6296=CARTESIAN_POINT('',(7.67921910621823,-3.51191647465084E-13,-2.31077344927308));
#6297=CARTESIAN_POINT('Ctrl Pts',(7.67921900305864,0.000815423282546346,
22.3107734492731));
#6298=CARTESIAN_POINT('Ctrl Pts',(7.67924509448734,-0.102304209114605,22.3171055672954));
#6299=CARTESIAN_POINT('Ctrl Pts',(7.67431750357225,-0.205370600635493,22.3234376853178));
#6300=CARTESIAN_POINT('Ctrl Pts',(7.66447767354317,-0.30789380388341,22.3297698033401));
#6301=CARTESIAN_POINT('Ctrl Pts',(7.65462973255273,-0.410501516898032,22.3361071409206));
#6302=CARTESIAN_POINT('Ctrl Pts',(7.63986152481682,-0.512564754953075,22.342444478501));
#6303=CARTESIAN_POINT('Ctrl Pts',(7.62026604465574,-0.613601250677855,22.3487818160815));
#6304=CARTESIAN_POINT('Ctrl Pts',(7.60063379821649,-0.714827317460683,22.3551310441751));
#6305=CARTESIAN_POINT('Ctrl Pts',(7.57615626072823,-0.815022402810588,22.3614802722688));
#6306=CARTESIAN_POINT('Ctrl Pts',(7.54697718013528,-0.913716262060345,22.3678295003625));
#6307=CARTESIAN_POINT('Ctrl Pts',(7.51776904979301,-1.01250837772573,22.3741850495424));
#6308=CARTESIAN_POINT('Ctrl Pts',(7.48385017622183,-1.10979591354012,22.3805405987224));
#6309=CARTESIAN_POINT('Ctrl Pts',(7.44541291204491,-1.20512758167354,22.3868961479023));
#6310=CARTESIAN_POINT('Ctrl Pts',(7.40689339787825,-1.30066324530179,22.3932652970057));
#6311=CARTESIAN_POINT('Ctrl Pts',(7.36383633604013,-1.39423431600571,22.3996344461092));
#6312=CARTESIAN_POINT('Ctrl Pts',(7.31648092742837,-1.48541238214788,22.4060035952127));
#6313=CARTESIAN_POINT('Ctrl Pts',(7.28355106781503,-1.54881550770199,22.4104325546913));
#6314=CARTESIAN_POINT('Ctrl Pts',(7.24854370443691,-1.61106203584785,22.4148615141699));
#6315=CARTESIAN_POINT('Ctrl Pts',(7.21155137183393,-1.67201652868321,22.4192904736485));
#6316=CARTESIAN_POINT('Ctrl Pts',(7.15998739255039,-1.7569816007573,22.4254640441895));
#6317=CARTESIAN_POINT('Ctrl Pts',(7.10439904072553,-1.83970790273964,22.4316376147305));
#6318=CARTESIAN_POINT('Ctrl Pts',(7.0450064794378,-1.9197895275122,22.4378111852716));
#6319=CARTESIAN_POINT('Ctrl Pts',(6.98569408981377,-1.99976305327453,22.4439764223545));
#6320=CARTESIAN_POINT('Ctrl Pts',(6.92258795393058,-2.07709865192323,22.4501416594374));
#6321=CARTESIAN_POINT('Ctrl Pts',(6.85595299413103,-2.15141688989996,22.4563068965204));
#6322=CARTESIAN_POINT('Ctrl Pts',(6.78938831987777,-2.22565673812496,22.4624656306046));
#6323=CARTESIAN_POINT('Ctrl Pts',(6.71930251005466,-2.29688523173755,22.4686243646889));
#6324=CARTESIAN_POINT('Ctrl Pts',(6.64600187892413,-2.36475449037458,22.4747830987731));
#6325=CARTESIAN_POINT('Ctrl Pts',(6.57275448031797,-2.43257446086895,22.4809373602497));
#6326=CARTESIAN_POINT('Ctrl Pts',(6.49629721980748,-2.49703975260539,22.4870916217263));
#6327=CARTESIAN_POINT('Ctrl Pts',(6.41697388958871,-2.55783864950106,22.4932458832029));
#6328=CARTESIAN_POINT('Ctrl Pts',(6.33768038094169,-2.61861468907769,22.4993978309876));
#6329=CARTESIAN_POINT('Ctrl Pts',(6.2555232878144,-2.67572680888366,22.5055497787722));
#6330=CARTESIAN_POINT('Ctrl Pts',(6.17087947714751,-2.72890356050742,22.5117017265569));
#6331=CARTESIAN_POINT('Ctrl Pts',(6.08624487519753,-2.78207452683337,22.5178530050481));
#6332=CARTESIAN_POINT('Ctrl Pts',(5.99912446122754,-2.83131074527077,22.5240042835394));
#6333=CARTESIAN_POINT('Ctrl Pts',(5.90992322417004,-2.87638465604113,22.5301555620306));
#6334=CARTESIAN_POINT('Ctrl Pts',(5.8207078612431,-2.92146570469656,22.5363078146357));
#6335=CARTESIAN_POINT('Ctrl Pts',(5.72941140823683,-2.96238294062894,22.5424600672407));
#6336=CARTESIAN_POINT('Ctrl Pts',(5.63646162197437,-2.99895568911236,22.5486123198458));
#6337=CARTESIAN_POINT('Ctrl Pts',(5.54341270018547,-3.03556744423388,22.5547711341313));
#6338=CARTESIAN_POINT('Ctrl Pts',(5.44870732873436,-3.06782529997915,22.5609299484169));
#6339=CARTESIAN_POINT('Ctrl Pts',(5.35279121626834,-3.09559755742493,22.5670887627024));
#6340=CARTESIAN_POINT('Ctrl Pts',(5.25682142366214,-3.12338535781376,22.5732510238126));
#6341=CARTESIAN_POINT('Ctrl Pts',(5.15963996278668,-3.14668245924176,22.5794132849227));
#6342=CARTESIAN_POINT('Ctrl Pts',(5.06170356259582,-3.16540815935531,22.5855755460329));
#6343=CARTESIAN_POINT('Ctrl Pts',(4.96360463068712,-3.18416493596547,22.5917480338093));
#6344=CARTESIAN_POINT('Ctrl Pts',(4.86474868687652,-3.19833509620449,22.5979205215858));
#6345=CARTESIAN_POINT('Ctrl Pts',(4.7655985483105,-3.20788973478385,22.6040930093622));
#6346=CARTESIAN_POINT('Ctrl Pts',(4.69217037397495,-3.21496566707668,22.6086642032616));
#6347=CARTESIAN_POINT('Ctrl Pts',(4.61858095894887,-3.21951129524688,22.6132353971609));
#6348=CARTESIAN_POINT('Ctrl Pts',(4.54501750299387,-3.22153329083036,22.6178065910603));
#6349=CARTESIAN_POINT('Ctrl Pts',(4.44566662018497,-3.22426409029657,22.6239802019041));
#6350=CARTESIAN_POINT('Ctrl Pts',(4.3460153608817,-3.22239945011425,22.6301538127479));
#6351=CARTESIAN_POINT('Ctrl Pts',(4.24652417069623,-3.21590433417235,22.6363274235917));
#6352=CARTESIAN_POINT('Ctrl Pts',(4.14716727029211,-3.20941798511421,22.6424927015082));
#6353=CARTESIAN_POINT('Ctrl Pts',(4.04797043900825,-3.19831361120412,22.6486579794248));
#6354=CARTESIAN_POINT('Ctrl Pts',(3.94939614020412,-3.18260813950406,22.6548232573413));
#6355=CARTESIAN_POINT('Ctrl Pts',(3.85092580785642,-3.16691923238786,22.6609820327302));
#6356=CARTESIAN_POINT('Ctrl Pts',(3.7530771290095,-3.1466389433667,22.6671408081192));
#6357=CARTESIAN_POINT('Ctrl Pts',(3.65630849093359,-3.12183608670396,22.6732995835082));
#6358=CARTESIAN_POINT('Ctrl Pts',(3.55961011952949,-3.09705124015508,22.6794538868217));
#6359=CARTESIAN_POINT('Ctrl Pts',(3.46399064894999,-3.06775046261778,22.6856081901352));
#6360=CARTESIAN_POINT('Ctrl Pts',(3.36989839396145,-3.03405366626327,22.6917624934487));
#6361=CARTESIAN_POINT('Ctrl Pts',(3.27584150789532,-3.00036953640693,22.6979144833829));
#6362=CARTESIAN_POINT('Ctrl Pts',(3.18331110499084,-2.96229281742073,22.7040664733171));
#6363=CARTESIAN_POINT('Ctrl Pts',(3.09273959245567,-2.91999304379184,22.7102184632513));
#6364=CARTESIAN_POINT('Ctrl Pts',(3.00217792962281,-2.87769787028683,22.7163697841532));
#6365=CARTESIAN_POINT('Ctrl Pts',(2.91357512696444,-2.83118073896755,22.7225211050551));
#6366=CARTESIAN_POINT('Ctrl Pts',(2.82734195657743,-2.78065860774081,22.728672425957));
#6367=CARTESIAN_POINT('Ctrl Pts',(2.74109512749669,-2.7301284741837,22.7348247211824));
#6368=CARTESIAN_POINT('Ctrl Pts',(2.65721905082264,-2.67559230018017,22.7409770164078));
#6369=CARTESIAN_POINT('Ctrl Pts',(2.57609744321833,-2.61731159235708,22.7471293116333));
#6370=CARTESIAN_POINT('Ctrl Pts',(2.49488931526314,-2.55896872517301,22.7532881685968));
#6371=CARTESIAN_POINT('Ctrl Pts',(2.4164418759712,-2.49687360303757,22.7594470255603));
#6372=CARTESIAN_POINT('Ctrl Pts',(2.34110741893956,-2.43132936775199,22.7656058825238));
#6373=CARTESIAN_POINT('Ctrl Pts',(2.26573079953395,-2.36574844937785,22.7717681864097));
#6374=CARTESIAN_POINT('Ctrl Pts',(2.19347094596956,-2.29671487343409,22.7779304902957));
#6375=CARTESIAN_POINT('Ctrl Pts',(2.12464327316731,-2.22456868781707,22.7840927941816));
#6376=CARTESIAN_POINT('Ctrl Pts',(2.05570138043574,-2.15230277517912,22.7902653244472));
#6377=CARTESIAN_POINT('Ctrl Pts',(1.99020333001169,-2.07691426329369,22.7964378547128));
#6378=CARTESIAN_POINT('Ctrl Pts',(1.92842431175713,-1.99877639562255,22.8026103849785));
#6379=CARTESIAN_POINT('Ctrl Pts',(1.88267679024094,-1.94091510414353,22.8071811594763));
#6380=CARTESIAN_POINT('Ctrl Pts',(1.83896772291095,-1.88154690348,22.811751933974));
#6381=CARTESIAN_POINT('Ctrl Pts',(1.79739295992886,-1.82083266961427,22.8163227084718));
#6382=CARTESIAN_POINT('Ctrl Pts',(1.74124124457877,-1.73883079796932,22.8224960889103));
#6383=CARTESIAN_POINT('Ctrl Pts',(1.68878795284854,-1.65408541782211,22.8286694693488));
#6384=CARTESIAN_POINT('Ctrl Pts',(1.64031213618421,-1.56696441651639,22.8348428497873));
#6385=CARTESIAN_POINT('Ctrl Pts',(1.59190175740682,-1.47996102053691,22.8410078967309));
#6386=CARTESIAN_POINT('Ctrl Pts',(1.54745839088643,-1.39058875358549,22.8471729436745));
#6387=CARTESIAN_POINT('Ctrl Pts',(1.50721851831545,-1.2992453703034,22.8533379906181));
#6388=CARTESIAN_POINT('Ctrl Pts',(1.46702109012038,-1.20799833456543,22.8594965347685));
#6389=CARTESIAN_POINT('Ctrl Pts',(1.43101851506279,-1.11478471117023,22.8656550789189));
#6390=CARTESIAN_POINT('Ctrl Pts',(1.39940146491032,-1.02002695992205,22.8718136230692));
#6391=CARTESIAN_POINT('Ctrl Pts',(1.36780737095772,-0.925338009459091,22.8779676956839));
#6392=CARTESIAN_POINT('Ctrl Pts',(1.34059260812932,-0.829107570824273,22.8841217682985));
#6393=CARTESIAN_POINT('Ctrl Pts',(1.31789945043922,-0.731777342039871,22.8902758409131));
#6394=CARTESIAN_POINT('Ctrl Pts',(1.29521482185299,-0.634483694309692,22.8964276005519));
#6395=CARTESIAN_POINT('Ctrl Pts',(1.27704852007994,-0.536091500147451,22.9025793601908));
#6396=CARTESIAN_POINT('Ctrl Pts',(1.26349249774668,-0.437055992126014,22.9087311198296));
#6397=CARTESIAN_POINT('Ctrl Pts',(1.24993794821603,-0.338031243879885,22.9148822111066));
#6398=CARTESIAN_POINT('Ctrl Pts',(1.24099274112815,-0.238363750908735,22.9210333023836));
#6399=CARTESIAN_POINT('Ctrl Pts',(1.23669725031307,-0.138516274931135,22.9271843936606));
#6400=CARTESIAN_POINT('Ctrl Pts',(1.23240107844362,-0.038652968036155,22.9333364601993));
#6401=CARTESIAN_POINT('Ctrl Pts',(1.23275610582834,0.0613899447312124,22.939488526738));
#6402=CARTESIAN_POINT('Ctrl Pts',(1.23775060464388,0.161148286130284,22.9456405932767));
#6403=CARTESIAN_POINT('Ctrl Pts',(1.24275043286246,0.261013075128447,22.9517992244064));
#6404=CARTESIAN_POINT('Ctrl Pts',(1.25239959633902,0.360592251938886,22.9579578555361));
#6405=CARTESIAN_POINT('Ctrl Pts',(1.2666343461172,0.459425473554663,22.9641164866659));
#6406=CARTESIAN_POINT('Ctrl Pts',(1.28087706579548,0.558314030944969,22.9702785659542));
#6407=CARTESIAN_POINT('Ctrl Pts',(1.29971040295971,0.656455374992856,22.9764406452425));
#6408=CARTESIAN_POINT('Ctrl Pts',(1.32301960403999,0.753400145871158,22.9826027245308));
#6409=CARTESIAN_POINT('Ctrl Pts',(1.34636750468061,0.850505871215389,22.9887750345327));
#6410=CARTESIAN_POINT('Ctrl Pts',(1.37420599120284,0.946410638148802,22.9949473445346));
#6411=CARTESIAN_POINT('Ctrl Pts',(1.40637060934822,1.04068089340155,23.0011196545365));
#6412=CARTESIAN_POINT('Ctrl Pts',(1.43020133655365,1.11052561303604,23.0056927116521));
#6413=CARTESIAN_POINT('Ctrl Pts',(1.45640577378608,1.1794734459682,23.0102657687678));
#6414=CARTESIAN_POINT('Ctrl Pts',(1.48490056087795,1.24735638165042,23.0148388258834));
#6415=CARTESIAN_POINT('Ctrl Pts',(1.52336904858866,1.33899959585093,23.0210125372674));
#6416=CARTESIAN_POINT('Ctrl Pts',(1.56614826883377,1.42902202661247,23.0271862486514));
#6417=CARTESIAN_POINT('Ctrl Pts',(1.61308032646999,1.51698971970861,23.0333599600354));
#6418=CARTESIAN_POINT('Ctrl Pts',(1.65994902767183,1.60483865987432,23.0395253371516));
#6419=CARTESIAN_POINT('Ctrl Pts',(1.71095922063842,1.6906379960412,23.0456907142677));
#6420=CARTESIAN_POINT('Ctrl Pts',(1.76590483597035,1.77397335666725,23.0518560913838));
#6421=CARTESIAN_POINT('Ctrl Pts',(1.82079248811693,1.85722080522016,23.0580149645252));
#6422=CARTESIAN_POINT('Ctrl Pts',(1.87960707114858,1.93800908549988,23.0641738376665));
#6423=CARTESIAN_POINT('Ctrl Pts',(1.94209692262656,2.01594892913493,23.0703327108079));
#6424=CARTESIAN_POINT('Ctrl Pts',(2.00454137323384,2.09383214698707,23.0764871093314));
#6425=CARTESIAN_POINT('Ctrl Pts',(2.07065551264351,2.16887070503612,23.0826415078549));
#6426=CARTESIAN_POINT('Ctrl Pts',(2.14014527643311,2.24070557594464,23.0887959063784));
#6427=CARTESIAN_POINT('Ctrl Pts',(2.20960890176716,2.31251342628959,23.0949479899355));
#6428=CARTESIAN_POINT('Ctrl Pts',(2.28244532695656,2.38111967231176,23.1011000734926));
#6429=CARTESIAN_POINT('Ctrl Pts',(2.35832183509285,2.44620023529738,23.1072521570496));
#6430=CARTESIAN_POINT('Ctrl Pts',(2.43419007094787,2.51127370300758,23.1134035698884));
#6431=CARTESIAN_POINT('Ctrl Pts',(2.51309740124686,2.57282196928315,23.1195549827271));
#6432=CARTESIAN_POINT('Ctrl Pts',(2.59467682086061,2.63056021574924,23.1257063955658));
#6433=CARTESIAN_POINT('Ctrl Pts',(2.67626913816593,2.68830759062171,23.1318587809418));
#6434=CARTESIAN_POINT('Ctrl Pts',(2.7605340295148,2.74224349840427,23.1380111663178));
#6435=CARTESIAN_POINT('Ctrl Pts',(2.84707505486027,2.79212613432012,23.1441635516938));
#6436=CARTESIAN_POINT('Ctrl Pts',(2.93370833294037,2.84206194512679,23.1503224955127));
#6437=CARTESIAN_POINT('Ctrl Pts',(3.02262221327157,2.88793563884925,23.1564814393316));
#6438=CARTESIAN_POINT('Ctrl Pts',(3.11339527590472,2.92955120262931,23.1626403831505));
#6439=CARTESIAN_POINT('Ctrl Pts',(3.20421911570178,2.97119004556558,23.1688027721953));
#6440=CARTESIAN_POINT('Ctrl Pts',(3.29690380634158,3.00856585256235,23.17496516124));
#6441=CARTESIAN_POINT('Ctrl Pts',(3.39100950494955,3.04153142357008,23.1811275502848));
#6442=CARTESIAN_POINT('Ctrl Pts',(3.48527131496083,3.07455168097436,23.1873001620813));
#6443=CARTESIAN_POINT('Ctrl Pts',(3.58095842534341,3.10314696473573,23.1934727738779));
#6444=CARTESIAN_POINT('Ctrl Pts',(3.67761733052942,3.12722040700784,23.1996453856745));
#6445=CARTESIAN_POINT('Ctrl Pts',(3.74917811516308,3.14504302163926,23.2042152382147));
#6446=CARTESIAN_POINT('Ctrl Pts',(3.82127127827554,3.16038823792912,23.2087850907549));
#6447=CARTESIAN_POINT('Ctrl Pts',(3.89371085221291,3.17323505433316,23.2133549432952));
#6448=CARTESIAN_POINT('Ctrl Pts',(3.99157672170618,3.19059110420017,23.219528814399));
#6449=CARTESIAN_POINT('Ctrl Pts',(4.09041747329918,3.20344585013164,23.2257026855029));
#6450=CARTESIAN_POINT('Ctrl Pts',(4.18978282391545,3.21169674616571,23.2318765566067));
#6451=CARTESIAN_POINT('Ctrl Pts',(4.28901409821647,3.21993650904591,23.2380420971418));
#6452=CARTESIAN_POINT('Ctrl Pts',(4.38876813573049,3.22358473387207,23.2442076376768));
#6453=CARTESIAN_POINT('Ctrl Pts',(4.48858499707313,3.22258997268571,23.2503731782119));
#6454=CARTESIAN_POINT('Ctrl Pts',(4.58829661811924,3.22159626030976,23.2565322182088));
#6455=CARTESIAN_POINT('Ctrl Pts',(4.68807049959196,3.21596929863723,23.2626912582057));
#6456=CARTESIAN_POINT('Ctrl Pts',(4.78744308369429,3.20570956088252,23.2688502982026));
#6457=CARTESIAN_POINT('Ctrl Pts',(4.88674354379862,3.19545726958109,23.2750048680069));
#6458=CARTESIAN_POINT('Ctrl Pts',(4.98564285509247,3.18057893184648,23.2811594378113));
#6459=CARTESIAN_POINT('Ctrl Pts',(5.08367988799598,3.16112704548895,23.2873140076156));
#6460=CARTESIAN_POINT('Ctrl Pts',(5.1816800877601,3.14168246732935,23.2934662651087));
#6461=CARTESIAN_POINT('Ctrl Pts',(5.27881822752662,3.11766783929687,23.2996185226019));
#6462=CARTESIAN_POINT('Ctrl Pts',(5.37464159431828,3.0891870847516,23.305770780095));
#6463=CARTESIAN_POINT('Ctrl Pts',(5.47045455235275,3.06070942391165,23.3119223693028));
#6464=CARTESIAN_POINT('Ctrl Pts',(5.56495260525435,3.02776672479357,23.3180739585106));
#6465=CARTESIAN_POINT('Ctrl Pts',(5.65769744527187,2.99051300615035,23.3242255477183));
#6466=CARTESIAN_POINT('Ctrl Pts',(5.75045698116954,2.95325338447053,23.330378111676));
#6467=CARTESIAN_POINT('Ctrl Pts',(5.84146234952923,2.91168154824708,23.3365306756336));
#6468=CARTESIAN_POINT('Ctrl Pts',(5.9302954322741,2.86599956788633,23.3426832395912));
#6469=CARTESIAN_POINT('Ctrl Pts',(6.01922324132289,2.82026887498492,23.3488423642762));
#6470=CARTESIAN_POINT('Ctrl Pts',(6.10597375245543,2.77041948499216,23.3550014889613));
#6471=CARTESIAN_POINT('Ctrl Pts',(6.190153786505,2.71669928255575,23.3611606136463));
#6472=CARTESIAN_POINT('Ctrl Pts',(6.2743809294481,2.66294901717952,23.3673231851053));
#6473=CARTESIAN_POINT('Ctrl Pts',(6.3560343758737,2.60532387568752,23.3734857565644));
#6474=CARTESIAN_POINT('Ctrl Pts',(6.4347519782709,2.54411368469316,23.3796483280234));
#6475=CARTESIAN_POINT('Ctrl Pts',(6.51360016871647,2.48280194945534,23.3858211228397));
#6476=CARTESIAN_POINT('Ctrl Pts',(6.58950245689766,2.41789356754295,23.3919939176561));
#6477=CARTESIAN_POINT('Ctrl Pts',(6.66213158399558,2.34971713119368,23.3981667124725));
#6478=CARTESIAN_POINT('Ctrl Pts',(6.71588005500475,2.29926383016906,23.4027348285505));
#6479=CARTESIAN_POINT('Ctrl Pts',(6.76783669360609,2.2470215505427,23.4073029446286));
#6480=CARTESIAN_POINT('Ctrl Pts',(6.8178831761066,2.19313500565588,23.4118710607067));
#6481=CARTESIAN_POINT('Ctrl Pts',(6.88585467551961,2.11994805881889,23.418075326897));
#6482=CARTESIAN_POINT('Ctrl Pts',(6.95055587273519,2.04345216793193,23.4242795930872));
#6483=CARTESIAN_POINT('Ctrl Pts',(7.0116429694277,1.96397660150807,23.4304838592775));
#6484=CARTESIAN_POINT('Ctrl Pts',(7.07162307533018,1.88594125281966,23.4365756947598));
#6485=CARTESIAN_POINT('Ctrl Pts',(7.12811864870048,1.80503365970823,23.442667530242));
#6486=CARTESIAN_POINT('Ctrl Pts',(7.18084054520929,1.72160327163658,23.4487593657243));
#6487=CARTESIAN_POINT('Ctrl Pts',(7.23351252721221,1.63825187136455,23.4548454337555));
#6488=CARTESIAN_POINT('Ctrl Pts',(7.28241769076799,1.55238279315417,23.4609315017867));
#6489=CARTESIAN_POINT('Ctrl Pts',(7.32730826166912,1.46437703684197,23.4670175698179));
#6490=CARTESIAN_POINT('Ctrl Pts',(7.37216900598024,1.37642975409245,23.4730995940899));
#6491=CARTESIAN_POINT('Ctrl Pts',(7.41302025501747,1.28634900893363,23.479181618362));
#6492=CARTESIAN_POINT('Ctrl Pts',(7.44965914240116,1.19454215906984,23.4852636426341));
#6493=CARTESIAN_POINT('Ctrl Pts',(7.48756586525713,1.09955846653514,23.4915561265206));
#6494=CARTESIAN_POINT('Ctrl Pts',(7.52096314848273,1.00272746696704,23.4978486104072));
#6495=CARTESIAN_POINT('Ctrl Pts',(7.54967999396536,0.904524165748279,23.5041410942938));
#6496=CARTESIAN_POINT('Ctrl Pts',(7.57743051006099,0.809625431388222,23.5102218344462));
#6497=CARTESIAN_POINT('Ctrl Pts',(7.60081044546113,0.713445735394949,23.5163025745986));
#6498=CARTESIAN_POINT('Ctrl Pts',(7.61971633945065,0.616428831210426,23.522383314751));
#6499=CARTESIAN_POINT('Ctrl Pts',(7.63960974593652,0.514344438268555,23.5287816705047));
#6500=CARTESIAN_POINT('Ctrl Pts',(7.65454893198461,0.411333539278742,23.5351800262584));
#6501=CARTESIAN_POINT('Ctrl Pts',(7.66447488326935,0.307922874932377,23.5415783820121));
#6502=CARTESIAN_POINT('Ctrl Pts',(7.6744008345541,0.204512210586012,23.5479767377657));
#6503=CARTESIAN_POINT('Ctrl Pts',(7.67931354939866,0.100702353844344,23.5543750935194));
#6504=CARTESIAN_POINT('Ctrl Pts',(7.67921772993578,-0.0029783932951826,
23.5607734492731));
#6505=CARTESIAN_POINT('Ctrl Pts',(7.67921900114641,0.000822946196721505,
23.3113461423745));
#6506=CARTESIAN_POINT('Ctrl Pts',(7.67916246529529,0.222223699938065,23.2981440527433));
#6507=CARTESIAN_POINT('Ctrl Pts',(7.65629256834702,0.443047830936302,23.2857023480931));
#6508=CARTESIAN_POINT('Ctrl Pts',(7.56973435070216,0.856870180313654,23.2620612092812));
#6509=CARTESIAN_POINT('Ctrl Pts',(7.51014820977475,1.04960502293162,23.2508847166683));
#6510=CARTESIAN_POINT('Ctrl Pts',(7.42065187039683,1.26521681989633,23.2369515898085));
#6511=CARTESIAN_POINT('Ctrl Pts',(7.40787152411228,1.29474964723432,23.2350099785529));
#6512=CARTESIAN_POINT('Ctrl Pts',(7.38975659501365,1.33494719853519,23.2323149582033));
#6513=CARTESIAN_POINT('Ctrl Pts',(7.38480139824918,1.34578211160455,23.2315832728468));
#6514=CARTESIAN_POINT('Ctrl Pts',(7.37636598006021,1.36395961519248,23.2303464529262));
#6515=CARTESIAN_POINT('Ctrl Pts',(7.37291780070969,1.37131710265611,23.2298432649276));
#6516=CARTESIAN_POINT('Ctrl Pts',(7.36629171590265,1.38531735264428,23.2288807082625));
#6517=CARTESIAN_POINT('Ctrl Pts',(7.36311880703881,1.39196239227626,23.2284216648887));
#6518=CARTESIAN_POINT('Ctrl Pts',(7.35550714160626,1.40776403510104,23.2273249854188));
#6519=CARTESIAN_POINT('Ctrl Pts',(7.35104776737681,1.41691053951358,23.226686102204));
#6520=CARTESIAN_POINT('Ctrl Pts',(7.33504414149721,1.44934429928481,23.2244064429076));
#6521=CARTESIAN_POINT('Ctrl Pts',(7.32326191936954,1.47251213873461,23.2227520004627));
#6522=CARTESIAN_POINT('Ctrl Pts',(7.21625161867555,1.67677745649977,23.2079492287376));
#6523=CARTESIAN_POINT('Ctrl Pts',(7.1042656669358,1.84855137085491,23.1940144442717));
#6524=CARTESIAN_POINT('Ctrl Pts',(6.84944412765601,2.16829965786655,23.1663806787226));
#6525=CARTESIAN_POINT('Ctrl Pts',(6.70720139641688,2.31561678349322,23.1527506660772));
#6526=CARTESIAN_POINT('Ctrl Pts',(6.52617955210191,2.47053968967476,23.1375502485921));
#6527=CARTESIAN_POINT('Ctrl Pts',(6.50006651533279,2.49218327119314,23.1354027475394));
#6528=CARTESIAN_POINT('Ctrl Pts',(6.45788118324589,2.52603925273079,23.1320039921066));
#6529=CARTESIAN_POINT('Ctrl Pts',(6.44202796275637,2.53851938447907,23.1307421789972));
#6530=CARTESIAN_POINT('Ctrl Pts',(6.41213395282259,2.56160146204964,23.1283912000536));
#6531=CARTESIAN_POINT('Ctrl Pts',(6.39812159526092,2.57223884468067,23.1273006599017));
#6532=CARTESIAN_POINT('Ctrl Pts',(6.37310663745903,2.59090788421063,23.1253737575749));
#6533=CARTESIAN_POINT('Ctrl Pts',(6.36213899432119,2.59898545152881,23.1245356140653));
#6534=CARTESIAN_POINT('Ctrl Pts',(6.33902427182084,2.6157842429427,23.1227830128144));
#6535=CARTESIAN_POINT('Ctrl Pts',(6.32686701665878,2.62449096504731,23.1218691285983));
#6536=CARTESIAN_POINT('Ctrl Pts',(6.29584075066423,2.64638611351152,23.119556496642));
#6537=CARTESIAN_POINT('Ctrl Pts',(6.27689002144462,2.65945769692104,23.1181622222351));
#6538=CARTESIAN_POINT('Ctrl Pts',(6.20367748751797,2.70880798764787,23.1128433709734));
#6539=CARTESIAN_POINT('Ctrl Pts',(6.14845619360334,2.74363962773884,23.1089727646797));
#6540=CARTESIAN_POINT('Ctrl Pts',(5.80390107549137,2.94661042703668,23.0855775644362));
#6541=CARTESIAN_POINT('Ctrl Pts',(5.49094578375706,3.07048929650484,23.0677513007489));
#6542=CARTESIAN_POINT('Ctrl Pts',(5.11892347952693,3.15427652898885,23.0456058484345));
#6543=CARTESIAN_POINT('Ctrl Pts',(5.07306742663107,3.16356006691765,23.042856109245));
#6544=CARTESIAN_POINT('Ctrl Pts',(4.99658974934862,3.17731706225886,23.0382129738546));
#6545=CARTESIAN_POINT('Ctrl Pts',(4.96607561566509,3.18235369947264,23.0363453939734));
#6546=CARTESIAN_POINT('Ctrl Pts',(4.92389204476934,3.18869425154179,23.0337371159028));
#6547=CARTESIAN_POINT('Ctrl Pts',(4.91227983416712,3.19037486883599,23.0330163559347));
#6548=CARTESIAN_POINT('Ctrl Pts',(4.89264555899072,3.19310712659352,23.0317926244979));
#6549=CARTESIAN_POINT('Ctrl Pts',(4.88462809798105,3.19419205681853,23.0312915051388));
#6550=CARTESIAN_POINT('Ctrl Pts',(4.86926857321914,3.19621165465521,23.0303286219528));
#6551=CARTESIAN_POINT('Ctrl Pts',(4.8619272506051,3.1971512369369,23.0298671563545));
#6552=CARTESIAN_POINT('Ctrl Pts',(4.84434195363117,3.19934035667021,23.0287589053283));
#6553=CARTESIAN_POINT('Ctrl Pts',(4.83409516099281,3.20056598424895,23.0281108136766));
#6554=CARTESIAN_POINT('Ctrl Pts',(4.79708590720555,3.20481249306297,23.0257620902968));
#6555=CARTESIAN_POINT('Ctrl Pts',(4.77029255667467,3.20754698371423,23.0240467068354));
#6556=CARTESIAN_POINT('Ctrl Pts',(4.57492799132225,3.22501445717925,23.0114450221691));
#6557=CARTESIAN_POINT('Ctrl Pts',(4.40547737372048,3.22678474942344,23.0000203398798));
#6558=CARTESIAN_POINT('Ctrl Pts',(4.08761659544302,3.20505725316384,22.9784672388896));
#6559=CARTESIAN_POINT('Ctrl Pts',(3.93942260627164,3.18451140987843,22.9683678690529));
#6560=CARTESIAN_POINT('Ctrl Pts',(3.67212488762544,3.12829420709448,22.9503392742126));
#6561=CARTESIAN_POINT('Ctrl Pts',(3.55262357440905,3.09588277850723,22.9423481048125));
#6562=CARTESIAN_POINT('Ctrl Pts',(3.40933195748334,3.04801068754464,22.9328596047883));
#6563=CARTESIAN_POINT('Ctrl Pts',(3.38350598342889,3.03901555949292,22.9311529781266));
#6564=CARTESIAN_POINT('Ctrl Pts',(3.34285383660536,3.02427367406246,22.9284715366918));
#6565=CARTESIAN_POINT('Ctrl Pts',(3.32795078624666,3.01874421577839,22.927489575792));
#6566=CARTESIAN_POINT('Ctrl Pts',(3.30003463698504,3.00815090011362,22.9256519602629));
#6567=CARTESIAN_POINT('Ctrl Pts',(3.28701240673154,3.00311231178834,22.924795487485));
#6568=CARTESIAN_POINT('Ctrl Pts',(3.2578264801945,2.99160100267817,22.9228773790739));
#6569=CARTESIAN_POINT('Ctrl Pts',(3.24168158459234,2.98508157341726,22.9218173392206));
#6570=CARTESIAN_POINT('Ctrl Pts',(3.20056633126299,2.9680901122468,22.9191198806092));
#6571=CARTESIAN_POINT('Ctrl Pts',(3.17567336787464,2.95743352224281,22.9174887073598));
#6572=CARTESIAN_POINT('Ctrl Pts',(3.00370981661835,2.88123800589189,22.906228150005));
#6573=CARTESIAN_POINT('Ctrl Pts',(2.86158830545213,2.80506803040446,22.8969775356826));
#6574=CARTESIAN_POINT('Ctrl Pts',(2.544564371737,2.6032416029654,22.8757741645235));
#6575=CARTESIAN_POINT('Ctrl Pts',(2.3753852105147,2.47008592096548,22.8640149364311));
#6576=CARTESIAN_POINT('Ctrl Pts',(2.16356480032044,2.26605482825328,22.8470253923365));
#6577=CARTESIAN_POINT('Ctrl Pts',(2.10846963840207,2.20891623524886,22.8423548082257));
#6578=CARTESIAN_POINT('Ctrl Pts',(2.04477740581955,2.13778418073868,22.8365564588816));
#6579=CARTESIAN_POINT('Ctrl Pts',(2.03410160835207,2.12567959524877,22.8355702764694));
#6580=CARTESIAN_POINT('Ctrl Pts',(2.01758292311321,2.10666410148685,22.8340209218618));
#6581=CARTESIAN_POINT('Ctrl Pts',(2.011677292993,2.09980771403798,22.8334622478071));
#6582=CARTESIAN_POINT('Ctrl Pts',(2.00069801171966,2.0869517557105,22.8324144681612));
#6583=CARTESIAN_POINT('Ctrl Pts',(1.99561735569461,2.08095842255152,22.8319258851611));
#6584=CARTESIAN_POINT('Ctrl Pts',(1.98405115664124,2.06721290710908,22.8308051150995));
#6585=CARTESIAN_POINT('Ctrl Pts',(1.97758013611835,2.05944875831949,22.8301719046903));
#6586=CARTESIAN_POINT('Ctrl Pts',(1.96043308584278,2.03867724710293,22.8284777872264));
#6587=CARTESIAN_POINT('Ctrl Pts',(1.94982239095783,2.02561668380669,22.8274124868013));
#6588=CARTESIAN_POINT('Ctrl Pts',(1.85700436846548,1.90952211707044,22.8179468613321));
#6589=CARTESIAN_POINT('Ctrl Pts',(1.78109635054655,1.80162830313741,22.8091804324976));
#6590=CARTESIAN_POINT('Ctrl Pts',(1.61492480762344,1.53168104685169,22.7878403079336));
#6591=CARTESIAN_POINT('Ctrl Pts',(1.53160504612944,1.36586921518023,22.7752183498749));
#6592=CARTESIAN_POINT('Ctrl Pts',(1.42930764846595,1.10935936764252,22.756907600032));
#6593=CARTESIAN_POINT('Ctrl Pts',(1.39921343571928,1.02351102889561,22.7509635488619));
#6594=CARTESIAN_POINT('Ctrl Pts',(1.36118430691327,0.898289561284954,22.7425688502952));
#6595=CARTESIAN_POINT('Ctrl Pts',(1.35029124254801,0.859867100264678,22.7400291929413));
#6596=CARTESIAN_POINT('Ctrl Pts',(1.33202552699521,0.790555204235873,22.7355114739159));
#6597=CARTESIAN_POINT('Ctrl Pts',(1.3243900999343,0.759741024881772,22.7335253060678));
#6598=CARTESIAN_POINT('Ctrl Pts',(1.31340444736956,0.712422226474213,22.7305083674589));
#6599=CARTESIAN_POINT('Ctrl Pts',(1.30972638013775,0.695996488163972,22.7294671460978));
#6600=CARTESIAN_POINT('Ctrl Pts',(1.30352618638333,0.667252998798782,22.7276554295386));
#6601=CARTESIAN_POINT('Ctrl Pts',(1.30094716564796,0.654948020704576,22.7268831307363));
#6602=CARTESIAN_POINT('Ctrl Pts',(1.29528109268812,0.627103577644397,22.7251428135002));
#6603=CARTESIAN_POINT('Ctrl Pts',(1.29223647376713,0.611555733953299,22.7241761651552));
#6604=CARTESIAN_POINT('Ctrl Pts',(1.28429407231168,0.5693485638147,22.7215654979395));
#6605=CARTESIAN_POINT('Ctrl Pts',(1.27961769371987,0.542648508570418,22.719928521869));
#6606=CARTESIAN_POINT('Ctrl Pts',(1.25861232981692,0.413121273881187,22.7120532666378));
#6607=CARTESIAN_POINT('Ctrl Pts',(1.24693488088784,0.309597115909877,22.7059625753096));
#6608=CARTESIAN_POINT('Ctrl Pts',(1.22309922846906,-0.0631150060972825,
22.6845068547967));
#6609=CARTESIAN_POINT('Ctrl Pts',(1.23967379372005,-0.332980062856612,22.6699329128804));
#6610=CARTESIAN_POINT('Ctrl Pts',(1.30564715605125,-0.682578152014254,22.6494563207962));
#6611=CARTESIAN_POINT('Ctrl Pts',(1.32508972884309,-0.76684569151032,22.6443844389545));
#6612=CARTESIAN_POINT('Ctrl Pts',(1.35224852690691,-0.866143539675064,22.6381358663738));
#6613=CARTESIAN_POINT('Ctrl Pts',(1.35672548134662,-0.882031444980441,22.6371276487459));
#6614=CARTESIAN_POINT('Ctrl Pts',(1.36386749809754,-0.906651084201533,22.6355512076021));
#6615=CARTESIAN_POINT('Ctrl Pts',(1.36644801963986,-0.915407327220928,22.6349877413193));
#6616=CARTESIAN_POINT('Ctrl Pts',(1.37131540556405,-0.931668264966201,22.633935952838));
#6617=CARTESIAN_POINT('Ctrl Pts',(1.37359250223412,-0.939175677202566,22.6334481959179));
#6618=CARTESIAN_POINT('Ctrl Pts',(1.37888074389968,-0.956384133657861,22.6323252297143));
#6619=CARTESIAN_POINT('Ctrl Pts',(1.38191034813374,-0.966079280127706,22.6316889670965));
#6620=CARTESIAN_POINT('Ctrl Pts',(1.39002068726323,-0.991608895626863,22.6300043572313));
#6621=CARTESIAN_POINT('Ctrl Pts',(1.39517816511764,-1.00741841101432,22.6289517986947));
#6622=CARTESIAN_POINT('Ctrl Pts',(1.43674560697618,-1.13157029147617,22.6206162147378));
#6623=CARTESIAN_POINT('Ctrl Pts',(1.47877010224343,-1.23793555430004,22.6130570289752));
#6624=CARTESIAN_POINT('Ctrl Pts',(1.59844683068817,-1.49927018963793,22.5937779688046));
#6625=CARTESIAN_POINT('Ctrl Pts',(1.68311679716082,-1.6506430934314,22.5819647930069));
#6626=CARTESIAN_POINT('Ctrl Pts',(1.86334364871756,-1.91949702857235,22.5603320580885));
#6627=CARTESIAN_POINT('Ctrl Pts',(1.95580873112871,-2.03849871830021,22.550477276464));
#6628=CARTESIAN_POINT('Ctrl Pts',(2.08174172089787,-2.17904675773991,22.538527634413));
#6629=CARTESIAN_POINT('Ctrl Pts',(2.10772107653243,-2.20702465349966,22.5361311741812));
#6630=CARTESIAN_POINT('Ctrl Pts',(2.14674754234381,-2.24758353535667,22.5326291537913));
#6631=CARTESIAN_POINT('Ctrl Pts',(2.15941269267318,-2.26052589135035,22.5315073136945));
#6632=CARTESIAN_POINT('Ctrl Pts',(2.18208772346199,-2.28330985685264,22.5295243610722));
#6633=CARTESIAN_POINT('Ctrl Pts',(2.19205399567784,-2.29319401570863,22.5286613687559));
#6634=CARTESIAN_POINT('Ctrl Pts',(2.21314708876907,-2.31384172537308,22.526852612463));
#6635=CARTESIAN_POINT('Ctrl Pts',(2.22428755373985,-2.32459087452439,22.5259074899587));
#6636=CARTESIAN_POINT('Ctrl Pts',(2.25394372076184,-2.35279556750469,22.5234179454305));
#6637=CARTESIAN_POINT('Ctrl Pts',(2.27258967899555,-2.37011302683431,22.5218794679856));
#6638=CARTESIAN_POINT('Ctrl Pts',(2.35512792653043,-2.44496941042161,22.5151822613708));
#6639=CARTESIAN_POINT('Ctrl Pts',(2.42110612888967,-2.50016191562204,22.5101214905855));
#6640=CARTESIAN_POINT('Ctrl Pts',(2.67123371974969,-2.69292758761975,22.4918365526643));
#6641=CARTESIAN_POINT('Ctrl Pts',(2.86772546851955,-2.81332900681846,22.4792188084483));
#6642=CARTESIAN_POINT('Ctrl Pts',(3.20560327854733,-2.97358929848789,22.4581436942687));
#6643=CARTESIAN_POINT('Ctrl Pts',(3.33983383040673,-3.02655147521524,22.4498958437639));
#6644=CARTESIAN_POINT('Ctrl Pts',(3.49454632389235,-3.07589921555084,22.4400613858485));
#6645=CARTESIAN_POINT('Ctrl Pts',(3.51200055550013,-3.08130338405846,22.4389472594558));
#6646=CARTESIAN_POINT('Ctrl Pts',(3.53860047828569,-3.08929199756158,22.4372409995548));
#6647=CARTESIAN_POINT('Ctrl Pts',(3.54771353621437,-3.09198498911904,22.4366549572409));
#6648=CARTESIAN_POINT('Ctrl Pts',(3.56434541547401,-3.09681998241459,22.4355824712363));
#6649=CARTESIAN_POINT('Ctrl Pts',(3.57186025092031,-3.09897496808296,22.4350967863488));
#6650=CARTESIAN_POINT('Ctrl Pts',(3.58870562528697,-3.10373935265144,22.4340055983626));
#6651=CARTESIAN_POINT('Ctrl Pts',(3.59804004512471,-3.10633400801682,22.433399275725));
#6652=CARTESIAN_POINT('Ctrl Pts',(3.6253140676919,-3.11378294999352,22.4316230988031));
#6653=CARTESIAN_POINT('Ctrl Pts',(3.64328378947108,-3.1185240997136,22.4304470859493));
#6654=CARTESIAN_POINT('Ctrl Pts',(3.81317022196487,-3.16177894966179,22.4192812796471));
#6655=CARTESIAN_POINT('Ctrl Pts',(3.96764951185471,-3.18931401920795,22.4087785785176));
#6656=CARTESIAN_POINT('Ctrl Pts',(4.40187603116108,-3.234419180028,22.3792887450694));
#6657=CARTESIAN_POINT('Ctrl Pts',(4.68289869584216,-3.2269549758532,22.3603596064908));
#6658=CARTESIAN_POINT('Ctrl Pts',(4.99781640975944,-3.17719518399707,22.340161950366));
#6659=CARTESIAN_POINT('Ctrl Pts',(5.0360694071743,-3.17044000781401,22.3377229769926));
#6660=CARTESIAN_POINT('Ctrl Pts',(5.09208672285232,-3.15949999688685,22.334171231863));
#6661=CARTESIAN_POINT('Ctrl Pts',(5.10995142454861,-3.15585342917296,22.3330415090427));
#6662=CARTESIAN_POINT('Ctrl Pts',(5.1415282961356,-3.14912828068964,22.3310496692376));
#6663=CARTESIAN_POINT('Ctrl Pts',(5.1552529529293,-3.14611127702715,22.3301856131744));
#6664=CARTESIAN_POINT('Ctrl Pts',(5.18399301652166,-3.13959618468013,22.3283795956119));
#6665=CARTESIAN_POINT('Ctrl Pts',(5.19900396946497,-3.13607991491364,22.3274382405512));
#6666=CARTESIAN_POINT('Ctrl Pts',(5.23844099492223,-3.12654287950546,22.3249698421697));
#6667=CARTESIAN_POINT('Ctrl Pts',(5.26282310449792,-3.12034352215674,22.3234485597827));
#6668=CARTESIAN_POINT('Ctrl Pts',(5.36760289800328,-3.09239217888041,22.3169289563497));
#6669=CARTESIAN_POINT('Ctrl Pts',(5.44721705513011,-3.06781264097421,22.3120221268178));
#6670=CARTESIAN_POINT('Ctrl Pts',(5.74479433618588,-2.96314527865529,22.2937338165805));
#6671=CARTESIAN_POINT('Ctrl Pts',(5.95482415443133,-2.86268168304686,22.2809869827984));
#6672=CARTESIAN_POINT('Ctrl Pts',(6.27558666625827,-2.66420113742317,22.2597335331932));
#6673=CARTESIAN_POINT('Ctrl Pts',(6.39362236700104,-2.57964784707828,22.2514378014791));
#6674=CARTESIAN_POINT('Ctrl Pts',(6.51966205056492,-2.47582043721844,22.2415486800561));
#6675=CARTESIAN_POINT('Ctrl Pts',(6.53367680368052,-2.46407388464559,22.2404336692325));
#6676=CARTESIAN_POINT('Ctrl Pts',(6.55482339236202,-2.44604113016822,22.2387263342749));
#6677=CARTESIAN_POINT('Ctrl Pts',(6.56202889477642,-2.43984136616794,22.2381401132628));
#6678=CARTESIAN_POINT('Ctrl Pts',(6.57511025561722,-2.42848478701234,22.2370674593006));
#6679=CARTESIAN_POINT('Ctrl Pts',(6.58099488163586,-2.42333838059769,22.2365817866953));
#6680=CARTESIAN_POINT('Ctrl Pts',(6.59412784798021,-2.41176832750362,22.23549082747));
#6681=CARTESIAN_POINT('Ctrl Pts',(6.60136592252056,-2.40533344953659,22.2348847229809));
#6682=CARTESIAN_POINT('Ctrl Pts',(6.62239675839439,-2.38646596035163,22.2331097613032));
#6683=CARTESIAN_POINT('Ctrl Pts',(6.63611094039606,-2.37394688468426,22.2319347578213));
#6684=CARTESIAN_POINT('Ctrl Pts',(6.75506206696603,-2.26346197338259,22.221594619939));
#6685=CARTESIAN_POINT('Ctrl Pts',(6.85373091292243,-2.15868391139478,22.2119966297143));
#6686=CARTESIAN_POINT('Ctrl Pts',(7.1236822730977,-1.83060606387584,22.1833402296544));
#6687=CARTESIAN_POINT('Ctrl Pts',(7.27316871492922,-1.59103939593297,22.164247297868));
#6688=CARTESIAN_POINT('Ctrl Pts',(7.40908317398408,-1.29243325749105,22.1433548892878));
#6689=CARTESIAN_POINT('Ctrl Pts',(7.42756459086342,-1.24936205723947,22.1404017610917));
#6690=CARTESIAN_POINT('Ctrl Pts',(7.45244975772723,-1.18768818246058,22.1362560437119));
#6691=CARTESIAN_POINT('Ctrl Pts',(7.45963212804002,-1.16940804457714,22.1350373995376));
#6692=CARTESIAN_POINT('Ctrl Pts',(7.471744889861,-1.13773161435172,22.1329428293128));
#6693=CARTESIAN_POINT('Ctrl Pts',(7.47675415114854,-1.12436628173937,22.1320642826363));
#6694=CARTESIAN_POINT('Ctrl Pts',(7.4861932591141,-1.09866325329039,22.1303845649077));
#6695=CARTESIAN_POINT('Ctrl Pts',(7.49063693466362,-1.08633097331331,22.1295829475777));
#6696=CARTESIAN_POINT('Ctrl Pts',(7.50092387874953,-1.05722662207765,22.1277010633123));
#6697=CARTESIAN_POINT('Ctrl Pts',(7.50670402697339,-1.04043257355392,22.1266228975944));
#6698=CARTESIAN_POINT('Ctrl Pts',(7.52638612418755,-0.981672747244577,22.1228767092465));
#6699=CARTESIAN_POINT('Ctrl Pts',(7.53956357991476,-0.939468269751344,22.1202323800905));
#6700=CARTESIAN_POINT('Ctrl Pts',(7.63634895762852,-0.605479453082931,22.0996355702265));
#6701=CARTESIAN_POINT('Ctrl Pts',(7.67921910621616,-0.303509123726089,22.0831558719124));
#6702=CARTESIAN_POINT('Ctrl Pts',(7.67921910621823,-2.19652074306964E-11,
22.0659612921829));
#6703=CARTESIAN_POINT('Origin',(4.45646910621825,-5.13094777615093E-16,
-2.31077344927308));
#6704=CARTESIAN_POINT('',(7.67921910621823,-1.24761686023381E-10,20.8155686056964));
#6705=CARTESIAN_POINT('',(7.67921910621823,2.36916961325777E-11,21.0595336661193));
#6706=CARTESIAN_POINT('',(7.67921910621823,-3.51191647465084E-13,-2.31077344927308));
#6707=CARTESIAN_POINT('Ctrl Pts',(7.67921910621823,2.36916961325777E-11,
21.0595336661193));
#6708=CARTESIAN_POINT('Ctrl Pts',(7.67921910621822,-0.0894454910351407,
21.0655592747916));
#6709=CARTESIAN_POINT('Ctrl Pts',(7.67549535737132,-0.178852116290269,21.0716247501547));
#6710=CARTESIAN_POINT('Ctrl Pts',(7.65085338500985,-0.47416340077961,21.0916381005274));
#6711=CARTESIAN_POINT('Ctrl Pts',(7.61383322363013,-0.678232801453661,21.1053943607614));
#6712=CARTESIAN_POINT('Ctrl Pts',(7.54610867038377,-0.917601779018526,21.1211849998897));
#6713=CARTESIAN_POINT('Ctrl Pts',(7.53394389311208,-0.957608929184082,21.1238140557288));
#6714=CARTESIAN_POINT('Ctrl Pts',(7.51525570954617,-1.01503055376256,21.127574415035));
#6715=CARTESIAN_POINT('Ctrl Pts',(7.50935519689536,-1.03264178216326,21.1287259328489));
#6716=CARTESIAN_POINT('Ctrl Pts',(7.49869163720208,-1.06357879489786,21.1307458908836));
#6717=CARTESIAN_POINT('Ctrl Pts',(7.49399249617127,-1.07692592438826,21.1316164115736));
#6718=CARTESIAN_POINT('Ctrl Pts',(7.48408836325053,-1.10447634813449,21.1334115044832));
#6719=CARTESIAN_POINT('Ctrl Pts',(7.47887096463145,-1.11867483552624,21.1343356396432));
#6720=CARTESIAN_POINT('Ctrl Pts',(7.46518053903198,-1.15513656798424,21.1367065737599));
#6721=CARTESIAN_POINT('Ctrl Pts',(7.45656020364345,-1.1773438029629,21.1381484314018));
#6722=CARTESIAN_POINT('Ctrl Pts',(7.41836543690256,-1.27259477372468,21.1443258095959));
#6723=CARTESIAN_POINT('Ctrl Pts',(7.38636233326804,-1.34463916919134,21.1489793599));
#6724=CARTESIAN_POINT('Ctrl Pts',(7.29112616054644,-1.53944418116927,21.1615863163779));
#6725=CARTESIAN_POINT('Ctrl Pts',(7.222597558429,-1.65942956209022,21.1693730409075));
#6726=CARTESIAN_POINT('Ctrl Pts',(7.02631843218325,-1.95695932259459,21.1893377020436));
#6727=CARTESIAN_POINT('Ctrl Pts',(6.88784907837612,-2.12654272502494,21.2013650111882));
#6728=CARTESIAN_POINT('Ctrl Pts',(6.70683449527531,-2.30724378010995,21.2165516493302));
#6729=CARTESIAN_POINT('Ctrl Pts',(6.6798903114792,-2.33322011720834,21.2188009880095));
#6730=CARTESIAN_POINT('Ctrl Pts',(6.6429474989928,-2.36761487407249,21.2218803009897));
#6731=CARTESIAN_POINT('Ctrl Pts',(6.63333998719551,-2.37645136876482,21.2226807020673));
#6732=CARTESIAN_POINT('Ctrl Pts',(6.61810042741656,-2.39029797529074,21.2239501566707));
#6733=CARTESIAN_POINT('Ctrl Pts',(6.61250390650538,-2.39534722257058,21.2244163146513));
#6734=CARTESIAN_POINT('Ctrl Pts',(6.60093970677717,-2.40570721898283,21.2253796072465));
#6735=CARTESIAN_POINT('Ctrl Pts',(6.59496997749778,-2.41101542884926,21.2258769315176));
#6736=CARTESIAN_POINT('Ctrl Pts',(6.58059567866102,-2.42370149521078,21.2270744274556));
#6737=CARTESIAN_POINT('Ctrl Pts',(6.57217236120537,-2.43105786886688,21.2277761573094));
#6738=CARTESIAN_POINT('Ctrl Pts',(6.54299151151208,-2.45627598917897,21.2302066292236));
#6739=CARTESIAN_POINT('Ctrl Pts',(6.5220453528253,-2.47391635597328,21.231950317318));
#6740=CARTESIAN_POINT('Ctrl Pts',(6.47015241808022,-2.51650091854812,21.2362626328236));
#6741=CARTESIAN_POINT('Ctrl Pts',(6.43896460881141,-2.54114317711107,21.2388478855091));
#6742=CARTESIAN_POINT('Ctrl Pts',(6.30940305325885,-2.63967605003347,21.2495354859299));
#6743=CARTESIAN_POINT('Ctrl Pts',(6.20729682729648,-2.70847791366628,21.2578340162899));
#6744=CARTESIAN_POINT('Ctrl Pts',(5.8778325078872,-2.90405024984104,21.2837479604227));
#6745=CARTESIAN_POINT('Ctrl Pts',(5.63885164786643,-3.00928612023419,21.3012537384686));
#6746=CARTESIAN_POINT('Ctrl Pts',(5.35211587014347,-3.09604315387601,21.3202384389464));
#6747=CARTESIAN_POINT('Ctrl Pts',(5.31424098962029,-3.10674974091398,21.3227102895318));
#6748=CARTESIAN_POINT('Ctrl Pts',(5.25864212906571,-3.12137225987302,21.3262882427625));
#6749=CARTESIAN_POINT('Ctrl Pts',(5.24106726070012,-3.12583622424566,21.3274119285351));
#6750=CARTESIAN_POINT('Ctrl Pts',(5.20977818947903,-3.1335030371891,21.3293997703925));
#6751=CARTESIAN_POINT('Ctrl Pts',(5.1960790307242,-3.13676473911685,21.3302658005443));
#6752=CARTESIAN_POINT('Ctrl Pts',(5.16743269590826,-3.14338719069717,21.3320679753663));
#6753=CARTESIAN_POINT('Ctrl Pts',(5.15248202146617,-3.14673136619804,21.3330035692662));
#6754=CARTESIAN_POINT('Ctrl Pts',(5.11335845295876,-3.15519007412421,21.3354392348696));
#6755=CARTESIAN_POINT('Ctrl Pts',(5.0891493032062,-3.16013351583897,21.3369338268248));
#6756=CARTESIAN_POINT('Ctrl Pts',(4.97856444449615,-3.18139288246952,21.3437066779751));
#6757=CARTESIAN_POINT('Ctrl Pts',(4.89159611255751,-3.19444998641969,21.3488813123645));
#6758=CARTESIAN_POINT('Ctrl Pts',(4.53099757776638,-3.23358622794944,21.3698795915762));
#6759=CARTESIAN_POINT('Ctrl Pts',(4.25515117475932,-3.22817197185011,21.3847631102892));
#6760=CARTESIAN_POINT('Ctrl Pts',(3.95846915963551,-3.18413977105302,21.4019122577136));
#6761=CARTESIAN_POINT('Ctrl Pts',(3.93363729602362,-3.18015673820093,21.4033573875573));
#6762=CARTESIAN_POINT('Ctrl Pts',(3.83366412538272,-3.16291847664373,21.4092237497656));
#6763=CARTESIAN_POINT('Ctrl Pts',(3.75896354248865,-3.14728825433992,21.4137173148762));
#6764=CARTESIAN_POINT('Ctrl Pts',(3.6688682437167,-3.12507198372703,21.4193482724277));
#6765=CARTESIAN_POINT('Ctrl Pts',(3.65287292847748,-3.12099714494885,21.4203561909509));
#6766=CARTESIAN_POINT('Ctrl Pts',(3.62798401336539,-3.11445263178789,21.4219383589673));
#6767=CARTESIAN_POINT('Ctrl Pts',(3.61906826906285,-3.11206725147489,21.4225079054173));
#6768=CARTESIAN_POINT('Ctrl Pts',(3.60260332888467,-3.10758623029718,21.4235650561599));
#6769=CARTESIAN_POINT('Ctrl Pts',(3.59505141809514,-3.1055013293777,21.4240520423586));
#6770=CARTESIAN_POINT('Ctrl Pts',(3.57785946651129,-3.10068751080452,21.4251654496892));
#6771=CARTESIAN_POINT('Ctrl Pts',(3.56822454399584,-3.09794117600695,21.4257928551082));
#6772=CARTESIAN_POINT('Ctrl Pts',(3.53859031269174,-3.08934463637538,21.4277327700116));
#6773=CARTESIAN_POINT('Ctrl Pts',(3.5186352652549,-3.0833454875905,21.4290534079612));
#6774=CARTESIAN_POINT('Ctrl Pts',(3.47217292080582,-3.06888461610578,21.4321596364767));
#6775=CARTESIAN_POINT('Ctrl Pts',(3.44571455669976,-3.06027235690635,21.4339524883671));
#6776=CARTESIAN_POINT('Ctrl Pts',(3.35292308249869,-3.02873393904662,21.4403170890623));
#6777=CARTESIAN_POINT('Ctrl Pts',(3.28723359685712,-3.00398572042259,21.4449620019285));
#6778=CARTESIAN_POINT('Ctrl Pts',(3.02360682805531,-2.89470831696087,21.4640416878018));
#6779=CARTESIAN_POINT('Ctrl Pts',(2.83354117659888,-2.79258758091511,21.4787801662447));
#6780=CARTESIAN_POINT('Ctrl Pts',(2.54241612605463,-2.5963394411612,21.5020622783845));
#6781=CARTESIAN_POINT('Ctrl Pts',(2.4346605484506,-2.51333957911612,21.5108752289492));
#6782=CARTESIAN_POINT('Ctrl Pts',(2.31085882361731,-2.4048489757991,21.5212284748952));
#6783=CARTESIAN_POINT('Ctrl Pts',(2.28951655508618,-2.38563593368456,21.5230225235111));
#6784=CARTESIAN_POINT('Ctrl Pts',(2.25641861588488,-2.35502934090511,21.5258201889696));
#6785=CARTESIAN_POINT('Ctrl Pts',(2.24448850554569,-2.34382746689756,21.5268318381654));
#6786=CARTESIAN_POINT('Ctrl Pts',(2.22357001165559,-2.32388389911429,21.5286116461956));
#6787=CARTESIAN_POINT('Ctrl Pts',(2.2145464253113,-2.31517978630887,21.5293813960359));
#6788=CARTESIAN_POINT('Ctrl Pts',(2.19395062645879,-2.29507983716735,21.5311430550137));
#6789=CARTESIAN_POINT('Ctrl Pts',(2.18241324388054,-2.28364867706766,21.532133395554));
#6790=CARTESIAN_POINT('Ctrl Pts',(2.15055942767161,-2.25160733954792,21.5348778668066));
#6791=CARTESIAN_POINT('Ctrl Pts',(2.13043314104628,-2.23080968000344,21.5366236516257));
#6792=CARTESIAN_POINT('Ctrl Pts',(2.00284300402277,-2.09535903842841,21.547774270745));
#6793=CARTESIAN_POINT('Ctrl Pts',(1.90359990188212,-1.97324057836944,21.5568202207237));
#6794=CARTESIAN_POINT('Ctrl Pts',(1.72959015113515,-1.7238982203473,21.573998039871));
#6795=CARTESIAN_POINT('Ctrl Pts',(1.65386141776108,-1.59783721366861,21.5821335627164));
#6796=CARTESIAN_POINT('Ctrl Pts',(1.51940519627895,-1.33484802773763,21.5987599413172));
#6797=CARTESIAN_POINT('Ctrl Pts',(1.46104025906988,-1.19814793962146,21.6072366142313));
#6798=CARTESIAN_POINT('Ctrl Pts',(1.40621283385749,-1.040384239427,21.6173446317372));
#6799=CARTESIAN_POINT('Ctrl Pts',(1.40026635069164,-1.02278412810262,21.6184767573136));
#6800=CARTESIAN_POINT('Ctrl Pts',(1.39145111896337,-0.995929790645079,21.6202123511876));
#6801=CARTESIAN_POINT('Ctrl Pts',(1.38847127691293,-0.986712077442884,21.6208095512638));
#6802=CARTESIAN_POINT('Ctrl Pts',(1.38316161464555,-0.97003080218331,21.621893173514));
#6803=CARTESIAN_POINT('Ctrl Pts',(1.38081734729296,-0.962572049203439,21.6223787447266));
#6804=CARTESIAN_POINT('Ctrl Pts',(1.37568311791045,-0.946026221909996,21.6234582388265));
#6805=CARTESIAN_POINT('Ctrl Pts',(1.37290623901174,-0.936935406975188,21.6240528880964));
#6806=CARTESIAN_POINT('Ctrl Pts',(1.36490598090118,-0.910323717797833,21.6257978371717));
#6807=CARTESIAN_POINT('Ctrl Pts',(1.35979153204007,-0.892770852123789,21.6269541281712));
#6808=CARTESIAN_POINT('Ctrl Pts',(1.31552139319692,-0.73587652615707,21.6373311068377));
#6809=CARTESIAN_POINT('Ctrl Pts',(1.28564910399624,-0.594102511906308,21.646992972663));
#6810=CARTESIAN_POINT('Ctrl Pts',(1.23304972865414,-0.221785400111993,21.6723549792319));
#6811=CARTESIAN_POINT('Ctrl Pts',(1.22544067477768,0.0101004426984798,21.6880895363299));
#6812=CARTESIAN_POINT('Ctrl Pts',(1.24901447328468,0.324695961601183,21.7085949282752));
#6813=CARTESIAN_POINT('Ctrl Pts',(1.25858162227676,0.40830187080147,21.7139706268327));
#6814=CARTESIAN_POINT('Ctrl Pts',(1.27526938171719,0.516455552410367,21.720831495374));
#6815=CARTESIAN_POINT('Ctrl Pts',(1.27942311766867,0.541421157809245,21.7224088106833));
#6816=CARTESIAN_POINT('Ctrl Pts',(1.28658581201005,0.581546384167389,21.7249341213125));
#6817=CARTESIAN_POINT('Ctrl Pts',(1.28941041419239,0.596737421631965,21.7258879144106));
#6818=CARTESIAN_POINT('Ctrl Pts',(1.29501097510969,0.625697462857361,21.7277020814093));
#6819=CARTESIAN_POINT('Ctrl Pts',(1.29776790337114,0.639469741876472,21.7285630375081));
#6820=CARTESIAN_POINT('Ctrl Pts',(1.30429766848937,0.671016341099972,21.7305312245234));
#6821=CARTESIAN_POINT('Ctrl Pts',(1.30813098596696,0.688777761266104,21.7316365005493));
#6822=CARTESIAN_POINT('Ctrl Pts',(1.32055441664901,0.744069107095733,21.7350690100018));
#6823=CARTESIAN_POINT('Ctrl Pts',(1.32966713815272,0.781478994718531,21.7373795361948));
#6824=CARTESIAN_POINT('Ctrl Pts',(1.37833664070143,0.966773416103719,21.7487775609975));
#6825=CARTESIAN_POINT('Ctrl Pts',(1.42772616266441,1.11187869866018,21.7575435006204));
#6826=CARTESIAN_POINT('Ctrl Pts',(1.58826818280931,1.49233236978607,21.7808127820048));
#6827=CARTESIAN_POINT('Ctrl Pts',(1.71785298017699,1.71859785588417,21.7949288367245));
#6828=CARTESIAN_POINT('Ctrl Pts',(1.8942320225445,1.95507044815074,21.8124780230518));
#6829=CARTESIAN_POINT('Ctrl Pts',(1.91576151570319,1.98296849161809,21.8145987811537));
#6830=CARTESIAN_POINT('Ctrl Pts',(1.94569545738399,2.02046918814093,21.8175274985888));
#6831=CARTESIAN_POINT('Ctrl Pts',(1.9537067162284,2.03038431401583,21.8183094403864));
#6832=CARTESIAN_POINT('Ctrl Pts',(1.96651026687984,2.04603969996539,21.8195566563613));
#6833=CARTESIAN_POINT('Ctrl Pts',(1.97126417698393,2.0518113783838,21.8200192091416));
#6834=CARTESIAN_POINT('Ctrl Pts',(1.98116414620967,2.06374595847814,21.8209814930568));
#6835=CARTESIAN_POINT('Ctrl Pts',(1.98631317191332,2.06990620101082,21.8214814540787));
#6836=CARTESIAN_POINT('Ctrl Pts',(1.99883438458165,2.08477320014454,21.822695848065));
#6837=CARTESIAN_POINT('Ctrl Pts',(2.00622985554705,2.09346013248053,21.8234119510475));
#6838=CARTESIAN_POINT('Ctrl Pts',(2.03245383391905,2.12393425508118,21.8259465838964));
#6839=CARTESIAN_POINT('Ctrl Pts',(2.05152745412194,2.14550746360978,21.8277817803363));
#6840=CARTESIAN_POINT('Ctrl Pts',(2.09946087266566,2.19828021194679,21.8323671820227));
#6841=CARTESIAN_POINT('Ctrl Pts',(2.12865310768617,2.22916935986334,21.8351366945353));
#6842=CARTESIAN_POINT('Ctrl Pts',(2.25526601364536,2.35794260166899,21.847019801996));
#6843=CARTESIAN_POINT('Ctrl Pts',(2.35831015677296,2.45008438041535,21.8563705800867));
#6844=CARTESIAN_POINT('Ctrl Pts',(2.65408776794743,2.68218776490518,21.8818052850557));
#6845=CARTESIAN_POINT('Ctrl Pts',(2.85695405217752,2.80789952646256,21.8977370870686));
#6846=CARTESIAN_POINT('Ctrl Pts',(3.10883363862467,2.92774218726787,21.9154330318392));
#6847=CARTESIAN_POINT('Ctrl Pts',(3.14615824177829,2.94463603105719,21.9180079327265));
#6848=CARTESIAN_POINT('Ctrl Pts',(3.20072188468266,2.96808960208253,21.9217056011462));
#6849=CARTESIAN_POINT('Ctrl Pts',(3.21770988823403,2.97521975538536,21.9228476573256));
#6850=CARTESIAN_POINT('Ctrl Pts',(3.24782988275535,2.98755892487783,21.9248566463485));
#6851=CARTESIAN_POINT('Ctrl Pts',(3.26093660661545,2.99282795272288,21.9257255892417));
#6852=CARTESIAN_POINT('Ctrl Pts',(3.2882071600684,3.00358324039593,21.9275228297402));
#6853=CARTESIAN_POINT('Ctrl Pts',(3.30237600513869,3.00905589566496,21.9284506529152));
#6854=CARTESIAN_POINT('Ctrl Pts',(3.33913167830573,3.02295480789258,21.9308424726539));
#6855=CARTESIAN_POINT('Ctrl Pts',(3.36177556497799,3.03122826547182,21.9323013563788));
#6856=CARTESIAN_POINT('Ctrl Pts',(3.46148456705871,3.06639615675739,21.938663949643));
#6857=CARTESIAN_POINT('Ctrl Pts',(3.53946620878464,3.09061271400874,21.9434792585718));
#6858=CARTESIAN_POINT('Ctrl Pts',(3.75926544729736,3.14981603179832,21.9566958957305));
#6859=CARTESIAN_POINT('Ctrl Pts',(3.90266692027411,3.17816637382334,21.9649080721699));
#6860=CARTESIAN_POINT('Ctrl Pts',(4.26975206053431,3.22512905950818,21.9856162192215));
#6861=CARTESIAN_POINT('Ctrl Pts',(4.49432918449552,3.23030322141188,21.9979845982489));
#6862=CARTESIAN_POINT('Ctrl Pts',(4.74234183679792,3.21014190544409,22.0129333669061));
#6863=CARTESIAN_POINT('Ctrl Pts',(4.76706886993191,3.20784381987485,22.0144384806114));
#6864=CARTESIAN_POINT('Ctrl Pts',(4.80169248772744,3.20422190126414,22.0165697153987));
#6865=CARTESIAN_POINT('Ctrl Pts',(4.81161393414145,3.20313741834048,22.0171831609168));
#6866=CARTESIAN_POINT('Ctrl Pts',(4.82879782551084,3.20117828224483,22.0182506384496));
#6867=CARTESIAN_POINT('Ctrl Pts',(4.83606269285441,3.20032494856243,22.0187034866824));
#6868=CARTESIAN_POINT('Ctrl Pts',(4.85144942568593,3.19846448927855,22.0196660050579));
#6869=CARTESIAN_POINT('Ctrl Pts',(4.85957044359388,3.19745114888469,22.0201760306036));
#6870=CARTESIAN_POINT('Ctrl Pts',(4.87978011043599,3.19485117188573,22.0214501310605));
#6871=CARTESIAN_POINT('Ctrl Pts',(4.89186368327318,3.1932268581928,22.0222162719655));
#6872=CARTESIAN_POINT('Ctrl Pts',(4.9377573612177,3.18679234397094,22.0251418639114));
#6873=CARTESIAN_POINT('Ctrl Pts',(4.97149814749713,3.18151358584001,22.0273253121985));
#6874=CARTESIAN_POINT('Ctrl Pts',(5.05793222290102,3.16658003655403,22.0329917053537));
#6875=CARTESIAN_POINT('Ctrl Pts',(5.11047900795235,3.15614597707446,22.0365066121112));
#6876=CARTESIAN_POINT('Ctrl Pts',(5.37600886758146,3.09650499856864,22.0545486725428));
#6877=CARTESIAN_POINT('Ctrl Pts',(5.58385238359823,3.02702960087466,22.0695478175534));
#6878=CARTESIAN_POINT('Ctrl Pts',(5.9260116787953,2.872483857061,22.0945969601111));
#6879=CARTESIAN_POINT('Ctrl Pts',(6.06406677136233,2.79756344843145,22.1048268122199));
#6880=CARTESIAN_POINT('Ctrl Pts',(6.22077774984749,2.69707056955922,22.1165432524591));
#6881=CARTESIAN_POINT('Ctrl Pts',(6.24520609819517,2.68093168722429,22.1183733665403));
#6882=CARTESIAN_POINT('Ctrl Pts',(6.28314942412115,2.65511443686881,22.1212226677672));
#6883=CARTESIAN_POINT('Ctrl Pts',(6.29681474923133,2.64566089804919,22.1222502352182));
#6884=CARTESIAN_POINT('Ctrl Pts',(6.32152865269249,2.62827991960129,22.1241113656387));
#6885=CARTESIAN_POINT('Ctrl Pts',(6.33260126592329,2.62038748584474,22.1249462343892));
#6886=CARTESIAN_POINT('Ctrl Pts',(6.34399004651055,2.61216049787625,22.1258060860518));
#6887=CARTESIAN_POINT('Ctrl Pts',(6.34435630426618,2.61189580461282,22.1258337397009));
#6888=CARTESIAN_POINT('Ctrl Pts',(6.34504919044514,2.61139483618877,22.1258860571886));
#6889=CARTESIAN_POINT('Ctrl Pts',(6.34537583019483,2.61115857678696,22.1259107216306));
#6890=CARTESIAN_POINT('Ctrl Pts',(6.3459960143008,2.61070981869984,22.1259575533618));
#6891=CARTESIAN_POINT('Ctrl Pts',(6.34628956714124,2.61049733179346,22.125979721103));
#6892=CARTESIAN_POINT('Ctrl Pts',(6.3468486986376,2.61009246322941,22.1260219456231));
#6893=CARTESIAN_POINT('Ctrl Pts',(6.34711428377475,2.60990009054467,22.1260420027471));
#6894=CARTESIAN_POINT('Ctrl Pts',(6.34762155982898,2.60953253453672,22.1260803137403));
#6895=CARTESIAN_POINT('Ctrl Pts',(6.3478632557635,2.60935735817646,22.1260985678763));
#6896=CARTESIAN_POINT('Ctrl Pts',(6.34832605018759,2.60902183598569,22.1261335215613));
#6897=CARTESIAN_POINT('Ctrl Pts',(6.34854715262481,2.60886149563399,22.12615022132));
#6898=CARTESIAN_POINT('Ctrl Pts',(6.34897145727519,2.60855371360722,22.1261822697158));
#6899=CARTESIAN_POINT('Ctrl Pts',(6.34917466262908,2.60840627630392,22.1261976185194));
#6900=CARTESIAN_POINT('Ctrl Pts',(6.34956540418965,2.60812270087323,22.1262271333225));
#6901=CARTESIAN_POINT('Ctrl Pts',(6.34975294294202,2.60798656626216,22.1262412994573));
#6902=CARTESIAN_POINT('Ctrl Pts',(6.35011421497847,2.60772425894134,22.1262685895347));
#6903=CARTESIAN_POINT('Ctrl Pts',(6.35028795033722,2.60759808909706,22.1262817135877));
#6904=CARTESIAN_POINT('Ctrl Pts',(6.35062318612198,2.60735458346847,22.1263070380061));
#6905=CARTESIAN_POINT('Ctrl Pts',(6.35078468826022,2.60723725003747,22.1263192384625));
#6906=CARTESIAN_POINT('Ctrl Pts',(6.35109679167411,2.60701045848802,22.1263428163573));
#6907=CARTESIAN_POINT('Ctrl Pts',(6.35124739435295,2.60690100233497,22.1263541938698));
#6908=CARTESIAN_POINT('Ctrl Pts',(6.35153884022466,2.60668914450413,22.1263762120114));
#6909=CARTESIAN_POINT('Ctrl Pts',(6.35167968461711,2.60658674445104,22.1263868527045));
#6910=CARTESIAN_POINT('Ctrl Pts',(6.35195259690634,2.60638829142875,22.1264074713941));
#6911=CARTESIAN_POINT('Ctrl Pts',(6.35208466580213,2.60629223983641,22.1264174494436));
#6912=CARTESIAN_POINT('Ctrl Pts',(6.35234087880805,2.60610587044467,22.1264368071289));
#6913=CARTESIAN_POINT('Ctrl Pts',(6.35246502374482,2.60601555382763,22.1264461868081));
#6914=CARTESIAN_POINT('Ctrl Pts',(6.35270613085828,2.60584011977123,22.1264644037604));
#6915=CARTESIAN_POINT('Ctrl Pts',(6.35282309375787,2.60575500332775,22.1264732410718));
#6916=CARTESIAN_POINT('Ctrl Pts',(6.36701439829685,2.59542622110449,22.1275455025337));
#6917=CARTESIAN_POINT('Ctrl Pts',(6.38100572782112,2.58506854703074,22.1286045210584));
#6918=CARTESIAN_POINT('Ctrl Pts',(6.4104590061279,2.56289284395919,22.1308382690139));
#6919=CARTESIAN_POINT('Ctrl Pts',(6.42589925953707,2.55104707029468,22.1320118739534));
#6920=CARTESIAN_POINT('Ctrl Pts',(6.53075741584978,2.46908037118173,22.1400022485682));
#6921=CARTESIAN_POINT('Ctrl Pts',(6.61652507837474,2.3944085061937,22.1466350720116));
#6922=CARTESIAN_POINT('Ctrl Pts',(6.90642010198939,2.11373462169066,22.1697460066299));
#6923=CARTESIAN_POINT('Ctrl Pts',(7.08648568047272,1.88497055543233,22.1853274524097));
#6924=CARTESIAN_POINT('Ctrl Pts',(7.26354373765657,1.58428152051933,22.2057145623015));
#6925=CARTESIAN_POINT('Ctrl Pts',(7.29214449780761,1.53250122818785,22.2092271134562));
#6926=CARTESIAN_POINT('Ctrl Pts',(7.32639037032406,1.46625636434933,22.2137602395819));
#6927=CARTESIAN_POINT('Ctrl Pts',(7.33337955504677,1.45249510696921,22.2147040193848));
#6928=CARTESIAN_POINT('Ctrl Pts',(7.34424066702408,1.43072433046129,22.2162012410957));
#6929=CARTESIAN_POINT('Ctrl Pts',(7.34817884068541,1.42274787095117,22.2167506661345));
#6930=CARTESIAN_POINT('Ctrl Pts',(7.35554743527964,1.40766638578361,22.2177913152666));
#6931=CARTESIAN_POINT('Ctrl Pts',(7.35898483508735,1.4005649753479,22.2182821021845));
#6932=CARTESIAN_POINT('Ctrl Pts',(7.36695539085149,1.38394304063307,22.2194326076356));
#6933=CARTESIAN_POINT('Ctrl Pts',(7.3714679269336,1.37441282759032,22.2200935697106));
#6934=CARTESIAN_POINT('Ctrl Pts',(7.38594975152599,1.34343591638403,22.2222458049025));
#6935=CARTESIAN_POINT('Ctrl Pts',(7.39572948222556,1.32190214411775,22.2237479003812));
#6936=CARTESIAN_POINT('Ctrl Pts',(7.44706623151683,1.2054781188722,22.2318933834356));
#6937=CARTESIAN_POINT('Ctrl Pts',(7.48426325738744,1.10874125717241,22.2387460001017));
#6938=CARTESIAN_POINT('Ctrl Pts',(7.61355085875772,0.717156085212655,22.2663877879574));
#6939=CARTESIAN_POINT('Ctrl Pts',(7.6677405817972,0.41144478362888,22.2875509873347));
#6940=CARTESIAN_POINT('Ctrl Pts',(7.67866302492731,0.0687969074833208,22.3094304860775));
#6941=CARTESIAN_POINT('Ctrl Pts',(7.67920843263985,0.0349000051372115,22.3115779087787));
#6942=CARTESIAN_POINT('Ctrl Pts',(7.67921895108708,0.000999948906710003,
22.3137088975806));
#6943=CARTESIAN_POINT('',(7.67921822734991,-0.00238007247472413,20.815728761447));
#6944=CARTESIAN_POINT('Ctrl Pts',(7.67921910621823,-2.19646041259736E-11,
22.0659612921829));
#6945=CARTESIAN_POINT('Ctrl Pts',(7.67921910621824,0.000842109108049127,
22.0659135845146));
#6946=CARTESIAN_POINT('Ctrl Pts',(7.67921877615567,0.00168423000929225,
22.0658658700222));
#6947=CARTESIAN_POINT('Ctrl Pts',(7.67912126048857,0.126079561885152,22.0588167216195));
#6948=CARTESIAN_POINT('Ctrl Pts',(7.67191931405605,0.24951134855579,22.051690097904));
#6949=CARTESIAN_POINT('Ctrl Pts',(7.65572397793286,0.388799127737251,22.0432006959801));
#6950=CARTESIAN_POINT('Ctrl Pts',(7.65366618859104,0.405373020163533,22.0421832630709));
#6951=CARTESIAN_POINT('Ctrl Pts',(7.65016125844979,0.431913667158585,22.0405412467));
#6952=CARTESIAN_POINT('Ctrl Pts',(7.6487960258009,0.441891175805831,22.0399210637177));
#6953=CARTESIAN_POINT('Ctrl Pts',(7.64628295121627,0.459637761990175,22.0388125532577));
#6954=CARTESIAN_POINT('Ctrl Pts',(7.64515344738692,0.467409251919766,22.0383252587355));
#6955=CARTESIAN_POINT('Ctrl Pts',(7.64265763604375,0.48415137067857,22.0372713886317));
#6956=CARTESIAN_POINT('Ctrl Pts',(7.64128186846532,0.493120230770056,22.0367043123262));
#6957=CARTESIAN_POINT('Ctrl Pts',(7.63733615137166,0.5181375918353,22.0351157470899));
#6958=CARTESIAN_POINT('Ctrl Pts',(7.63468268707784,0.534172380154636,22.0340897559942));
#6959=CARTESIAN_POINT('Ctrl Pts',(7.61800360356846,0.630436935911772,22.0278860413881));
#6960=CARTESIAN_POINT('Ctrl Pts',(7.60106307384245,0.710124985476,22.0225662729259));
#6961=CARTESIAN_POINT('Ctrl Pts',(7.54145529904885,0.946164657647747,22.0064167459452));
#6962=CARTESIAN_POINT('Ctrl Pts',(7.4899976845368,1.10003164587155,21.995377230245));
#6963=CARTESIAN_POINT('Ctrl Pts',(7.34547094238736,1.44368286573009,21.9702396457718));
#6964=CARTESIAN_POINT('Ctrl Pts',(7.24487274784753,1.62953552915293,21.9563053998555));
#6965=CARTESIAN_POINT('Ctrl Pts',(7.11147812723515,1.82696352195835,21.941303067941));
#6966=CARTESIAN_POINT('Ctrl Pts',(7.0958458931962,1.84947529400642,21.9395883740116));
#6967=CARTESIAN_POINT('Ctrl Pts',(7.0697577452087,1.88603994531729,21.9367959574913));
#6968=CARTESIAN_POINT('Ctrl Pts',(7.05947131823346,1.90021148550149,21.9357118405982));
#6969=CARTESIAN_POINT('Ctrl Pts',(7.04077082619802,1.92553820546547,21.9337707666036));
#6970=CARTESIAN_POINT('Ctrl Pts',(7.03239881726623,1.93672375265293,21.9329122116886));
#6971=CARTESIAN_POINT('Ctrl Pts',(7.01438729306753,1.96046490835058,21.9310870189626));
#6972=CARTESIAN_POINT('Ctrl Pts',(7.00472745497092,1.97300469068947,21.930121207837));
#6973=CARTESIAN_POINT('Ctrl Pts',(6.97831712824019,2.00677134669496,21.9275153111671));
#6974=CARTESIAN_POINT('Ctrl Pts',(6.96139101780366,2.02785970140345,21.9258822233686));
#6975=CARTESIAN_POINT('Ctrl Pts',(6.86879011112797,2.14030296978391,21.9171394742127));
#6976=CARTESIAN_POINT('Ctrl Pts',(6.78837611166571,2.22764531667753,21.9102263459081));
#6977=CARTESIAN_POINT('Ctrl Pts',(6.59210561128341,2.41852051185743,21.8945744984749));
#6978=CARTESIAN_POINT('Ctrl Pts',(6.47322207354766,2.51851034840963,21.8859535260676));
#6979=CARTESIAN_POINT('Ctrl Pts',(6.2106578648704,2.70878953694886,21.8677970235736));
#6980=CARTESIAN_POINT('Ctrl Pts',(6.06613393139463,2.7970849342464,21.8582745128319));
#6981=CARTESIAN_POINT('Ctrl Pts',(5.89132580071345,2.88583282597355,21.8465224427134));
#6982=CARTESIAN_POINT('Ctrl Pts',(5.86712792267801,2.89773815739771,21.8448905250422));
#6983=CARTESIAN_POINT('Ctrl Pts',(5.83346392538425,2.91377923435332,21.8426092607368));
#6984=CARTESIAN_POINT('Ctrl Pts',(5.82412230723014,2.9181756070509,21.8419750658686));
#6985=CARTESIAN_POINT('Ctrl Pts',(5.80804707284597,2.92564682727969,21.8408814833456));
#6986=CARTESIAN_POINT('Ctrl Pts',(5.80132362287688,2.92874353337133,21.8404234220518));
#6987=CARTESIAN_POINT('Ctrl Pts',(5.78723110209174,2.93517554853987,21.8394617888629));
#6988=CARTESIAN_POINT('Ctrl Pts',(5.77986009468512,2.93850630031104,21.8389579335414));
#6989=CARTESIAN_POINT('Ctrl Pts',(5.76177285848519,2.94659755966904,21.8377195405781));
#6990=CARTESIAN_POINT('Ctrl Pts',(5.75104309548055,2.95132736928182,21.836983173722));
#6991=CARTESIAN_POINT('Ctrl Pts',(5.71196146689861,2.96830090043147,21.8342954498185));
#6992=CARTESIAN_POINT('Ctrl Pts',(5.6834607985182,2.98019504844327,21.8323247193045));
#6993=CARTESIAN_POINT('Ctrl Pts',(5.61144889062973,3.00903964505913,21.8273265000807));
#6994=CARTESIAN_POINT('Ctrl Pts',(5.56773282375193,3.0254570557488,21.824275253203));
#6995=CARTESIAN_POINT('Ctrl Pts',(5.21018577466158,3.15093802191481,21.799265532027));
#6996=CARTESIAN_POINT('Ctrl Pts',(4.88154189409492,3.2118355338613,21.7762187141575));
#6997=CARTESIAN_POINT('Ctrl Pts',(4.48214848204969,3.22334844004773,21.7504640284719));
#6998=CARTESIAN_POINT('Ctrl Pts',(4.41491971886507,3.22318310433417,21.746192976532));
#6999=CARTESIAN_POINT('Ctrl Pts',(4.32448134831466,3.22013018766958,21.7405304896149));
#7000=CARTESIAN_POINT('Ctrl Pts',(4.30123033828528,3.21909306549873,21.7390820533646));
#7001=CARTESIAN_POINT('Ctrl Pts',(4.26300839351863,3.21697306755446,21.736712615184));
#7002=CARTESIAN_POINT('Ctrl Pts',(4.24803047448806,3.21603733089037,21.7357870478897));
#7003=CARTESIAN_POINT('Ctrl Pts',(4.21889362710179,3.21401261560774,21.7339920546336));
#7004=CARTESIAN_POINT('Ctrl Pts',(4.20473430682369,3.21293460912538,21.7331223067461));
#7005=CARTESIAN_POINT('Ctrl Pts',(4.17143177881153,3.21017764990761,21.7310824416129));
#7006=CARTESIAN_POINT('Ctrl Pts',(4.15229541567964,3.20842098433393,21.7299147843668));
#7007=CARTESIAN_POINT('Ctrl Pts',(4.08906129528561,3.20204542696027,21.7260703552774));
#7008=CARTESIAN_POINT('Ctrl Pts',(4.04504199275132,3.19668757202262,21.7234167158049));
#7009=CARTESIAN_POINT('Ctrl Pts',(3.94042109426429,3.18175652466718,21.7171537219483));
#7010=CARTESIAN_POINT('Ctrl Pts',(3.8799540333302,3.17135793517871,21.7135694708794));
#7011=CARTESIAN_POINT('Ctrl Pts',(3.6420033517624,3.1234060132616,21.699547077474));
#7012=CARTESIAN_POINT('Ctrl Pts',(3.46752971828005,3.07262476574035,21.6894690763852));
#7013=CARTESIAN_POINT('Ctrl Pts',(3.13728345856494,2.94544041364587,21.6696597843506));
#7014=CARTESIAN_POINT('Ctrl Pts',(2.98157454690569,2.87063431478247,21.6599599185457));
#7015=CARTESIAN_POINT('Ctrl Pts',(2.80932594678627,2.77015598152087,21.6480060112895));
#7016=CARTESIAN_POINT('Ctrl Pts',(2.78620525234023,2.75627707245762,21.6463741857773));
#7017=CARTESIAN_POINT('Ctrl Pts',(2.75447775967312,2.73668588080824,21.6440930290269));
#7018=CARTESIAN_POINT('Ctrl Pts',(2.74571946668359,2.7312194745257,21.6434588477069));
#7019=CARTESIAN_POINT('Ctrl Pts',(2.73072705892367,2.72176169842072,21.6423652831093));
#7020=CARTESIAN_POINT('Ctrl Pts',(2.72448008833745,2.71779071970731,21.6419072261066));
#7021=CARTESIAN_POINT('Ctrl Pts',(2.71143555587516,2.70943553147768,21.6409455946213));
#7022=CARTESIAN_POINT('Ctrl Pts',(2.70464077409589,2.70504722338562,21.6404417366692));
#7023=CARTESIAN_POINT('Ctrl Pts',(2.68803614146954,2.69423457013526,21.6392033264973));
#7024=CARTESIAN_POINT('Ctrl Pts',(2.6782447505816,2.6877822085799,21.6384669449442));
#7025=CARTESIAN_POINT('Ctrl Pts',(2.64279374941111,2.66414209470341,21.6357791058896));
#7026=CARTESIAN_POINT('Ctrl Pts',(2.61734724537921,2.64663975979544,21.6338082727896));
#7027=CARTESIAN_POINT('Ctrl Pts',(2.55406673726221,2.60176159871099,21.6288097369357));
#7028=CARTESIAN_POINT('Ctrl Pts',(2.5165696675721,2.57392461349346,21.625758272399));
#7029=CARTESIAN_POINT('Ctrl Pts',(2.21723170070704,2.34144596281452,21.6007429055165));
#7030=CARTESIAN_POINT('Ctrl Pts',(1.98785158780413,2.09822690457166,21.5776903687778));
#7031=CARTESIAN_POINT('Ctrl Pts',(1.76168105448884,1.76882526761004,21.5519357139471));
#7032=CARTESIAN_POINT('Ctrl Pts',(1.72541411513742,1.71229821669841,21.5476690793576));
#7033=CARTESIAN_POINT('Ctrl Pts',(1.67899274227599,1.63471215597493,21.5420114411486));
#7034=CARTESIAN_POINT('Ctrl Pts',(1.66726434443109,1.61461934447604,21.5405635608198));
#7035=CARTESIAN_POINT('Ctrl Pts',(1.64833090244838,1.58136097600671,21.5381947940013));
#7036=CARTESIAN_POINT('Ctrl Pts',(1.64099857096971,1.56826923237064,21.5372693472328));
#7037=CARTESIAN_POINT('Ctrl Pts',(1.62690526103363,1.54268845630915,21.535474421338));
#7038=CARTESIAN_POINT('Ctrl Pts',(1.62013488366135,1.5302050239555,21.5346046214852));
#7039=CARTESIAN_POINT('Ctrl Pts',(1.60439522989349,1.50072037171207,21.5325643789903));
#7040=CARTESIAN_POINT('Ctrl Pts',(1.59549504204625,1.48368273528748,21.5313963989991));
#7041=CARTESIAN_POINT('Ctrl Pts',(1.56655655349929,1.42705699209951,21.5275497547784));
#7042=CARTESIAN_POINT('Ctrl Pts',(1.54718282513905,1.38713367897605,21.5248942604633));
#7043=CARTESIAN_POINT('Ctrl Pts',(1.50298042613934,1.29104290849796,21.5186261199715));
#7044=CARTESIAN_POINT('Ctrl Pts',(1.47892009986949,1.23454029530846,21.5150386345858));
#7045=CARTESIAN_POINT('Ctrl Pts',(1.39010477320703,1.00823796581482,21.5009952647507));
#7046=CARTESIAN_POINT('Ctrl Pts',(1.33814465599626,0.833781208828499,21.4909008008378));
#7047=CARTESIAN_POINT('Ctrl Pts',(1.29682924988139,0.635017363350291,21.4795366082732));
#7048=CARTESIAN_POINT('Ctrl Pts',(1.29270209432549,0.614124873587356,21.4783434322785));
#7049=CARTESIAN_POINT('Ctrl Pts',(1.28391381252941,0.567194921616959,21.4756635988978));
#7050=CARTESIAN_POINT('Ctrl Pts',(1.27936558250794,0.541138009763068,21.4741759175493));
#7051=CARTESIAN_POINT('Ctrl Pts',(1.25317484229494,0.379357777084059,21.4649262768301));
#7052=CARTESIAN_POINT('Ctrl Pts',(1.23991480680202,0.24243698799337,21.4570445553621));
#7053=CARTESIAN_POINT('Ctrl Pts',(1.23488242236496,0.0882176054906887,21.4477055315022));
#7054=CARTESIAN_POINT('Ctrl Pts',(1.23446416447521,0.0713248557818932,21.4466763225296));
#7055=CARTESIAN_POINT('Ctrl Pts',(1.23400772808643,0.0443035399910697,21.4450189352054));
#7056=CARTESIAN_POINT('Ctrl Pts',(1.23388441389743,0.0341764767837041,21.4443952891196));
#7057=CARTESIAN_POINT('Ctrl Pts',(1.23375018772044,0.0161897629948173,21.4432829426017));
#7058=CARTESIAN_POINT('Ctrl Pts',(1.23372028906768,0.00833043366257391,
21.4427953024419));
#7059=CARTESIAN_POINT('Ctrl Pts',(1.23371782024977,-0.00856522920951279,
21.441743476549));
#7060=CARTESIAN_POINT('Ctrl Pts',(1.23375450402847,-0.0176012072661911,
21.441178810483));
#7061=CARTESIAN_POINT('Ctrl Pts',(1.23396208780022,-0.0427156442270686,
21.4396036675532));
#7062=CARTESIAN_POINT('Ctrl Pts',(1.23421531739218,-0.0587929031799864,
21.4385888073402));
#7063=CARTESIAN_POINT('Ctrl Pts',(1.23640685526231,-0.153104865227369,21.4325998571954));
#7064=CARTESIAN_POINT('Ctrl Pts',(1.24107392493832,-0.231243755721218,21.4274946066202));
#7065=CARTESIAN_POINT('Ctrl Pts',(1.26852818691636,-0.516142733974112,21.4085329069887));
#7066=CARTESIAN_POINT('Ctrl Pts',(1.30846833788901,-0.720738339356372,21.3942788224359));
#7067=CARTESIAN_POINT('Ctrl Pts',(1.4159776506892,-1.08164476805225,21.3690791194112));
#7068=CARTESIAN_POINT('Ctrl Pts',(1.47672252803411,-1.23922133088451,21.3580489650839));
#7069=CARTESIAN_POINT('Ctrl Pts',(1.56130457477777,-1.41593910835468,21.3457147415664));
#7070=CARTESIAN_POINT('Ctrl Pts',(1.57338978496306,-1.4403870741801,21.3440086551491));
#7071=CARTESIAN_POINT('Ctrl Pts',(1.59372382682094,-1.48024059512673,21.3412273471052));
#7072=CARTESIAN_POINT('Ctrl Pts',(1.60179001493065,-1.4957372961789,21.3401458168145));
#7073=CARTESIAN_POINT('Ctrl Pts',(1.61653148676677,-1.5235048332093,21.3382075659164));
#7074=CARTESIAN_POINT('Ctrl Pts',(1.62316124558087,-1.53579921727494,21.3373492667883));
#7075=CARTESIAN_POINT('Ctrl Pts',(1.63748709261377,-1.56195690460794,21.3355227071192));
#7076=CARTESIAN_POINT('Ctrl Pts',(1.64520600613941,-1.57580733627731,21.3345552872252));
#7077=CARTESIAN_POINT('Ctrl Pts',(1.666425171527,-1.61322976135414,21.3319403215778));
#7078=CARTESIAN_POINT('Ctrl Pts',(1.68012191952706,-1.63668927653366,21.3302998586874));
#7079=CARTESIAN_POINT('Ctrl Pts',(1.75625636033325,-1.763384299147,21.3214292851569));
#7080=CARTESIAN_POINT('Ctrl Pts',(1.82416046896246,-1.86323079765025,21.3144029243599));
#7081=CARTESIAN_POINT('Ctrl Pts',(1.99520160425979,-2.08664967404673,21.2983286802267));
#7082=CARTESIAN_POINT('Ctrl Pts',(2.10230341826476,-2.20677375784047,21.2894119699326));
#7083=CARTESIAN_POINT('Ctrl Pts',(2.26992793408395,-2.36862449357437,21.2763535845023));
#7084=CARTESIAN_POINT('Ctrl Pts',(2.32361041720719,-2.41707622317187,21.2722852571039));
#7085=CARTESIAN_POINT('Ctrl Pts',(2.40575465883652,-2.4863475517751,21.2661513034181));
#7086=CARTESIAN_POINT('Ctrl Pts',(2.43300286609687,-2.50857292856336,21.2641306474073));
#7087=CARTESIAN_POINT('Ctrl Pts',(2.51632649544916,-2.57429605687005,21.2579754354103));
#7088=CARTESIAN_POINT('Ctrl Pts',(2.57347651286352,-2.61638888851312,21.2537855601515));
#7089=CARTESIAN_POINT('Ctrl Pts',(2.64529077923625,-2.66571041118799,21.2484964762904));
#7090=CARTESIAN_POINT('Ctrl Pts',(2.65868567611587,-2.6747623524345,21.2475089463438));
#7091=CARTESIAN_POINT('Ctrl Pts',(2.67976890916512,-2.68877997032381,21.2459520850319));
#7092=CARTESIAN_POINT('Ctrl Pts',(2.68741146762053,-2.69381446753511,21.2453872193123));
#7093=CARTESIAN_POINT('Ctrl Pts',(2.7016426836614,-2.70310253085828,21.2443342297044));
#7094=CARTESIAN_POINT('Ctrl Pts',(2.70822551498868,-2.70736466085925,21.2438466834194));
#7095=CARTESIAN_POINT('Ctrl Pts',(2.72334210443495,-2.71707395075883,21.2427260529807));
#7096=CARTESIAN_POINT('Ctrl Pts',(2.73188599051141,-2.72250493639574,21.2420919321062));
#7097=CARTESIAN_POINT('Ctrl Pts',(2.75855799134515,-2.73928326418616,21.2401104069708));
#7098=CARTESIAN_POINT('Ctrl Pts',(2.77677314677391,-2.750490207647,21.2387543758944));
#7099=CARTESIAN_POINT('Ctrl Pts',(2.81975331529215,-2.77634776125233,21.2355506734605));
#7100=CARTESIAN_POINT('Ctrl Pts',(2.84460538034556,-2.79084945500261,21.2336951322606));
#7101=CARTESIAN_POINT('Ctrl Pts',(2.93388462219644,-2.84135549409408,21.2270271092326));
#7102=CARTESIAN_POINT('Ctrl Pts',(2.99934740231663,-2.87547553107803,21.2221343988962));
#7103=CARTESIAN_POINT('Ctrl Pts',(3.27239084094545,-3.00607038640625,21.201869056379));
#7104=CARTESIAN_POINT('Ctrl Pts',(3.48882004948076,-3.08255927008653,21.1861920592357));
#7105=CARTESIAN_POINT('Ctrl Pts',(3.77045289720855,-3.1494709691046,21.1671093530028));
#7106=CARTESIAN_POINT('Ctrl Pts',(3.82976275105909,-3.16180731092247,21.1631572100751));
#7107=CARTESIAN_POINT('Ctrl Pts',(3.95556899830644,-3.18429529347676,21.1549194014639));
#7108=CARTESIAN_POINT('Ctrl Pts',(4.02210756245774,-3.19405206028661,21.1506469766707));
#7109=CARTESIAN_POINT('Ctrl Pts',(4.11203066566997,-3.20437536527155,21.14498298276));
#7110=CARTESIAN_POINT('Ctrl Pts',(4.13518304041096,-3.20677947954871,21.1435343736363));
#7111=CARTESIAN_POINT('Ctrl Pts',(4.1733029143296,-3.21032080799395,21.1411647265495));
#7112=CARTESIAN_POINT('Ctrl Pts',(4.18825561295168,-3.21160463267941,21.1402391216426));
#7113=CARTESIAN_POINT('Ctrl Pts',(4.21737271767371,-3.21389982897593,21.1384441070594));
#7114=CARTESIAN_POINT('Ctrl Pts',(4.23153589202662,-3.21492212239086,21.1375743750853));
#7115=CARTESIAN_POINT('Ctrl Pts',(4.26487885882177,-3.2171073862618,21.1355346264945));
#7116=CARTESIAN_POINT('Ctrl Pts',(4.28406334268476,-3.21819251056869,21.1343670690558));
#7117=CARTESIAN_POINT('Ctrl Pts',(4.34753474400673,-3.2212134130724,21.1305233256148));
#7118=CARTESIAN_POINT('Ctrl Pts',(4.39185304959156,-3.22240711267805,21.1278702603562));
#7119=CARTESIAN_POINT('Ctrl Pts',(4.49750438496747,-3.22307214638956,21.1216088593854));
#7120=CARTESIAN_POINT('Ctrl Pts',(4.55882611790766,-3.22170787719385,21.1180256092012));
#7121=CARTESIAN_POINT('Ctrl Pts',(4.80113242525486,-3.20939113864234,21.1040096963537));
#7122=CARTESIAN_POINT('Ctrl Pts',(4.98109278024956,-3.18492680668508,21.0939367799592));
#7123=CARTESIAN_POINT('Ctrl Pts',(5.32659350340669,-3.10786449233529,21.0741221008113));
#7124=CARTESIAN_POINT('Ctrl Pts',(5.49182414907099,-3.05678971827337,21.0644115984847));
#7125=CARTESIAN_POINT('Ctrl Pts',(5.67714092167695,-2.98275080184001,21.0524483080475));
#7126=CARTESIAN_POINT('Ctrl Pts',(5.70200876037321,-2.97245233595862,21.0508194848186));
#7127=CARTESIAN_POINT('Ctrl Pts',(5.73622594850445,-2.95777727984837,21.0485418053271));
#7128=CARTESIAN_POINT('Ctrl Pts',(5.74568840241036,-2.95366511510209,21.047908037168));
#7129=CARTESIAN_POINT('Ctrl Pts',(5.761903858874,-2.94652548550338,21.046814996002));
#7130=CARTESIAN_POINT('Ctrl Pts',(5.76866654762435,-2.94352003599903,21.0463570464011));
#7131=CARTESIAN_POINT('Ctrl Pts',(5.78280060528964,-2.93718024173226,21.0453954162027));
#7132=CARTESIAN_POINT('Ctrl Pts',(5.79016981939347,-2.93384141024268,21.0448914507697));
#7133=CARTESIAN_POINT('Ctrl Pts',(5.80715073355459,-2.92607052777174,21.0437242977306));
#7134=CARTESIAN_POINT('Ctrl Pts',(5.81675330346425,-2.92161881279534,21.0430599285895));
#7135=CARTESIAN_POINT('Ctrl Pts',(5.8509235474757,-2.90557264219218,21.0406807027316));
#7136=CARTESIAN_POINT('Ctrl Pts',(5.87536556466588,-2.89371530992005,21.0389508831883));
#7137=CARTESIAN_POINT('Ctrl Pts',(5.93510858138337,-2.86379385046773,21.0346588040189));
#7138=CARTESIAN_POINT('Ctrl Pts',(5.97023102850904,-2.84538476673711,21.0320798171875));
#7139=CARTESIAN_POINT('Ctrl Pts',(6.11247463059183,-2.76745019535287,21.0214309892446));
#7140=CARTESIAN_POINT('Ctrl Pts',(6.21649385710969,-2.70248852536109,21.0131662447088));
#7141=CARTESIAN_POINT('Ctrl Pts',(6.52960296733948,-2.48118858601443,20.9872339417916));
#7142=CARTESIAN_POINT('Ctrl Pts',(6.72362101636808,-2.30526638462494,20.9696738125613));
#7143=CARTESIAN_POINT('Ctrl Pts',(6.92000852821356,-2.07813229303284,20.9506463919663));
#7144=CARTESIAN_POINT('Ctrl Pts',(6.94515379110272,-2.04795240893094,20.9481794437155));
#7145=CARTESIAN_POINT('Ctrl Pts',(6.98108259752001,-2.00319058298671,20.9446072734778));
#7146=CARTESIAN_POINT('Ctrl Pts',(6.99230406181366,-1.98896628721787,20.9434845470196));
#7147=CARTESIAN_POINT('Ctrl Pts',(7.01203124601801,-1.96352181317441,20.9414978810501));
#7148=CARTESIAN_POINT('Ctrl Pts',(7.02058443405943,-1.95233920124294,20.9406320740342));
#7149=CARTESIAN_POINT('Ctrl Pts',(7.03829419050025,-1.92886796618653,20.93882984984));
#7150=CARTESIAN_POINT('Ctrl Pts',(7.04743695544084,-1.91656933446637,20.9378939868921));
#7151=CARTESIAN_POINT('Ctrl Pts',(7.07110579319574,-1.88425165374463,20.9354564951519));
#7152=CARTESIAN_POINT('Ctrl Pts',(7.08548991676087,-1.86412953661981,20.9339603626393));
#7153=CARTESIAN_POINT('Ctrl Pts',(7.15010519603996,-1.77150273888731,20.9271679739803));
#7154=CARTESIAN_POINT('Ctrl Pts',(7.19758087514342,-1.69711686108284,20.9219761069846));
#7155=CARTESIAN_POINT('Ctrl Pts',(7.31045767863544,-1.50313728456852,20.9089851687597));
#7156=CARTESIAN_POINT('Ctrl Pts',(7.37143708304061,-1.38117257964705,20.9013225220935));
#7157=CARTESIAN_POINT('Ctrl Pts',(7.47487383296203,-1.13668513682375,20.886465823715));
#7158=CARTESIAN_POINT('Ctrl Pts',(7.51802321582908,-1.01474347804668,20.8792798363644));
#7159=CARTESIAN_POINT('Ctrl Pts',(7.58347539939457,-0.787104701564741,20.8657822333784));
#7160=CARTESIAN_POINT('Ctrl Pts',(7.60801366630656,-0.682249332651416,20.8595321725366));
#7161=CARTESIAN_POINT('Ctrl Pts',(7.63019193682435,-0.560240909038873,20.8520215108499));
#7162=CARTESIAN_POINT('Ctrl Pts',(7.63300152491294,-0.544084781188677,20.8510221893566));
#7163=CARTESIAN_POINT('Ctrl Pts',(7.63734026912222,-0.517955591880709,20.8493972704103));
#7164=CARTESIAN_POINT('Ctrl Pts',(7.638946142258,-0.507995333476345,20.8487758211932));
#7165=CARTESIAN_POINT('Ctrl Pts',(7.64171664784164,-0.490282690182273,20.8476667904289));
#7166=CARTESIAN_POINT('Ctrl Pts',(7.64289979624358,-0.482533391075683,20.847180257461));
#7167=CARTESIAN_POINT('Ctrl Pts',(7.64514623937996,-0.467451175904277,20.8462306880971));
#7168=CARTESIAN_POINT('Ctrl Pts',(7.64621250925745,-0.460118986323355,20.845767858341));
#7169=CARTESIAN_POINT('Ctrl Pts',(7.64853126191395,-0.443778630614379,20.8447338369327));
#7170=CARTESIAN_POINT('Ctrl Pts',(7.64977091030739,-0.434768745650329,20.8441619522962));
#7171=CARTESIAN_POINT('Ctrl Pts',(7.65277916626227,-0.41219729204756,20.8427251313785));
#7172=CARTESIAN_POINT('Ctrl Pts',(7.65449959599747,-0.398629626472879,20.8418577213568));
#7173=CARTESIAN_POINT('Ctrl Pts',(7.67141719267095,-0.258049455211929,20.8328342839026));
#7174=CARTESIAN_POINT('Ctrl Pts',(7.67912378100643,-0.130265619523243,20.8243335871624));
#7175=CARTESIAN_POINT('Ctrl Pts',(7.67921822734991,-0.00238007247472413,
20.815728761447));
#7176=CARTESIAN_POINT('Ctrl Pts',(7.67921822450325,-0.00238392389238244,
20.815729020591));
#7177=CARTESIAN_POINT('Ctrl Pts',(7.67921881231805,-0.00158927619454485,
20.8156755524433));
#7178=CARTESIAN_POINT('Ctrl Pts',(7.6792191062182,-0.000794634884726798,
20.8156220807944));
#7179=CARTESIAN_POINT('Ctrl Pts',(7.67921910621823,-1.24761686023381E-10,
20.8155686056964));
#7180=CARTESIAN_POINT('Origin',(4.45646910621825,-5.13094777615093E-16,
-2.31077344927308));
#7181=CARTESIAN_POINT('',(7.67921910621823,-8.48293998545729E-13,19.5612501365773));
#7182=CARTESIAN_POINT('',(7.67921910621823,5.28351711817002E-12,19.808946496524));
#7183=CARTESIAN_POINT('',(7.67921910621823,-3.51191647465084E-13,-2.31077344927308));
#7184=CARTESIAN_POINT('',(7.67921816809758,-0.00245899486517952,19.8090860941722));
#7185=CARTESIAN_POINT('Ctrl Pts',(7.67921910621823,5.28351711817003E-12,
19.808946496524));
#7186=CARTESIAN_POINT('Ctrl Pts',(7.67921910621823,-0.000819655941728086,
19.8089930222664));
#7187=CARTESIAN_POINT('Ctrl Pts',(7.67921879351827,-0.00163932095804614,
19.8090395547947));
#7188=CARTESIAN_POINT('Ctrl Pts',(7.67921816809758,-0.00245899486630962,
19.8090860941722));
#7189=CARTESIAN_POINT('Ctrl Pts',(7.67921816490598,-0.00246317421660369,
19.8090863314671));
#7190=CARTESIAN_POINT('Ctrl Pts',(7.67913282611117,-0.114118094441251,19.8154258682507));
#7191=CARTESIAN_POINT('Ctrl Pts',(7.67324495034378,-0.225684694903017,19.821876714552));
#7192=CARTESIAN_POINT('Ctrl Pts',(7.65995857656981,-0.352156167876153,19.8295423684475));
#7193=CARTESIAN_POINT('Ctrl Pts',(7.65822438964366,-0.367589223768464,19.8304838408652));
#7194=CARTESIAN_POINT('Ctrl Pts',(7.65520755005175,-0.392793903076085,19.8320321904543));
#7195=CARTESIAN_POINT('Ctrl Pts',(7.65399147657129,-0.402573431456799,19.8326356133735));
#7196=CARTESIAN_POINT('Ctrl Pts',(7.6517549709269,-0.419909450366868,19.8337102500715));
#7197=CARTESIAN_POINT('Ctrl Pts',(7.65075253204503,-0.427468240245285,19.8341804839197));
#7198=CARTESIAN_POINT('Ctrl Pts',(7.64866592955735,-0.442784780665778,19.8351368545086));
#7199=CARTESIAN_POINT('Ctrl Pts',(7.6475803123914,-0.450542105353103,19.8356230726358));
#7200=CARTESIAN_POINT('Ctrl Pts',(7.64515180075102,-0.467445926340511,19.8366866681174));
#7201=CARTESIAN_POINT('Ctrl Pts',(7.64379784965398,-0.476590491634979,19.8372646364939));
#7202=CARTESIAN_POINT('Ctrl Pts',(7.63990681365725,-0.502112110544535,19.8388846843901));
#7203=CARTESIAN_POINT('Ctrl Pts',(7.63728276071966,-0.518475338727434,19.8399314330506));
#7204=CARTESIAN_POINT('Ctrl Pts',(7.62169880203334,-0.611080461423574,19.8458982464262));
#7205=CARTESIAN_POINT('Ctrl Pts',(7.60612501604948,-0.686850740133894,19.8509449895099));
#7206=CARTESIAN_POINT('Ctrl Pts',(7.58240794903486,-0.784316482790087,19.8575911537956));
#7207=CARTESIAN_POINT('Ctrl Pts',(7.57673406295805,-0.806593179864548,19.8591208440121));
#7208=CARTESIAN_POINT('Ctrl Pts',(7.53812782042504,-0.951661329855261,19.8691447924729));
#7209=CARTESIAN_POINT('Ctrl Pts',(7.4981930612836,-1.0724709552804,19.8777804320858));
#7210=CARTESIAN_POINT('Ctrl Pts',(7.41174345647061,-1.28992011533772,19.8935855024148));
#7211=CARTESIAN_POINT('Ctrl Pts',(7.36734079704524,-1.38721622984992,19.9007608661631));
#7212=CARTESIAN_POINT('Ctrl Pts',(7.26101764104557,-1.59250607854635,19.9160234404596));
#7213=CARTESIAN_POINT('Ctrl Pts',(7.19750955614411,-1.69949164751796,19.9240543836823));
#7214=CARTESIAN_POINT('Ctrl Pts',(7.11265555434568,-1.82525091957933,19.9335828705979));
#7215=CARTESIAN_POINT('Ctrl Pts',(7.09705087750684,-1.84775413682039,19.9352918242933));
#7216=CARTESIAN_POINT('Ctrl Pts',(7.07193207395194,-1.88300928772761,19.9379761409524));
#7217=CARTESIAN_POINT('Ctrl Pts',(7.06260736855221,-1.89589395413968,19.9389586748279));
#7218=CARTESIAN_POINT('Ctrl Pts',(7.04491754736462,-1.91996020965646,19.9407969108687));
#7219=CARTESIAN_POINT('Ctrl Pts',(7.03657443257313,-1.93115743888423,19.9416534350849));
#7220=CARTESIAN_POINT('Ctrl Pts',(7.01767059842093,-1.95618693372098,19.9435710764523));
#7221=CARTESIAN_POINT('Ctrl Pts',(7.00707003257307,-1.96998866399782,19.9446306024861));
#7222=CARTESIAN_POINT('Ctrl Pts',(6.97971122053792,-2.0050182557509,19.9473256454622));
#7223=CARTESIAN_POINT('Ctrl Pts',(6.96279641038478,-2.02612252463055,19.948954937408));
#7224=CARTESIAN_POINT('Ctrl Pts',(6.84403145326458,-2.17053966883919,19.9601494409179));
#7225=CARTESIAN_POINT('Ctrl Pts',(6.7333849345405,-2.28634205844877,19.9693413166352));
#7226=CARTESIAN_POINT('Ctrl Pts',(6.41817885596634,-2.57055430412483,19.9932929457057));
#7227=CARTESIAN_POINT('Ctrl Pts',(6.20075118951711,-2.72277401004116,20.0076333202954));
#7228=CARTESIAN_POINT('Ctrl Pts',(5.94474967140447,-2.85863345708013,20.0248481903556));
#7229=CARTESIAN_POINT('Ctrl Pts',(5.9221466880512,-2.87028803880192,20.0263713570415));
#7230=CARTESIAN_POINT('Ctrl Pts',(5.8822049854042,-2.89028803914877,20.0290727052385));
#7231=CARTESIAN_POINT('Ctrl Pts',(5.86492476126281,-2.8987480699643,20.0302445693536));
#7232=CARTESIAN_POINT('Ctrl Pts',(5.83884695124865,-2.91122698844464,20.0320193148926));
#7233=CARTESIAN_POINT('Ctrl Pts',(5.83010498220628,-2.91536199454235,20.0326153061962));
#7234=CARTESIAN_POINT('Ctrl Pts',(5.82131746409663,-2.91947024704796,20.0332155841384));
#7235=CARTESIAN_POINT('Ctrl Pts',(5.82129026071566,-2.91948296443702,20.0332174424207));
#7236=CARTESIAN_POINT('Ctrl Pts',(5.82123556182638,-2.91950853485101,20.0332211789634));
#7237=CARTESIAN_POINT('Ctrl Pts',(5.82120806627845,-2.91952138788447,20.0332230572269));
#7238=CARTESIAN_POINT('Ctrl Pts',(5.82115277914063,-2.9195472313871,20.0332268340001));
#7239=CARTESIAN_POINT('Ctrl Pts',(5.82112498756047,-2.91956022184148,20.0332287325095));
#7240=CARTESIAN_POINT('Ctrl Pts',(5.82106910441031,-2.91958634200046,20.0332325500452));
#7241=CARTESIAN_POINT('Ctrl Pts',(5.82104101284883,-2.91959947169059,20.0332344690711));
#7242=CARTESIAN_POINT('Ctrl Pts',(5.82098452576975,-2.91962587214329,20.0332383279115));
#7243=CARTESIAN_POINT('Ctrl Pts',(5.82095613021751,-2.91963914291132,20.0332402677286));
#7244=CARTESIAN_POINT('Ctrl Pts',(5.82089903104375,-2.91966582740976,20.0332441684331));
#7245=CARTESIAN_POINT('Ctrl Pts',(5.82087032748953,-2.91967924109775,20.0332461293162));
#7246=CARTESIAN_POINT('Ctrl Pts',(5.82081260819859,-2.91970621332517,20.0332500724346));
#7247=CARTESIAN_POINT('Ctrl Pts',(5.82078359246063,-2.91971977185393,20.0332520546703));
#7248=CARTESIAN_POINT('Ctrl Pts',(5.82072524470242,-2.91974703564475,20.0332560407746));
#7249=CARTESIAN_POINT('Ctrl Pts',(5.82069591257783,-2.91976074094403,20.0332580446508));
#7250=CARTESIAN_POINT('Ctrl Pts',(5.82063692773613,-2.91978830025504,20.0332620743315));
#7251=CARTESIAN_POINT('Ctrl Pts',(5.820607275043,-2.91980215424376,20.0332641001347));
#7252=CARTESIAN_POINT('Ctrl Pts',(5.82054764473718,-2.91983001291971,20.033268173966));
#7253=CARTESIAN_POINT('Ctrl Pts',(5.82051766708296,-2.91984401761422,20.0332702219972));
#7254=CARTESIAN_POINT('Ctrl Pts',(5.82045738241223,-2.91987217974078,20.033274340589));
#7255=CARTESIAN_POINT('Ctrl Pts',(5.8204270754542,-2.9198863371331,20.0332764111459));
#7256=CARTESIAN_POINT('Ctrl Pts',(5.82036612773428,-2.9199148066927,20.0332805750934));
#7257=CARTESIAN_POINT('Ctrl Pts',(5.8203354869391,-2.91992911886281,20.0332826684865));
#7258=CARTESIAN_POINT('Ctrl Pts',(5.82027386698238,-2.91995790007082,20.0332868784192));
#7259=CARTESIAN_POINT('Ctrl Pts',(5.82024288786449,-2.9199723690753,20.0332889949561));
#7260=CARTESIAN_POINT('Ctrl Pts',(5.82018058667748,-2.92000146605419,20.0332932514904));
#7261=CARTESIAN_POINT('Ctrl Pts',(5.82014926456717,-2.92001609403448,20.0332953914911));
#7262=CARTESIAN_POINT('Ctrl Pts',(5.82008627264695,-2.92004551114234,20.0332996952783));
#7263=CARTESIAN_POINT('Ctrl Pts',(5.82005460292467,-2.92006030021529,20.0333018590593));
#7264=CARTESIAN_POINT('Ctrl Pts',(5.81999091104595,-2.92009004167821,20.0333062107317));
#7265=CARTESIAN_POINT('Ctrl Pts',(5.81995888886353,-2.92010499406627,20.0333083986253));
#7266=CARTESIAN_POINT('Ctrl Pts',(5.8198944872475,-2.92013506436638,20.0333127988532));
#7267=CARTESIAN_POINT('Ctrl Pts',(5.81986210780262,-2.92015018226933,20.0333150111886));
#7268=CARTESIAN_POINT('Ctrl Pts',(5.81979698678821,-2.92018058583132,20.0333194606342));
#7269=CARTESIAN_POINT('Ctrl Pts',(5.81976424512392,-2.92019587151987,20.0333216977512));
#7270=CARTESIAN_POINT('Ctrl Pts',(5.8196983945757,-2.92022661298732,20.0333261971092));
#7271=CARTESIAN_POINT('Ctrl Pts',(5.81966528577417,-2.92024206871264,20.0333284593449));
#7272=CARTESIAN_POINT('Ctrl Pts',(5.8195986958551,-2.92027315258719,20.0333330092897));
#7273=CARTESIAN_POINT('Ctrl Pts',(5.81956521474586,-2.92028878071707,20.0333352969986));
#7274=CARTESIAN_POINT('Ctrl Pts',(5.81949787507735,-2.92032021175049,20.0333398982416));
#7275=CARTESIAN_POINT('Ctrl Pts',(5.81946401650961,-2.92033601464212,20.0333422117767));
#7276=CARTESIAN_POINT('Ctrl Pts',(5.81939591671594,-2.92036779758206,20.0333468650294));
#7277=CARTESIAN_POINT('Ctrl Pts',(5.81936167542007,-2.92038377764672,20.0333492047521));
#7278=CARTESIAN_POINT('Ctrl Pts',(5.81929280483042,-2.92041591737568,20.0333539107459));
#7279=CARTESIAN_POINT('Ctrl Pts',(5.81925817549578,-2.92043207704234,20.0333562770202));
#7280=CARTESIAN_POINT('Ctrl Pts',(5.81918852336661,-2.92046457847383,20.0333610364918));
#7281=CARTESIAN_POINT('Ctrl Pts',(5.81915350056692,-2.92048092022395,20.0333634296898));
#7282=CARTESIAN_POINT('Ctrl Pts',(5.81908305596489,-2.92051378835703,20.0333682433888));
#7283=CARTESIAN_POINT('Ctrl Pts',(5.81904763417721,-2.92053031471561,20.0333706638893));
#7284=CARTESIAN_POINT('Ctrl Pts',(5.81897638601533,-2.92056355461796,20.033375532576));
#7285=CARTESIAN_POINT('Ctrl Pts',(5.8189405596092,-2.92058026815862,20.0333779807649));
#7286=CARTESIAN_POINT('Ctrl Pts',(5.81886849642417,-2.92061388507026,20.0333829052254));
#7287=CARTESIAN_POINT('Ctrl Pts',(5.81883225976557,-2.92063078836666,20.0333853814892));
#7288=CARTESIAN_POINT('Ctrl Pts',(5.81875937034235,-2.92066478740855,20.0333903624926));
#7289=CARTESIAN_POINT('Ctrl Pts',(5.81872271753058,-2.92068188315709,20.0333928672358));
#7290=CARTESIAN_POINT('Ctrl Pts',(5.81864898991746,-2.92071626979044,20.0333979056017));
#7291=CARTESIAN_POINT('Ctrl Pts',(5.81861191514423,-2.9207335606427,20.0334004392228));
#7292=CARTESIAN_POINT('Ctrl Pts',(5.81853733763696,-2.92076834020982,20.0334055357539));
#7293=CARTESIAN_POINT('Ctrl Pts',(5.8184998348711,-2.9207858289196,20.0334080986665));
#7294=CARTESIAN_POINT('Ctrl Pts',(5.81842439535529,-2.92082100695055,20.0334132541937));
#7295=CARTESIAN_POINT('Ctrl Pts',(5.81838645851186,-2.92083869629487,20.0334158468151));
#7296=CARTESIAN_POINT('Ctrl Pts',(5.81831014460997,-2.92087427843873,20.0334210621874));
#7297=CARTESIAN_POINT('Ctrl Pts',(5.81827176755886,-2.92089217121386,20.0334236849382));
#7298=CARTESIAN_POINT('Ctrl Pts',(5.81819456686792,-2.9209281631278,20.0334289610063));
#7299=CARTESIAN_POINT('Ctrl Pts',(5.81815574331681,-2.92094626220372,20.0334316143181));
#7300=CARTESIAN_POINT('Ctrl Pts',(5.81807764335683,-2.92098266957697,20.0334369519383));
#7301=CARTESIAN_POINT('Ctrl Pts',(5.81803836681591,-2.92100097791378,20.0334396362562));
#7302=CARTESIAN_POINT('Ctrl Pts',(5.81795935430806,-2.92103780680397,20.0334450363392));
#7303=CARTESIAN_POINT('Ctrl Pts',(5.81791961843136,-2.92105632729265,20.0334477520987));
#7304=CARTESIAN_POINT('Ctrl Pts',(5.81783968067501,-2.92109358348382,20.033453215516));
#7305=CARTESIAN_POINT('Ctrl Pts',(5.81779947873957,-2.92111231918905,20.0334559631782));
#7306=CARTESIAN_POINT('Ctrl Pts',(5.81771860215329,-2.92115000887153,20.0334614908616));
#7307=CARTESIAN_POINT('Ctrl Pts',(5.81767792752605,-2.92116896281392,20.0334642708817));
#7308=CARTESIAN_POINT('Ctrl Pts',(5.81759609871236,-2.92120709208799,20.0334698637504));
#7309=CARTESIAN_POINT('Ctrl Pts',(5.81755494454887,-2.92122626738448,20.0334726765981));
#7310=CARTESIAN_POINT('Ctrl Pts',(5.81747214977746,-2.92126484250105,20.0334783355943));
#7311=CARTESIAN_POINT('Ctrl Pts',(5.81743050912676,-2.92128424231595,20.0334811817464));
#7312=CARTESIAN_POINT('Ctrl Pts',(5.81734673432384,-2.92132326968141,20.0334869078358));
#7313=CARTESIAN_POINT('Ctrl Pts',(5.81730460018414,-2.92134289720036,20.0334897877729));
#7314=CARTESIAN_POINT('Ctrl Pts',(5.81721983123472,-2.92138238323556,20.0334955819242));
#7315=CARTESIAN_POINT('Ctrl Pts',(5.81717719642748,-2.92140224172418,20.033498496139));
#7316=CARTESIAN_POINT('Ctrl Pts',(5.81709141888581,-2.92144219299921,20.0335043593436));
#7317=CARTESIAN_POINT('Ctrl Pts',(5.81704827613498,-2.92146228576608,20.0335073083353));
#7318=CARTESIAN_POINT('Ctrl Pts',(5.81696147539766,-2.92150270891947,20.0335132415956));
#7319=CARTESIAN_POINT('Ctrl Pts',(5.81691781728047,-2.92152303933896,20.0335162258738));
#7320=CARTESIAN_POINT('Ctrl Pts',(5.81682997820801,-2.92156394125377,20.0335222302288));
#7321=CARTESIAN_POINT('Ctrl Pts',(5.81678579731698,-2.92158451269054,20.0335252503019));
#7322=CARTESIAN_POINT('Ctrl Pts',(5.81669690506214,-2.92162590010846,20.0335313267709));
#7323=CARTESIAN_POINT('Ctrl Pts',(5.81665219366934,-2.92164671607371,20.0335343831695));
#7324=CARTESIAN_POINT('Ctrl Pts',(5.81656649370655,-2.92168661240241,20.0335402415401));
#7325=CARTESIAN_POINT('Ctrl Pts',(5.8165255052001,-2.92170569293563,20.0335430435029));
#7326=CARTESIAN_POINT('Ctrl Pts',(5.80936120444545,-2.92504055853287,20.03403279767));
#7327=CARTESIAN_POINT('Ctrl Pts',(5.80222602422412,-2.92833017458233,20.0345213703911));
#7328=CARTESIAN_POINT('Ctrl Pts',(5.78589245937321,-2.93578832635036,20.0356415912259));
#7329=CARTESIAN_POINT('Ctrl Pts',(5.77668646957328,-2.93993973681065,20.0362742581863));
#7330=CARTESIAN_POINT('Ctrl Pts',(5.75211758274164,-2.95088032637994,20.0379658284221));
#7331=CARTESIAN_POINT('Ctrl Pts',(5.73672109396272,-2.95759268584033,20.0390291041189));
#7332=CARTESIAN_POINT('Ctrl Pts',(5.60174730892285,-3.01518539488075,20.0483739874767));
#7333=CARTESIAN_POINT('Ctrl Pts',(5.4792585254509,-3.05890494407524,20.0570116580039));
#7334=CARTESIAN_POINT('Ctrl Pts',(5.17519390166147,-3.14712598535538,20.0783182687046));
#7335=CARTESIAN_POINT('Ctrl Pts',(4.99171247775257,-3.18347130357153,20.0910440507683));
#7336=CARTESIAN_POINT('Ctrl Pts',(4.7154531055782,-3.21362131739292,20.1094728223012));
#7337=CARTESIAN_POINT('Ctrl Pts',(4.62440820435326,-3.21966357332375,20.1154355373931));
#7338=CARTESIAN_POINT('Ctrl Pts',(4.49321950416103,-3.22278887606631,20.1238537528369));
#7339=CARTESIAN_POINT('Ctrl Pts',(4.45320062382921,-3.22299678498016,20.1263988125576));
#7340=CARTESIAN_POINT('Ctrl Pts',(4.38139349742741,-3.22203231062258,20.1309252434993));
#7341=CARTESIAN_POINT('Ctrl Pts',(4.34960740189976,-3.22113477679159,20.1329147651224));
#7342=CARTESIAN_POINT('Ctrl Pts',(4.30101022805123,-3.21904237737638,20.1359357866314));
#7343=CARTESIAN_POINT('Ctrl Pts',(4.28418729247799,-3.21818586847259,20.1369777792007));
#7344=CARTESIAN_POINT('Ctrl Pts',(4.25359573460019,-3.21638778558901,20.1388659031364));
#7345=CARTESIAN_POINT('Ctrl Pts',(4.23982505984386,-3.21548959860791,20.1397133698728));
#7346=CARTESIAN_POINT('Ctrl Pts',(4.20981483239099,-3.21333852968221,20.1415550446753));
#7347=CARTESIAN_POINT('Ctrl Pts',(4.19357809131214,-3.21205092839857,20.1425481425902));
#7348=CARTESIAN_POINT('Ctrl Pts',(4.14908534781253,-3.20818294452152,20.1452607933752));
#7349=CARTESIAN_POINT('Ctrl Pts',(4.12085215251896,-3.20535238603411,20.1469724951313));
#7350=CARTESIAN_POINT('Ctrl Pts',(3.96445418755285,-3.18758334860892,20.1564064548065));
#7351=CARTESIAN_POINT('Ctrl Pts',(3.8372312947948,-3.16533037149005,20.1638947482334));
#7352=CARTESIAN_POINT('Ctrl Pts',(3.49661533133824,-3.08442180691213,20.1838253745984));
#7353=CARTESIAN_POINT('Ctrl Pts',(3.28739537265973,-3.01135137486931,20.1959120165873));
#7354=CARTESIAN_POINT('Ctrl Pts',(2.99186978768175,-2.87266090425585,20.2145409796746));
#7355=CARTESIAN_POINT('Ctrl Pts',(2.89869762689419,-2.82322070746324,20.2206735830858));
#7356=CARTESIAN_POINT('Ctrl Pts',(2.79326446088465,-2.76046499163195,20.2281133225626));
#7357=CARTESIAN_POINT('Ctrl Pts',(2.7784751074608,-2.75150009488225,20.2291688314202));
#7358=CARTESIAN_POINT('Ctrl Pts',(2.75584678180456,-2.73753314606053,20.230803361959));
#7359=CARTESIAN_POINT('Ctrl Pts',(2.74795585036782,-2.73261531606496,20.2313770493173));
#7360=CARTESIAN_POINT('Ctrl Pts',(2.73346046416206,-2.72349409198464,20.2324379317567));
#7361=CARTESIAN_POINT('Ctrl Pts',(2.72684994291019,-2.71930071811731,20.2329244729903));
#7362=CARTESIAN_POINT('Ctrl Pts',(2.71188965746375,-2.709734064192,20.2340317633046));
#7363=CARTESIAN_POINT('Ctrl Pts',(2.7035494538933,-2.70434628662569,20.2346534521706));
#7364=CARTESIAN_POINT('Ctrl Pts',(2.6819497674388,-2.6902509762051,20.2362746687025));
#7365=CARTESIAN_POINT('Ctrl Pts',(2.6687296200076,-2.68148404889672,20.2372779275445));
#7366=CARTESIAN_POINT('Ctrl Pts',(2.57900949322299,-2.62102785316734,20.2441590443347));
#7367=CARTESIAN_POINT('Ctrl Pts',(2.50470335423577,-2.56617395770382,20.2502183024655));
#7368=CARTESIAN_POINT('Ctrl Pts',(2.36860322579397,-2.45636936876508,20.2618715565205));
#7369=CARTESIAN_POINT('Ctrl Pts',(2.30636282134923,-2.40207754498297,20.2674431279201));
#7370=CARTESIAN_POINT('Ctrl Pts',(2.14978544891488,-2.25453025251069,20.2819928625193));
#7371=CARTESIAN_POINT('Ctrl Pts',(2.05899155860516,-2.1577304560453,20.2909715906244));
#7372=CARTESIAN_POINT('Ctrl Pts',(1.91192627110592,-1.98015592933211,20.3063083074358));
#7373=CARTESIAN_POINT('Ctrl Pts',(1.85290544149997,-1.90188718867303,20.3127323961146));
#7374=CARTESIAN_POINT('Ctrl Pts',(1.77381199807104,-1.78640181666568,20.3217269699739));
#7375=CARTESIAN_POINT('Ctrl Pts',(1.75076438177461,-1.75129746664236,20.3244011813034));
#7376=CARTESIAN_POINT('Ctrl Pts',(1.71082455016542,-1.68779276381244,20.329134128871));
#7377=CARTESIAN_POINT('Ctrl Pts',(1.69367095468105,-1.65956468570267,20.3312021313625));
#7378=CARTESIAN_POINT('Ctrl Pts',(1.66830039732782,-1.61633076657862,20.3343166353418));
#7379=CARTESIAN_POINT('Ctrl Pts',(1.65976434434846,-1.60151565374527,20.3353746560474));
#7380=CARTESIAN_POINT('Ctrl Pts',(1.64448238195334,-1.57449757419441,20.3372876979737));
#7381=CARTESIAN_POINT('Ctrl Pts',(1.63769703908918,-1.56231750673292,20.3381441215073));
#7382=CARTESIAN_POINT('Ctrl Pts',(1.62323351363649,-1.53595369522348,20.3399851467335));
#7383=CARTESIAN_POINT('Ctrl Pts',(1.61558230622519,-1.52175552614142,20.3409687705793));
#7384=CARTESIAN_POINT('Ctrl Pts',(1.59509423658253,-1.48304319123189,20.3436298541507));
#7385=CARTESIAN_POINT('Ctrl Pts',(1.58246581166175,-1.45841982528852,20.3452999569794));
#7386=CARTESIAN_POINT('Ctrl Pts',(1.51807178700059,-1.32877652926377,20.353980939165));
#7387=CARTESIAN_POINT('Ctrl Pts',(1.47173742439461,-1.22114985921871,20.3608017814509));
#7388=CARTESIAN_POINT('Ctrl Pts',(1.35217200510447,-0.895656203089265,20.3806244011082));
#7389=CARTESIAN_POINT('Ctrl Pts',(1.296257402794,-0.672247373377331,20.393168308898));
#7390=CARTESIAN_POINT('Ctrl Pts',(1.24940767471226,-0.336051254309889,20.4125051524799));
#7391=CARTESIAN_POINT('Ctrl Pts',(1.23982242172045,-0.226610598667985,20.418880058432));
#7392=CARTESIAN_POINT('Ctrl Pts',(1.23520751265689,-0.0994763455260606,
20.426592485967));
#7393=CARTESIAN_POINT('Ctrl Pts',(1.23471631830738,-0.0820410874345721,
20.4276568651638));
#7394=CARTESIAN_POINT('Ctrl Pts',(1.23417967116551,-0.0552756420812884,
20.4293022691181));
#7395=CARTESIAN_POINT('Ctrl Pts',(1.23403316091057,-0.0459475041239562,
20.4298778479594));
#7396=CARTESIAN_POINT('Ctrl Pts',(1.23383822938874,-0.0287931573369041,
20.4309404664841));
#7397=CARTESIAN_POINT('Ctrl Pts',(1.23377781117846,-0.0209672873408642,
20.431426836118));
#7398=CARTESIAN_POINT('Ctrl Pts',(1.23370557101281,-0.00325132210821304,
20.432531473411));
#7399=CARTESIAN_POINT('Ctrl Pts',(1.23371076933772,0.00663859296840534,
20.433150661333));
#7400=CARTESIAN_POINT('Ctrl Pts',(1.23384217768,0.0322609461688485,20.4347610960076));
#7401=CARTESIAN_POINT('Ctrl Pts',(1.23403807036731,0.0479925546045979,20.4357559949973));
#7402=CARTESIAN_POINT('Ctrl Pts',(1.23611316789384,0.152920866169307,20.442429938369));
#7403=CARTESIAN_POINT('Ctrl Pts',(1.24158030059646,0.24200026682429,20.4482784897219));
#7404=CARTESIAN_POINT('Ctrl Pts',(1.25939907103643,0.414716411022131,20.4598365065786));
#7405=CARTESIAN_POINT('Ctrl Pts',(1.27136083570037,0.49832808061199,20.4655324263059));
#7406=CARTESIAN_POINT('Ctrl Pts',(1.30367401373184,0.674513195164816,20.4776453424081));
#7407=CARTESIAN_POINT('Ctrl Pts',(1.32485419765819,0.76685964024731,20.484059683078));
#7408=CARTESIAN_POINT('Ctrl Pts',(1.39480270069939,1.02006747699278,20.501695061679));
#7409=CARTESIAN_POINT('Ctrl Pts',(1.45213240989311,1.17826759719335,20.5127533074032));
#7410=CARTESIAN_POINT('Ctrl Pts',(1.53819524297594,1.36799834712336,20.5259645828656));
#7411=CARTESIAN_POINT('Ctrl Pts',(1.5555313261051,1.40438671703225,20.5284970646515));
#7412=CARTESIAN_POINT('Ctrl Pts',(1.58181644870487,1.45699418154849,20.5321579301705));
#7413=CARTESIAN_POINT('Ctrl Pts',(1.59022937067149,1.47347539771574,20.5333047840139));
#7414=CARTESIAN_POINT('Ctrl Pts',(1.60529797065546,1.50237786852277,20.5353161771918));
#7415=CARTESIAN_POINT('Ctrl Pts',(1.61189397798415,1.51482951316069,20.536182784287));
#7416=CARTESIAN_POINT('Ctrl Pts',(1.62492858380067,1.53905028600817,20.5378687941861));
#7417=CARTESIAN_POINT('Ctrl Pts',(1.63135941257534,1.55082324601425,20.5386884494922));
#7418=CARTESIAN_POINT('Ctrl Pts',(1.64891372406711,1.5824884682818,20.5408936432014));
#7419=CARTESIAN_POINT('Ctrl Pts',(1.66017514654665,1.60230368785051,20.5422742340315));
#7420=CARTESIAN_POINT('Ctrl Pts',(1.70365329247344,1.67695170225576,20.5474794678214));
#7421=CARTESIAN_POINT('Ctrl Pts',(1.73728156691112,1.73094825153254,20.5512531149485));
#7422=CARTESIAN_POINT('Ctrl Pts',(1.95885876212814,2.06432086333692,20.5746927623689));
#7423=CARTESIAN_POINT('Ctrl Pts',(2.18798573699663,2.3137461611115,20.5926221221632));
#7424=CARTESIAN_POINT('Ctrl Pts',(2.48823381582663,2.55232515107536,20.6148909545366));
#7425=CARTESIAN_POINT('Ctrl Pts',(2.52555490973856,2.5806750602596,20.6176452888697));
#7426=CARTESIAN_POINT('Ctrl Pts',(2.588540489327,2.62638899941919,20.6222954793586));
#7427=CARTESIAN_POINT('Ctrl Pts',(2.61386186205316,2.64421536130786,20.6241654159564));
#7428=CARTESIAN_POINT('Ctrl Pts',(2.6491306161265,2.66829214229066,20.6267764707066));
#7429=CARTESIAN_POINT('Ctrl Pts',(2.6588620624634,2.67485780570083,20.6274975930849));
#7430=CARTESIAN_POINT('Ctrl Pts',(2.67536153894342,2.68585905714554,20.6287217683737));
#7431=CARTESIAN_POINT('Ctrl Pts',(2.68211091863217,2.69032266864342,20.6292229659869));
#7432=CARTESIAN_POINT('Ctrl Pts',(2.69506521365907,2.69881986428452,20.6301858891662));
#7433=CARTESIAN_POINT('Ctrl Pts',(2.70126731702476,2.70285756361273,20.6306473156675));
#7434=CARTESIAN_POINT('Ctrl Pts',(2.71614798101354,2.71247237146189,20.6317552853609));
#7435=CARTESIAN_POINT('Ctrl Pts',(2.72483945769178,2.71802920115407,20.6324031330788));
#7436=CARTESIAN_POINT('Ctrl Pts',(2.75629112064216,2.73792549743324,20.6347495969276));
#7437=CARTESIAN_POINT('Ctrl Pts',(2.77920324245831,2.75202113450313,20.6364629271834));
#7438=CARTESIAN_POINT('Ctrl Pts',(2.95354164134404,2.85628910374484,20.6495137254482));
#7439=CARTESIAN_POINT('Ctrl Pts',(3.11194687143989,2.93418249981422,20.6614345117631));
#7440=CARTESIAN_POINT('Ctrl Pts',(3.44210615082447,3.06416199695857,20.6854396598147));
#7441=CARTESIAN_POINT('Ctrl Pts',(3.6134741487632,3.11566895043166,20.697478531601));
#7442=CARTESIAN_POINT('Ctrl Pts',(3.8477529416144,3.16532507819361,20.7130876531449));
#7443=CARTESIAN_POINT('Ctrl Pts',(3.90761196640856,3.1762516946349,20.7170064603597));
#7444=CARTESIAN_POINT('Ctrl Pts',(4.01129732122736,3.19215927825279,20.723674691094));
#7445=CARTESIAN_POINT('Ctrl Pts',(4.05498102339162,3.19794721715642,20.7264479140934));
#7446=CARTESIAN_POINT('Ctrl Pts',(4.11782259031509,3.20496545558575,20.7303874057335));
#7447=CARTESIAN_POINT('Ctrl Pts',(4.13689262585017,3.20692312550297,20.731576335498));
#7448=CARTESIAN_POINT('Ctrl Pts',(4.1701109575492,3.21003396048734,20.7336362502505));
#7449=CARTESIAN_POINT('Ctrl Pts',(4.18425134964875,3.21126400659393,20.73450962429));
#7450=CARTESIAN_POINT('Ctrl Pts',(4.21337694933047,3.21360382356192,20.7363015460987));
#7451=CARTESIAN_POINT('Ctrl Pts',(4.22836273611425,3.21470229219921,20.7372197190299));
#7452=CARTESIAN_POINT('Ctrl Pts',(4.26666007168502,3.21724036473999,20.7395567500802));
#7453=CARTESIAN_POINT('Ctrl Pts',(4.28998083752481,3.21853145618465,20.7409709409398));
#7454=CARTESIAN_POINT('Ctrl Pts',(4.38108421032933,3.22258228036187,20.7464627472769));
#7455=CARTESIAN_POINT('Ctrl Pts',(4.4489357965181,3.22345523548394,20.7504816530738));
#7456=CARTESIAN_POINT('Ctrl Pts',(4.84827485961254,3.21598211746203,20.7738165118144));
#7457=CARTESIAN_POINT('Ctrl Pts',(5.17678795814548,3.15866346104973,20.7914900717375));
#7458=CARTESIAN_POINT('Ctrl Pts',(5.53495440649006,3.03729560693319,20.8134535400521));
#7459=CARTESIAN_POINT('Ctrl Pts',(5.57881788371412,3.02136193445235,20.8161965455119));
#7460=CARTESIAN_POINT('Ctrl Pts',(5.65109606151289,2.99331536852946,20.8208293857182));
#7461=CARTESIAN_POINT('Ctrl Pts',(5.67971126637191,2.98173588971379,20.8226935477415));
#7462=CARTESIAN_POINT('Ctrl Pts',(5.71895891253584,2.96519384252772,20.8252978185569));
#7463=CARTESIAN_POINT('Ctrl Pts',(5.7297381847252,2.96058117245109,20.8260180673548));
#7464=CARTESIAN_POINT('Ctrl Pts',(5.74791112929617,2.95268699595843,20.8272411930127));
#7465=CARTESIAN_POINT('Ctrl Pts',(5.75531818572171,2.94943622782203,20.8277422220125));
#7466=CARTESIAN_POINT('Ctrl Pts',(5.76948123786019,2.9431567271634,20.8287051744138));
#7467=CARTESIAN_POINT('Ctrl Pts',(5.7762391487376,2.94013254985871,20.8291668009553));
#7468=CARTESIAN_POINT('Ctrl Pts',(5.79239893157632,2.93283407811172,20.8302757185385));
#7469=CARTESIAN_POINT('Ctrl Pts',(5.8017907263311,2.92853785354625,20.8309243189601));
#7470=CARTESIAN_POINT('Ctrl Pts',(5.83564905679423,2.9128523062008,20.8332770583424));
#7471=CARTESIAN_POINT('Ctrl Pts',(5.85999217588149,2.90120126431552,20.8349960144749));
#7472=CARTESIAN_POINT('Ctrl Pts',(6.03284349692361,2.81578708472014,20.8473836888667));
#7473=CARTESIAN_POINT('Ctrl Pts',(6.1755968630441,2.73097097064393,20.8585693983261));
#7474=CARTESIAN_POINT('Ctrl Pts',(6.4377951656247,2.54645566370535,20.8802568993132));
#7475=CARTESIAN_POINT('Ctrl Pts',(6.55783681924014,2.44833609508093,20.890726944524));
#7476=CARTESIAN_POINT('Ctrl Pts',(6.75889532256174,2.25827201167407,20.9089762780794));
#7477=CARTESIAN_POINT('Ctrl Pts',(6.84261675183808,2.16962312873576,20.9168419363039));
#7478=CARTESIAN_POINT('Ctrl Pts',(6.93867446349931,2.05560598473064,20.9262046031921));
#7479=CARTESIAN_POINT('Ctrl Pts',(6.95595886930006,2.03455410289331,20.9279042989028));
#7480=CARTESIAN_POINT('Ctrl Pts',(6.98289058999791,2.00089079943567,20.9305774483291));
#7481=CARTESIAN_POINT('Ctrl Pts',(6.9927148628753,1.98842323995954,20.9315579725511));
#7482=CARTESIAN_POINT('Ctrl Pts',(7.01101018345009,1.96484923916137,20.9333944162909));
#7483=CARTESIAN_POINT('Ctrl Pts',(7.01950188144625,1.95375936356498,20.9342511416336));
#7484=CARTESIAN_POINT('Ctrl Pts',(7.03843922835544,1.92869186672666,20.9361717855173));
#7485=CARTESIAN_POINT('Ctrl Pts',(7.04884404664413,1.91468384211724,20.9372340908805));
#7486=CARTESIAN_POINT('Ctrl Pts',(7.07517470949746,1.87862669825667,20.939941097252));
#7487=CARTESIAN_POINT('Ctrl Pts',(7.0909363261925,1.85645895271271,20.9415794765655));
#7488=CARTESIAN_POINT('Ctrl Pts',(7.20050333873654,1.69815366806227,20.9531043423383));
#7489=CARTESIAN_POINT('Ctrl Pts',(7.28399717572356,1.55516711557353,20.9625898658224));
#7490=CARTESIAN_POINT('Ctrl Pts',(7.44818744653167,1.21664002217988,20.9837964926371));
#7491=CARTESIAN_POINT('Ctrl Pts',(7.52136408678864,1.01833134794205,20.99535411982));
#7492=CARTESIAN_POINT('Ctrl Pts',(7.5945379959547,0.738132985891712,21.0120888477955));
#7493=CARTESIAN_POINT('Ctrl Pts',(7.61163223008169,0.661256504066419,21.0167242860153));
#7494=CARTESIAN_POINT('Ctrl Pts',(7.62881137678469,0.567997817193637,21.0224832725238));
#7495=CARTESIAN_POINT('Ctrl Pts',(7.63161050260384,0.552135934576607,21.023467481253));
#7496=CARTESIAN_POINT('Ctrl Pts',(7.63579522938433,0.527337403274637,21.0250144523421));
#7497=CARTESIAN_POINT('Ctrl Pts',(7.63726235790212,0.518414524973121,21.0255727398601));
#7498=CARTESIAN_POINT('Ctrl Pts',(7.63993442073019,0.501724951712649,21.0266202822847));
#7499=CARTESIAN_POINT('Ctrl Pts',(7.64114851379147,0.493959919459706,21.0271090186155));
#7500=CARTESIAN_POINT('Ctrl Pts',(7.64386097654276,0.476185941869878,21.028230772511));
#7501=CARTESIAN_POINT('Ctrl Pts',(7.64534061062872,0.466174332302416,21.0288648193733));
#7502=CARTESIAN_POINT('Ctrl Pts',(7.64916093146459,0.439455441262774,21.0305625005589));
#7503=CARTESIAN_POINT('Ctrl Pts',(7.65141758979928,0.422736720527652,21.031630555888));
#7504=CARTESIAN_POINT('Ctrl Pts',(7.67054209998754,0.272140053014318,21.041298477021));
#7505=CARTESIAN_POINT('Ctrl Pts',(7.67911557658673,0.137357291392169,21.0502816467442));
#7506=CARTESIAN_POINT('Ctrl Pts',(7.67921879563721,0.00163395566385627,
21.0594235963388));
#7507=CARTESIAN_POINT('Ctrl Pts',(7.67921910621823,0.000816976217060092,
21.0594786294844));
#7508=CARTESIAN_POINT('Ctrl Pts',(7.67921910621823,2.36916961325777E-11,
21.0595336661193));
#7509=CARTESIAN_POINT('Ctrl Pts',(7.67921910621823,-1.24760202169227E-10,
20.8155686056964));
#7510=CARTESIAN_POINT('Ctrl Pts',(7.6792191062261,0.203257940460228,20.80189032375));
#7511=CARTESIAN_POINT('Ctrl Pts',(7.65998935550836,0.406090050604238,20.7880266178191));
#7512=CARTESIAN_POINT('Ctrl Pts',(7.59870376082183,0.726321729020061,20.7665139614357));
#7513=CARTESIAN_POINT('Ctrl Pts',(7.56876354080615,0.845465263401139,20.7585874627029));
#7514=CARTESIAN_POINT('Ctrl Pts',(7.523943767758,0.988666502017597,20.7491638285754));
#7515=CARTESIAN_POINT('Ctrl Pts',(7.51546199988171,1.01460573698085,20.7474608135917));
#7516=CARTESIAN_POINT('Ctrl Pts',(7.50152389680916,1.05546726803852,20.7447837277565));
#7517=CARTESIAN_POINT('Ctrl Pts',(7.4962850938062,1.07046186650283,20.7438025499587));
#7518=CARTESIAN_POINT('Ctrl Pts',(7.48623244264119,1.09856574117376,20.741965631895));
#7519=CARTESIAN_POINT('Ctrl Pts',(7.48144384267872,1.11168359522666,20.7411090798109));
#7520=CARTESIAN_POINT('Ctrl Pts',(7.47048712685998,1.14110328617626,20.7391897985364));
#7521=CARTESIAN_POINT('Ctrl Pts',(7.46427169298736,1.15738712454581,20.7381286737232));
#7522=CARTESIAN_POINT('Ctrl Pts',(7.44804219250174,1.19889299521616,20.7354265473123));
#7523=CARTESIAN_POINT('Ctrl Pts',(7.4378409880456,1.22404073238074,20.7337918288744));
#7524=CARTESIAN_POINT('Ctrl Pts',(7.36412608603623,1.39936994107175,20.7224057437365));
#7525=CARTESIAN_POINT('Ctrl Pts',(7.28960895896023,1.54467912888601,20.7130435841599));
#7526=CARTESIAN_POINT('Ctrl Pts',(7.15253708840796,1.76838638007053,20.6982482621205));
#7527=CARTESIAN_POINT('Ctrl Pts',(7.09678668209508,1.85059352979628,20.6927150567814));
#7528=CARTESIAN_POINT('Ctrl Pts',(6.95800088501966,2.03617332615649,20.6797461891262));
#7529=CARTESIAN_POINT('Ctrl Pts',(6.87221246868468,2.13725102567721,20.6723066282859));
#7530=CARTESIAN_POINT('Ctrl Pts',(6.75170724713302,2.26268013789008,20.6621570477182));
#7531=CARTESIAN_POINT('Ctrl Pts',(6.72238397565363,2.29204472459433,20.6597079433507));
#7532=CARTESIAN_POINT('Ctrl Pts',(6.67236566993344,2.34023544503516,20.6555473006361));
#7533=CARTESIAN_POINT('Ctrl Pts',(6.65197712163546,2.35937363585616,20.6538558339527));
#7534=CARTESIAN_POINT('Ctrl Pts',(6.62316937748986,2.38571795762875,20.6514677209536));
#7535=CARTESIAN_POINT('Ctrl Pts',(6.61495749831553,2.39315024428694,20.6507871724835));
#7536=CARTESIAN_POINT('Ctrl Pts',(6.600678099961,2.40594074688318,20.6496037966797));
#7537=CARTESIAN_POINT('Ctrl Pts',(6.5946283121756,2.41131878741107,20.6491024351465));
#7538=CARTESIAN_POINT('Ctrl Pts',(6.58301236934597,2.42156685042413,20.6481396556417));
#7539=CARTESIAN_POINT('Ctrl Pts',(6.5774496164347,2.4264405893615,20.6476785395253));
#7540=CARTESIAN_POINT('Ctrl Pts',(6.56409996640319,2.43805574235876,20.6465719239631));
#7541=CARTESIAN_POINT('Ctrl Pts',(6.55629748751088,2.44477901005511,20.6459251265765));
#7542=CARTESIAN_POINT('Ctrl Pts',(6.52808644334703,2.46885332545938,20.6435869123943));
#7543=CARTESIAN_POINT('Ctrl Pts',(6.5074945945319,2.48598661945031,20.6418809145935));
#7544=CARTESIAN_POINT('Ctrl Pts',(6.34453104947261,2.61817631557478,20.628401220226));
#7545=CARTESIAN_POINT('Ctrl Pts',(6.19281620159547,2.72116002521634,20.615998648016));
#7546=CARTESIAN_POINT('Ctrl Pts',(5.88174862151484,2.89566070739654,20.5918700573903));
#7547=CARTESIAN_POINT('Ctrl Pts',(5.72366501311888,2.96824847082924,20.5801823209653));
#7548=CARTESIAN_POINT('Ctrl Pts',(5.47551235773078,3.05873329744433,20.5629773745373));
#7549=CARTESIAN_POINT('Ctrl Pts',(5.38926380573703,3.08612948045021,20.5571903115747));
#7550=CARTESIAN_POINT('Ctrl Pts',(5.27790731466135,3.11640475872218,20.5499578868994));
#7551=CARTESIAN_POINT('Ctrl Pts',(5.25376945080736,3.12266738016391,20.5484041296313));
#7552=CARTESIAN_POINT('Ctrl Pts',(5.21464094984338,3.13233606290279,20.5459073727343));
#7553=CARTESIAN_POINT('Ctrl Pts',(5.19969474289645,3.13591604184041,20.5449588083495));
#7554=CARTESIAN_POINT('Ctrl Pts',(5.17102179811783,3.14256739720128,20.5431487066705));
#7555=CARTESIAN_POINT('Ctrl Pts',(5.15729947838207,3.14565608336492,20.5422866323182));
#7556=CARTESIAN_POINT('Ctrl Pts',(5.12594556248534,3.1524980216798,20.5403262652642));
#7557=CARTESIAN_POINT('Ctrl Pts',(5.10830171704411,3.15619339872267,20.5392298431364));
#7558=CARTESIAN_POINT('Ctrl Pts',(5.05260318548244,3.16737206698251,20.5357891321195));
#7559=CARTESIAN_POINT('Ctrl Pts',(5.01444304553417,3.17431676563756,20.5334619398997));
#7560=CARTESIAN_POINT('Ctrl Pts',(4.71393741233468,3.22341854804529,20.5153498105479));
#7561=CARTESIAN_POINT('Ctrl Pts',(4.44742107592595,3.23367423882385,20.5006737179238));
#7562=CARTESIAN_POINT('Ctrl Pts',(4.06353980416161,3.20093963814636,20.4790725630545));
#7563=CARTESIAN_POINT('Ctrl Pts',(3.94509511252665,3.184164019046,20.4723235635139));
#7564=CARTESIAN_POINT('Ctrl Pts',(3.78954398774724,3.15322930830187,20.4630472432282));
#7565=CARTESIAN_POINT('Ctrl Pts',(3.7513658642522,3.1449122936069,20.4607366398938));
#7566=CARTESIAN_POINT('Ctrl Pts',(3.68704564691588,3.12967025138595,20.4567720802185));
#7567=CARTESIAN_POINT('Ctrl Pts',(3.66082164240132,3.1231063616649,20.4551352820614));
#7568=CARTESIAN_POINT('Ctrl Pts',(3.62392674084557,3.11337671115039,20.4527995567347));
#7569=CARTESIAN_POINT('Ctrl Pts',(3.61318412502423,3.11048416933536,20.4521155077195));
#7570=CARTESIAN_POINT('Ctrl Pts',(3.59476433537833,3.105422047809,20.4509354558885));
#7571=CARTESIAN_POINT('Ctrl Pts',(3.58707973035685,3.10327944587264,20.4504409990242));
#7572=CARTESIAN_POINT('Ctrl Pts',(3.57213506253294,3.09905274435522,20.4494750962023));
#7573=CARTESIAN_POINT('Ctrl Pts',(3.56487430613983,3.09697163739382,20.4490038487882));
#7574=CARTESIAN_POINT('Ctrl Pts',(3.54500772836103,3.09120174594519,20.4477091675299));
#7575=CARTESIAN_POINT('Ctrl Pts',(3.53241720034677,3.08746143924772,20.4468828292859));
#7576=CARTESIAN_POINT('Ctrl Pts',(3.48346842136487,3.07259385096927,20.4436484500621));
#7577=CARTESIAN_POINT('Ctrl Pts',(3.44728692398579,3.06090090251647,20.4412107480804));
#7578=CARTESIAN_POINT('Ctrl Pts',(3.20529514745477,2.97793848262771,20.4246280459604));
#7579=CARTESIAN_POINT('Ctrl Pts',(3.00697034113911,2.88660677169174,20.4097130586563));
#7580=CARTESIAN_POINT('Ctrl Pts',(2.70060084843092,2.70593053389447,20.3857514398787));
#7581=CARTESIAN_POINT('Ctrl Pts',(2.58642818491596,2.62832404664212,20.3765728759691));
#7582=CARTESIAN_POINT('Ctrl Pts',(2.41540983311767,2.49527492241208,20.3625349108826));
#7583=CARTESIAN_POINT('Ctrl Pts',(2.35504024960806,2.44465097302806,20.3575144372955));
#7584=CARTESIAN_POINT('Ctrl Pts',(2.27890749228751,2.37590195233017,20.3510920914764));
#7585=CARTESIAN_POINT('Ctrl Pts',(2.26141027714564,2.35974605738787,20.3496093961948));
#7586=CARTESIAN_POINT('Ctrl Pts',(2.23309616264653,2.333015012279,20.3471985648858));
#7587=CARTESIAN_POINT('Ctrl Pts',(2.22217203866494,2.32255525662752,20.3462655463012));
#7588=CARTESIAN_POINT('Ctrl Pts',(2.20117150344368,2.30216212912379,20.3444661209253));
#7589=CARTESIAN_POINT('Ctrl Pts',(2.19108610178463,2.29223855633506,20.3435993197227));
#7590=CARTESIAN_POINT('Ctrl Pts',(2.1679136661994,2.26913562952003,20.3416013858849));
#7591=CARTESIAN_POINT('Ctrl Pts',(2.15487447642931,2.25590883895909,20.3404723804837));
#7592=CARTESIAN_POINT('Ctrl Pts',(2.11285165171629,2.21253778197229,20.3368173930513));
#7593=CARTESIAN_POINT('Ctrl Pts',(2.08433949533688,2.18194123681857,20.3343117528587));
#7594=CARTESIAN_POINT('Ctrl Pts',(1.92298277105438,2.00188593293669,20.3199596174104));
#7595=CARTESIAN_POINT('Ctrl Pts',(1.80367825308385,1.84087302224888,20.3086884487533));
#7596=CARTESIAN_POINT('Ctrl Pts',(1.59027512033337,1.48860411157131,20.2856448669569));
#7597=CARTESIAN_POINT('Ctrl Pts',(1.49864568288021,1.29702278404258,20.2739297414775));
#7598=CARTESIAN_POINT('Ctrl Pts',(1.41528918661982,1.06696876460386,20.2593346217264));
#7599=CARTESIAN_POINT('Ctrl Pts',(1.40456724890996,1.03590178631152,20.2573525153534));
#7600=CARTESIAN_POINT('Ctrl Pts',(1.39057778088595,0.993263436025819,20.2546100502707));
#7601=CARTESIAN_POINT('Ctrl Pts',(1.38689673438307,0.981828557120877,20.2538724164229));
#7602=CARTESIAN_POINT('Ctrl Pts',(1.38082694378758,0.962605428850905,20.2526283610638));
#7603=CARTESIAN_POINT('Ctrl Pts',(1.37840360118651,0.95482808261079,20.2521239370618));
#7604=CARTESIAN_POINT('Ctrl Pts',(1.37385129024226,0.940020700127089,20.2511613218751));
#7605=CARTESIAN_POINT('Ctrl Pts',(1.37171682348752,0.932992426373027,20.2507034701408));
#7606=CARTESIAN_POINT('Ctrl Pts',(1.3667033594522,0.916279042268058,20.2496125382579));
#7607=CARTESIAN_POINT('Ctrl Pts',(1.36384586601288,0.906587635549567,20.2489782401659));
#7608=CARTESIAN_POINT('Ctrl Pts',(1.35391925631181,0.872327679480057,20.2467303040314));
#7609=CARTESIAN_POINT('Ctrl Pts',(1.34709717001337,0.847689341173257,20.2451034746778));
#7610=CARTESIAN_POINT('Ctrl Pts',(1.28648369248787,0.618197672365597,20.2298725880862));
#7611=CARTESIAN_POINT('Ctrl Pts',(1.25272076689596,0.408605982979522,20.2154244926738));
#7612=CARTESIAN_POINT('Ctrl Pts',(1.23033864421164,0.0435797743187418,20.1907206631199));
#7613=CARTESIAN_POINT('Ctrl Pts',(1.23193806497929,-0.110569175730084,20.1804204087835));
#7614=CARTESIAN_POINT('Ctrl Pts',(1.25145946029103,-0.348049065600556,20.1649425440327));
#7615=CARTESIAN_POINT('Ctrl Pts',(1.26166099667973,-0.431773357404261,20.1595587545492));
#7616=CARTESIAN_POINT('Ctrl Pts',(1.27902942970534,-0.539062577063086,20.1527505866144));
#7617=CARTESIAN_POINT('Ctrl Pts',(1.28319630573297,-0.563072949058847,20.1512328028228));
#7618=CARTESIAN_POINT('Ctrl Pts',(1.29041203669186,-0.602023744971367,20.1487795490925));
#7619=CARTESIAN_POINT('Ctrl Pts',(1.29329522837953,-0.616993507509841,20.1478388638717));
#7620=CARTESIAN_POINT('Ctrl Pts',(1.29905018209044,-0.645772576752312,20.146034389472));
#7621=CARTESIAN_POINT('Ctrl Pts',(1.30190658538588,-0.659584562787673,20.1451701342649));
#7622=CARTESIAN_POINT('Ctrl Pts',(1.30867510920621,-0.691263351746486,20.1431917593684));
#7623=CARTESIAN_POINT('Ctrl Pts',(1.31264886001595,-0.709116598340052,20.1420796335322));
#7624=CARTESIAN_POINT('Ctrl Pts',(1.32584814273356,-0.76612540676154,20.1385367285437));
#7625=CARTESIAN_POINT('Ctrl Pts',(1.33565509216899,-0.805143379692991,20.1361245567497));
#7626=CARTESIAN_POINT('Ctrl Pts',(1.41168727026304,-1.08534479382796,20.1188715974321));
#7627=CARTESIAN_POINT('Ctrl Pts',(1.50505740756165,-1.31827664298623,20.1049915521263));
#7628=CARTESIAN_POINT('Ctrl Pts',(1.68630305642329,-1.65199931205563,20.0837317363204));
#7629=CARTESIAN_POINT('Ctrl Pts',(1.75498278903876,-1.76206936643015,20.0764430315668));
#7630=CARTESIAN_POINT('Ctrl Pts',(1.85384761567692,-1.90109400940692,20.0664836399689));
#7631=CARTESIAN_POINT('Ctrl Pts',(1.87823172031496,-1.93403431536836,20.0640639190838));
#7632=CARTESIAN_POINT('Ctrl Pts',(1.92033470756023,-1.9886993444595,20.0599295794272));
#7633=CARTESIAN_POINT('Ctrl Pts',(1.93772142845937,-2.01067470902559,20.0582341012643));
#7634=CARTESIAN_POINT('Ctrl Pts',(1.96250895929181,-2.04117802014961,20.0558288074632));
#7635=CARTESIAN_POINT('Ctrl Pts',(1.96967194866709,-2.04989873231762,20.0551350880543));
#7636=CARTESIAN_POINT('Ctrl Pts',(1.98199428400089,-2.06474114823008,20.0539436394842));
#7637=CARTESIAN_POINT('Ctrl Pts',(1.98713099088256,-2.07088167840589,20.0534475359148));
#7638=CARTESIAN_POINT('Ctrl Pts',(1.99712953798906,-2.08274406169786,20.0524828396211));
#7639=CARTESIAN_POINT('Ctrl Pts',(2.00198854631444,-2.08846812681644,20.0520144732105));
#7640=CARTESIAN_POINT('Ctrl Pts',(2.01525484993465,-2.1039860075396,20.0507370561269));
#7641=CARTESIAN_POINT('Ctrl Pts',(2.0237009456924,-2.1137462546264,20.0499252291492));
#7642=CARTESIAN_POINT('Ctrl Pts',(2.0561805337055,-2.15082689871259,20.0468097258168));
#7643=CARTESIAN_POINT('Ctrl Pts',(2.08061648811493,-2.17778916729506,20.0444790059511));
#7644=CARTESIAN_POINT('Ctrl Pts',(2.28207448279141,-2.39264851399055,20.0254098062097));
#7645=CARTESIAN_POINT('Ctrl Pts',(2.48062649945428,-2.55906294482358,20.0075953142518));
#7646=CARTESIAN_POINT('Ctrl Pts',(2.82526077354712,-2.78365780893886,19.9800813837387));
#7647=CARTESIAN_POINT('Ctrl Pts',(2.95943637791279,-2.85805805322755,19.9700408879759));
#7648=CARTESIAN_POINT('Ctrl Pts',(3.13334299989975,-2.938866839654,19.9578952435934));
#7649=CARTESIAN_POINT('Ctrl Pts',(3.1685609613684,-2.95447014054449,19.9554770547485));
#7650=CARTESIAN_POINT('Ctrl Pts',(3.22079471556389,-2.97650072554189,19.9519496106603));
#7651=CARTESIAN_POINT('Ctrl Pts',(3.23759768930003,-2.98342089882741,19.9508237339326));
#7652=CARTESIAN_POINT('Ctrl Pts',(3.26748930596217,-2.99543683543929,19.9488362390606));
#7653=CARTESIAN_POINT('Ctrl Pts',(3.28055429751014,-3.00058980420504,19.9479727107522));
#7654=CARTESIAN_POINT('Ctrl Pts',(3.30805952469041,-3.01123091393206,19.9461653946557));
#7655=CARTESIAN_POINT('Ctrl Pts',(3.3225064062497,-3.01670097823114,19.945222230232));
#7656=CARTESIAN_POINT('Ctrl Pts',(3.36071279427442,-3.03085392928518,19.9427436623629));
#7657=CARTESIAN_POINT('Ctrl Pts',(3.38453645659788,-3.03936142735575,19.9412141079569));
#7658=CARTESIAN_POINT('Ctrl Pts',(3.48844873359562,-3.07509499564038,19.9346087210251));
#7659=CARTESIAN_POINT('Ctrl Pts',(3.56949541547581,-3.0994438445374,19.9296274781268));
#7660=CARTESIAN_POINT('Ctrl Pts',(3.87510280463767,-3.17828549753513,19.9113407801115));
#7661=CARTESIAN_POINT('Ctrl Pts',(4.10434396128122,-3.21177452756352,19.8986562972658));
#7662=CARTESIAN_POINT('Ctrl Pts',(4.47971555154625,-3.22590940141942,19.8774889338543));
#7663=CARTESIAN_POINT('Ctrl Pts',(4.62441592132182,-3.22161685842743,19.8692162974869));
#7664=CARTESIAN_POINT('Ctrl Pts',(4.78651243498082,-3.20585762362093,19.8593535461784));
#7665=CARTESIAN_POINT('Ctrl Pts',(4.80469026986745,-3.20393409536691,19.8582389634646));
#7666=CARTESIAN_POINT('Ctrl Pts',(4.83229288190581,-3.20077559077427,19.8565321505794));
#7667=CARTESIAN_POINT('Ctrl Pts',(4.84173052562481,-3.19965334469102,19.8559460178015));
#7668=CARTESIAN_POINT('Ctrl Pts',(4.85892194073672,-3.19753192283268,19.8548734480458));
#7669=CARTESIAN_POINT('Ctrl Pts',(4.86667717562877,-3.1965462640085,19.8543877706623));
#7670=CARTESIAN_POINT('Ctrl Pts',(4.88403362947328,-3.19427612642629,19.853296703348));
#7671=CARTESIAN_POINT('Ctrl Pts',(4.89363259764473,-3.19297658454093,19.8526904947386));
#7672=CARTESIAN_POINT('Ctrl Pts',(4.92162264998712,-3.18905861237541,19.8509149535667));
#7673=CARTESIAN_POINT('Ctrl Pts',(4.93999677737464,-3.18632446650533,19.8497394688616));
#7674=CARTESIAN_POINT('Ctrl Pts',(5.1085324262356,-3.15975436535562,19.8388724412056));
#7675=CARTESIAN_POINT('Ctrl Pts',(5.25683910587114,-3.12548102727469,19.8286976206247));
#7676=CARTESIAN_POINT('Ctrl Pts',(5.43373017371002,-3.07118370025185,19.8162044147342));
#7677=CARTESIAN_POINT('Ctrl Pts',(5.46515468487823,-3.06100668064633,19.8139704444758));
#7678=CARTESIAN_POINT('Ctrl Pts',(5.64130152808877,-3.00095336228902,19.8013802254744));
#7679=CARTESIAN_POINT('Ctrl Pts',(5.78249319775757,-2.94129489771561,19.7910411925474));
#7680=CARTESIAN_POINT('Ctrl Pts',(6.02393773082323,-2.81834155729616,19.7731953955648));
#7681=CARTESIAN_POINT('Ctrl Pts',(6.12595464539173,-2.75913585088555,19.7655945915664));
#7682=CARTESIAN_POINT('Ctrl Pts',(6.24707572910493,-2.6796593074015,19.756498768043));
#7683=CARTESIAN_POINT('Ctrl Pts',(6.26945597515771,-2.6645684014369,19.7548146595061));
#7684=CARTESIAN_POINT('Ctrl Pts',(6.30464751193567,-2.64019021200097,19.7521603860266));
#7685=CARTESIAN_POINT('Ctrl Pts',(6.31758415818323,-2.63108695266961,19.7511833177971));
#7686=CARTESIAN_POINT('Ctrl Pts',(6.34182106850008,-2.61376371900126,19.7493500314472));
#7687=CARTESIAN_POINT('Ctrl Pts',(6.35313587150298,-2.60556481240337,19.7484930348424));
#7688=CARTESIAN_POINT('Ctrl Pts',(6.37852230530873,-2.58691635862701,19.7465674512095));
#7689=CARTESIAN_POINT('Ctrl Pts',(6.39256280608908,-2.57642503303667,19.7455005146797));
#7690=CARTESIAN_POINT('Ctrl Pts',(6.42837835861238,-2.54920486003063,19.7427733380155));
#7691=CARTESIAN_POINT('Ctrl Pts',(6.45002673253861,-2.53231111412581,19.7411195851715));
#7692=CARTESIAN_POINT('Ctrl Pts',(6.6297510256859,-2.38832630670371,19.7273372753132));
#7693=CARTESIAN_POINT('Ctrl Pts',(6.77572779417187,-2.24684466245014,19.7158352373193));
#7694=CARTESIAN_POINT('Ctrl Pts',(7.05407028301371,-1.92082684355086,19.6918202814469));
#7695=CARTESIAN_POINT('Ctrl Pts',(7.18221625672768,-1.73418107325598,19.679400318638));
#7696=CARTESIAN_POINT('Ctrl Pts',(7.30585583971991,-1.50607079426406,19.6639357204327));
#7697=CARTESIAN_POINT('Ctrl Pts',(7.32145310892779,-1.47618442407018,19.6619036633946));
#7698=CARTESIAN_POINT('Ctrl Pts',(7.34202125897629,-1.43521897247623,19.6591028451176));
#7699=CARTESIAN_POINT('Ctrl Pts',(7.34740315719715,-1.42434722846931,19.6583580796775));
#7700=CARTESIAN_POINT('Ctrl Pts',(7.35630692692184,-1.40610274672691,19.6571053784026));
#7701=CARTESIAN_POINT('Ctrl Pts',(7.35986243244629,-1.3987464070686,19.6565995022249));
#7702=CARTESIAN_POINT('Ctrl Pts',(7.36655200965819,-1.38477027029404,19.6556367839711));
#7703=CARTESIAN_POINT('Ctrl Pts',(7.36969156103243,-1.37815316007054,19.6551802979656));
#7704=CARTESIAN_POINT('Ctrl Pts',(7.37707287882182,-1.36245791558826,19.6540960455252));
#7705=CARTESIAN_POINT('Ctrl Pts',(7.38129488731788,-1.35337064851568,19.6534670950788));
#7706=CARTESIAN_POINT('Ctrl Pts',(7.39603633287587,-1.32125063906304,19.6512402017276));
#7707=CARTESIAN_POINT('Ctrl Pts',(7.40632631602469,-1.29811443285608,19.6496293072818));
#7708=CARTESIAN_POINT('Ctrl Pts',(7.50289398300163,-1.07391099812518,19.6339697595508));
#7709=CARTESIAN_POINT('Ctrl Pts',(7.56875016578579,-0.864686239394832,19.619020285394));
#7710=CARTESIAN_POINT('Ctrl Pts',(7.65691843364384,-0.436815108652667,19.5895292030837));
#7711=CARTESIAN_POINT('Ctrl Pts',(7.67914521343245,-0.219257380582916,19.5750715637153));
#7712=CARTESIAN_POINT('Ctrl Pts',(7.6792190449084,-0.000725876579082373,
19.5612958883318));
#7713=CARTESIAN_POINT('Ctrl Pts',(7.67921910621823,-0.000362938246920867,
19.561273011506));
#7714=CARTESIAN_POINT('Ctrl Pts',(7.67921910621823,-6.1812332959659E-13,
19.5612501365773));
#7715=CARTESIAN_POINT('Origin',(4.45646910621825,-5.13094777615093E-16,
-2.31077344927308));
#7716=CARTESIAN_POINT('',(7.67921910621823,-1.45987529487438E-10,18.3139723139554));
#7717=CARTESIAN_POINT('',(7.67921897520325,-0.000918943817116763,18.5636187829496));
#7718=CARTESIAN_POINT('',(7.67921910621823,-3.51191647465084E-13,-2.31077344927308));
#7719=CARTESIAN_POINT('Ctrl Pts',(7.67921897520336,-0.000918943050560485,
18.563618782904));
#7720=CARTESIAN_POINT('Ctrl Pts',(7.67917356350457,-0.160178590564636,18.5730889559059));
#7721=CARTESIAN_POINT('Ctrl Pts',(7.66732338519769,-0.319224689801024,18.582188712083));
#7722=CARTESIAN_POINT('Ctrl Pts',(7.61684168702354,-0.656712027958172,18.601389853412));
#7723=CARTESIAN_POINT('Ctrl Pts',(7.57473373595707,-0.834053580990784,18.6114133596575));
#7724=CARTESIAN_POINT('Ctrl Pts',(7.5073910412776,-1.03880805762323,18.6237545995969));
#7725=CARTESIAN_POINT('Ctrl Pts',(7.49639354296673,-1.07056346511797,18.6256919062879));
#7726=CARTESIAN_POINT('Ctrl Pts',(7.46242930077096,-1.16388954087417,18.6314701367851));
#7727=CARTESIAN_POINT('Ctrl Pts',(7.438075150811,-1.22493250391884,18.6353596962907));
#7728=CARTESIAN_POINT('Ctrl Pts',(7.40557325509175,-1.2996737858473,18.6403102253246));
#7729=CARTESIAN_POINT('Ctrl Pts',(7.39916576821595,-1.31411702777398,18.6412757729855));
#7730=CARTESIAN_POINT('Ctrl Pts',(7.38891397262255,-1.33677481829658,18.642805404894));
#7731=CARTESIAN_POINT('Ctrl Pts',(7.38514065592759,-1.34502147140448,18.6433652739932));
#7732=CARTESIAN_POINT('Ctrl Pts',(7.37836486266749,-1.35966639418101,18.6443653057261));
#7733=CARTESIAN_POINT('Ctrl Pts',(7.37537608714793,-1.36607084314315,18.6448046251953));
#7734=CARTESIAN_POINT('Ctrl Pts',(7.36818336454741,-1.38135227718971,18.64585761081));
#7735=CARTESIAN_POINT('Ctrl Pts',(7.36395991403987,-1.3902198503516,18.6464724634038));
#7736=CARTESIAN_POINT('Ctrl Pts',(7.35108385516542,-1.41693915595175,18.6483363587531));
#7737=CARTESIAN_POINT('Ctrl Pts',(7.34230706769252,-1.43473005502303,18.6495926589333));
#7738=CARTESIAN_POINT('Ctrl Pts',(7.32159332733969,-1.47575852029142,18.6525233890286));
#7739=CARTESIAN_POINT('Ctrl Pts',(7.30953707559525,-1.49893398206685,18.6542040508736));
#7740=CARTESIAN_POINT('Ctrl Pts',(7.17184995981142,-1.75592646754528,18.6731031286075));
#7741=CARTESIAN_POINT('Ctrl Pts',(7.01807954662349,-1.97350568006721,18.6914450774901));
#7742=CARTESIAN_POINT('Ctrl Pts',(6.73319137800491,-2.28637827532187,18.7196838462234));
#7743=CARTESIAN_POINT('Ctrl Pts',(6.61858264811044,-2.39505068158381,18.7299725698775));
#7744=CARTESIAN_POINT('Ctrl Pts',(6.47557964101822,-2.51197883283734,18.7415989456958));
#7745=CARTESIAN_POINT('Ctrl Pts',(6.45448577515163,-2.52878913120045,18.7432859974226));
#7746=CARTESIAN_POINT('Ctrl Pts',(6.41945606182192,-2.55599331767073,18.7460427883805));
#7747=CARTESIAN_POINT('Ctrl Pts',(6.40564306879896,-2.56654252066682,18.7471186480954));
#7748=CARTESIAN_POINT('Ctrl Pts',(6.38058119887818,-2.5853636385761,18.7490508222521));
#7749=CARTESIAN_POINT('Ctrl Pts',(6.36936270492503,-2.59367511044622,18.7499086723365));
#7750=CARTESIAN_POINT('Ctrl Pts',(6.34523741372527,-2.61130719827547,18.7517386315419));
#7751=CARTESIAN_POINT('Ctrl Pts',(6.33231481186469,-2.62060563725948,18.752709867849));
#7752=CARTESIAN_POINT('Ctrl Pts',(6.29692131942659,-2.645677021416,18.755346047474));
#7753=CARTESIAN_POINT('Ctrl Pts',(6.27431662203581,-2.66125942566688,18.757003708272));
#7754=CARTESIAN_POINT('Ctrl Pts',(6.14725794539208,-2.7464721192601,18.7661826513142));
#7755=CARTESIAN_POINT('Ctrl Pts',(6.03899798318785,-2.81024617558669,18.7734821598319));
#7756=CARTESIAN_POINT('Ctrl Pts',(5.79545616018205,-2.93516293020397,18.7890917753257));
#7757=CARTESIAN_POINT('Ctrl Pts',(5.65912042505228,-2.9936097426788,18.7973262161945));
#7758=CARTESIAN_POINT('Ctrl Pts',(5.36020121707528,-3.09802645040613,18.8150566582545));
#7759=CARTESIAN_POINT('Ctrl Pts',(5.19706273181819,-3.14102003279783,18.8245450803554));
#7760=CARTESIAN_POINT('Ctrl Pts',(5.00483253038499,-3.1758684797173,18.8362565915394));
#7761=CARTESIAN_POINT('Ctrl Pts',(4.97827150468608,-3.18034042122053,18.8378865374679));
#7762=CARTESIAN_POINT('Ctrl Pts',(4.94146034302869,-3.18606459145615,18.8401655620948));
#7763=CARTESIAN_POINT('Ctrl Pts',(4.93125474143186,-3.18760139832158,18.840799530006));
#7764=CARTESIAN_POINT('Ctrl Pts',(4.91371750308837,-3.19015614888042,18.8418928565044));
#7765=CARTESIAN_POINT('Ctrl Pts',(4.90638934317869,-3.19119791433405,18.8423508904925));
#7766=CARTESIAN_POINT('Ctrl Pts',(4.89104354812957,-3.19332555166944,18.8433126299002));
#7767=CARTESIAN_POINT('Ctrl Pts',(4.88302535938324,-3.19440648357651,18.8438166198042));
#7768=CARTESIAN_POINT('Ctrl Pts',(4.86336909043711,-3.19698102011017,18.8450556216426));
#7769=CARTESIAN_POINT('Ctrl Pts',(4.85172682485273,-3.19844127130076,18.8457924663105));
#7770=CARTESIAN_POINT('Ctrl Pts',(4.8093689262314,-3.20351928690994,18.8484835548272));
#7771=CARTESIAN_POINT('Ctrl Pts',(4.77861068689287,-3.20675829185713,18.8504572325396));
#7772=CARTESIAN_POINT('Ctrl Pts',(4.70121818108527,-3.21378349008913,18.8554644493983));
#7773=CARTESIAN_POINT('Ctrl Pts',(4.6545401249802,-3.216997646603,18.8585218473489));
#7774=CARTESIAN_POINT('Ctrl Pts',(4.27363471350332,-3.23490492109894,18.8836915536146));
#7775=CARTESIAN_POINT('Ctrl Pts',(3.93902101098271,-3.19849399258761,18.906900344412));
#7776=CARTESIAN_POINT('Ctrl Pts',(3.55291754202133,-3.09418390780742,18.9326539648519));
#7777=CARTESIAN_POINT('Ctrl Pts',(3.49042217883087,-3.07524532503367,18.9367998591109));
#7778=CARTESIAN_POINT('Ctrl Pts',(3.40672109736123,-3.04707675217856,18.9423248363451));
#7779=CARTESIAN_POINT('Ctrl Pts',(3.38497961444894,-3.03949961818888,18.9437574399099));
#7780=CARTESIAN_POINT('Ctrl Pts',(3.34925324939164,-3.02661762234632,18.9461078309039));
#7781=CARTESIAN_POINT('Ctrl Pts',(3.33522105625367,-3.0214473366213,18.9470300391507));
#7782=CARTESIAN_POINT('Ctrl Pts',(3.30790869940422,-3.01116738226655,18.9488233570551));
#7783=CARTESIAN_POINT('Ctrl Pts',(3.29462540522846,-3.00606707124693,18.9496947538756));
#7784=CARTESIAN_POINT('Ctrl Pts',(3.26333241909884,-2.99381327201624,18.9517459861798));
#7785=CARTESIAN_POINT('Ctrl Pts',(3.24535248127419,-2.98658494069769,18.952923282763));
#7786=CARTESIAN_POINT('Ctrl Pts',(3.18557894507538,-2.96192609491856,18.9568338210127));
#7787=CARTESIAN_POINT('Ctrl Pts',(3.14408651938923,-2.94377652757285,18.9595427977026));
#7788=CARTESIAN_POINT('Ctrl Pts',(3.04576102040916,-2.89827476731839,18.9659596879517));
#7789=CARTESIAN_POINT('Ctrl Pts',(2.98932062613632,-2.8701167165736,18.9696407473141));
#7790=CARTESIAN_POINT('Ctrl Pts',(2.62460320862054,-2.67458738133287,18.9935192532195));
#7791=CARTESIAN_POINT('Ctrl Pts',(2.34466244250546,-2.45954024522084,19.0120208142239));
#7792=CARTESIAN_POINT('Ctrl Pts',(2.08611660375009,-2.18364397895329,19.0346758970734));
#7793=CARTESIAN_POINT('Ctrl Pts',(2.06759245105464,-2.16336317465537,19.0363374809732));
#7794=CARTESIAN_POINT('Ctrl Pts',(2.04242232926372,-2.13508867829872,19.03865295371));
#7795=CARTESIAN_POINT('Ctrl Pts',(2.03555184824896,-2.12729526129635,19.039291071974));
#7796=CARTESIAN_POINT('Ctrl Pts',(2.02383940043123,-2.11387921477343,19.0403896635026));
#7797=CARTESIAN_POINT('Ctrl Pts',(2.01897889721417,-2.10827277611714,19.0408487832938));
#7798=CARTESIAN_POINT('Ctrl Pts',(2.00886963138116,-2.09653036547292,19.0418105698564));
#7799=CARTESIAN_POINT('Ctrl Pts',(2.00362453591578,-2.09039141581821,19.0423135075052));
#7800=CARTESIAN_POINT('Ctrl Pts',(1.99086799162813,-2.07534682412467,19.0435461928208));
#7801=CARTESIAN_POINT('Ctrl Pts',(1.98338169825066,-2.06642008300027,19.044277731418));
#7802=CARTESIAN_POINT('Ctrl Pts',(1.95655462912258,-2.03407659224649,19.0469280719851));
#7803=CARTESIAN_POINT('Ctrl Pts',(1.93749737641811,-2.01042812468135,19.0488655657819));
#7804=CARTESIAN_POINT('Ctrl Pts',(1.89063860099345,-1.95056796563532,19.0537615591165));
#7805=CARTESIAN_POINT('Ctrl Pts',(1.86326753713745,-1.91402893803081,19.0567426691068));
#7806=CARTESIAN_POINT('Ctrl Pts',(1.74511466782522,-1.74911260872656,19.070122807827));
#7807=CARTESIAN_POINT('Ctrl Pts',(1.66302589472062,-1.61477831263553,19.0808133521838));
#7808=CARTESIAN_POINT('Ctrl Pts',(1.49390897990924,-1.28624381846734,19.1057799670569));
#7809=CARTESIAN_POINT('Ctrl Pts',(1.41561998982431,-1.08832453837688,19.119913206994));
#7810=CARTESIAN_POINT('Ctrl Pts',(1.34705079505857,-0.84796711067773,19.1357780272142));
#7811=CARTESIAN_POINT('Ctrl Pts',(1.33737180656961,-0.811641966334892,19.1381437790465));
#7812=CARTESIAN_POINT('Ctrl Pts',(1.32342020451585,-0.755340225812226,19.1417627794148));
#7813=CARTESIAN_POINT('Ctrl Pts',(1.31869849407533,-0.73547936308691,19.1430303312957));
#7814=CARTESIAN_POINT('Ctrl Pts',(1.31099644737121,-0.701657358663538,19.145173862704));
#7815=CARTESIAN_POINT('Ctrl Pts',(1.30791962556671,-0.687719037720674,19.1460529120865));
#7816=CARTESIAN_POINT('Ctrl Pts',(1.30187626068711,-0.659451031255482,19.1478271367258));
#7817=CARTESIAN_POINT('Ctrl Pts',(1.29891450926542,-0.645120656984942,19.1487221402857));
#7818=CARTESIAN_POINT('Ctrl Pts',(1.2918428951659,-0.609688968004864,19.1509243581212));
#7819=CARTESIAN_POINT('Ctrl Pts',(1.28784632917964,-0.588565565301257,19.1522279450183));
#7820=CARTESIAN_POINT('Ctrl Pts',(1.27362923061179,-0.509076373733218,19.1571000174714));
#7821=CARTESIAN_POINT('Ctrl Pts',(1.264807218163,-0.450470290566245,19.1606243420331));
#7822=CARTESIAN_POINT('Ctrl Pts',(1.24658513511028,-0.301639059924374,19.1694312479794));
#7823=CARTESIAN_POINT('Ctrl Pts',(1.2393681539368,-0.211197664560141,19.1746500614103));
#7824=CARTESIAN_POINT('Ctrl Pts',(1.23076599840026,0.0185765508398514,19.1877145216239));
#7825=CARTESIAN_POINT('Ctrl Pts',(1.2345799297012,0.157914209373653,19.1954526268538));
#7826=CARTESIAN_POINT('Ctrl Pts',(1.26255608127138,0.460635451149534,19.2124828429316));
#7827=CARTESIAN_POINT('Ctrl Pts',(1.29027651959695,0.623279101294859,19.2217751700751));
#7828=CARTESIAN_POINT('Ctrl Pts',(1.33687171770365,0.809296453501305,19.233269792944));
#7829=CARTESIAN_POINT('Ctrl Pts',(1.34377101459511,0.835439463856024,19.2349058713996));
#7830=CARTESIAN_POINT('Ctrl Pts',(1.35376076551621,0.871450124478345,19.2371919910161));
#7831=CARTESIAN_POINT('Ctrl Pts',(1.35657121447973,0.881395155964502,19.2378267948465));
#7832=CARTESIAN_POINT('Ctrl Pts',(1.36147758098768,0.898443021810753,19.2389211808651));
#7833=CARTESIAN_POINT('Ctrl Pts',(1.36355025781861,0.905552538120719,19.23937943265));
#7834=CARTESIAN_POINT('Ctrl Pts',(1.36793771408795,0.92041121814292,19.2403411765516));
#7835=CARTESIAN_POINT('Ctrl Pts',(1.37025717397582,0.928158862933251,19.2408449503942));
#7836=CARTESIAN_POINT('Ctrl Pts',(1.37600827936483,0.947109252538608,19.2420826608993));
#7837=CARTESIAN_POINT('Ctrl Pts',(1.37947188506063,0.958302109489029,19.2428184217461));
#7838=CARTESIAN_POINT('Ctrl Pts',(1.39226582107709,0.998861987740441,19.2455011456527));
#7839=CARTESIAN_POINT('Ctrl Pts',(1.40195584896868,1.02811266019896,19.2474673890269));
#7840=CARTESIAN_POINT('Ctrl Pts',(1.42733448872995,1.10119392812346,19.2524516952861));
#7841=CARTESIAN_POINT('Ctrl Pts',(1.44355589047861,1.14483104180327,19.2554933570124));
#7842=CARTESIAN_POINT('Ctrl Pts',(1.58189040738712,1.49363700090604,19.2802570552746));
#7843=CARTESIAN_POINT('Ctrl Pts',(1.74909751177648,1.7788659225165,19.3030546684332));
#7844=CARTESIAN_POINT('Ctrl Pts',(2.00089291534823,2.08834568149386,19.328811022667));
#7845=CARTESIAN_POINT('Ctrl Pts',(2.0469498138578,2.14132204965114,19.3332751884546));
#7846=CARTESIAN_POINT('Ctrl Pts',(2.11080115673308,2.21009484705856,19.3391497368552));
#7847=CARTESIAN_POINT('Ctrl Pts',(2.12709024478052,2.22725650298233,19.3406226838635));
#7848=CARTESIAN_POINT('Ctrl Pts',(2.15407656800868,2.25506849510468,19.3430218012453));
#7849=CARTESIAN_POINT('Ctrl Pts',(2.16466201690661,2.26582558802671,19.3439527626723));
#7850=CARTESIAN_POINT('Ctrl Pts',(2.1853282032757,2.28653388050096,19.3457510509876));
#7851=CARTESIAN_POINT('Ctrl Pts',(2.19539973392539,2.29649373861153,19.3466187516621));
#7852=CARTESIAN_POINT('Ctrl Pts',(2.2191269330718,2.31965044247967,19.3486429673614));
#7853=CARTESIAN_POINT('Ctrl Pts',(2.23283432096202,2.33279372014201,19.3497971333116));
#7854=CARTESIAN_POINT('Ctrl Pts',(2.27797333916505,2.37531571030506,19.3535493649714));
#7855=CARTESIAN_POINT('Ctrl Pts',(2.30987799878461,2.4041870582627,19.3561258341601));
#7856=CARTESIAN_POINT('Ctrl Pts',(2.38686016802551,2.47109566320175,19.3621755648519));
#7857=CARTESIAN_POINT('Ctrl Pts',(2.43242300171203,2.5085519497695,19.3656260383219));
#7858=CARTESIAN_POINT('Ctrl Pts',(2.70253068673412,2.71844868103846,19.3854192919508));
#7859=CARTESIAN_POINT('Ctrl Pts',(2.94796248030909,2.86193205947185,19.4007085830358));
#7860=CARTESIAN_POINT('Ctrl Pts',(3.2309808820318,2.98074927247887,19.4183296450099));
#7861=CARTESIAN_POINT('Ctrl Pts',(3.25309689062051,2.98974629025681,19.4197073812968));
#7862=CARTESIAN_POINT('Ctrl Pts',(3.33936965777885,3.02373059828085,19.4250920785058));
#7863=CARTESIAN_POINT('Ctrl Pts',(3.40421618554404,3.04690338070842,19.4291612278102));
#7864=CARTESIAN_POINT('Ctrl Pts',(3.48500511511073,3.07288660394029,19.4343143775769));
#7865=CARTESIAN_POINT('Ctrl Pts',(3.50029665751029,3.07767909158117,19.4352933961573));
#7866=CARTESIAN_POINT('Ctrl Pts',(3.52434583995685,3.0850197660745,19.4368397395733));
#7867=CARTESIAN_POINT('Ctrl Pts',(3.53307987509124,3.08764522955952,19.43740269666));
#7868=CARTESIAN_POINT('Ctrl Pts',(3.54927811117731,3.09243956759608,19.4384494910594));
#7869=CARTESIAN_POINT('Ctrl Pts',(3.55673912169654,3.09461854373629,19.4389327372406));
#7870=CARTESIAN_POINT('Ctrl Pts',(3.57394291717288,3.09957541059197,19.4400494818632));
#7871=CARTESIAN_POINT('Ctrl Pts',(3.5836909375287,3.10233435690301,19.4406840495841));
#7872=CARTESIAN_POINT('Ctrl Pts',(3.61408931549002,3.11078328819564,19.4426681333856));
#7873=CARTESIAN_POINT('Ctrl Pts',(3.63478302094563,3.11631325415694,19.4440263065033));
#7874=CARTESIAN_POINT('Ctrl Pts',(3.68345540603113,3.12880145871449,19.447235876117));
#7875=CARTESIAN_POINT('Ctrl Pts',(3.71147504787871,3.13559124898457,19.4490951792185));
#7876=CARTESIAN_POINT('Ctrl Pts',(3.8117468809298,3.1584695423951,19.4557813877245));
#7877=CARTESIAN_POINT('Ctrl Pts',(3.88445432883449,3.17244295745975,19.4606889497949));
#7878=CARTESIAN_POINT('Ctrl Pts',(4.2062636485862,3.22286831318564,19.4825006955638));
#7879=CARTESIAN_POINT('Ctrl Pts',(4.45870276160217,3.23256933229992,19.4997585902873));
#7880=CARTESIAN_POINT('Ctrl Pts',(4.80751678769213,3.20507570916502,19.5226416266125));
#7881=CARTESIAN_POINT('Ctrl Pts',(4.90493597665786,3.19290236554748,19.5289392361525));
#7882=CARTESIAN_POINT('Ctrl Pts',(5.02788771375879,3.17179865046942,19.5367693448369));
#7883=CARTESIAN_POINT('Ctrl Pts',(5.0540626374201,3.1669714150774,19.53842956906));
#7884=CARTESIAN_POINT('Ctrl Pts',(5.09561494365793,3.15877473337479,19.5410550758631));
#7885=CARTESIAN_POINT('Ctrl Pts',(5.11103218066666,3.15561601170437,19.5420270074152));
#7886=CARTESIAN_POINT('Ctrl Pts',(5.13873880317185,3.14972761978986,19.5437698850695));
#7887=CARTESIAN_POINT('Ctrl Pts',(5.15103642098971,3.14703865095611,19.5445421110312));
#7888=CARTESIAN_POINT('Ctrl Pts',(5.17988700871665,3.14055289769689,19.5463507464063));
#7889=CARTESIAN_POINT('Ctrl Pts',(5.19642644978054,3.1366971660958,19.5473852475298));
#7890=CARTESIAN_POINT('Ctrl Pts',(5.24449311352943,3.12509035378476,19.5503853628957));
#7891=CARTESIAN_POINT('Ctrl Pts',(5.27593520739811,3.11699325954761,19.552339856268));
#7892=CARTESIAN_POINT('Ctrl Pts',(5.51334540361283,3.05201361495254,19.5670484419043));
#7893=CARTESIAN_POINT('Ctrl Pts',(5.71332795076684,2.97524724648285,19.5791074001547));
#7894=CARTESIAN_POINT('Ctrl Pts',(6.10364171832906,2.77898258731845,19.6035518423707));
#7895=CARTESIAN_POINT('Ctrl Pts',(6.29204193627464,2.6583013428099,19.6158758171254));
#7896=CARTESIAN_POINT('Ctrl Pts',(6.48575271537412,2.5037444153385,19.6307654613275));
#7897=CARTESIAN_POINT('Ctrl Pts',(6.50488815946412,2.48811321326056,19.6322631243497));
#7898=CARTESIAN_POINT('Ctrl Pts',(6.5314812282206,2.46587539012949,19.6343854701012));
#7899=CARTESIAN_POINT('Ctrl Pts',(6.53909136526391,2.45945141569425,19.6349976155408));
#7900=CARTESIAN_POINT('Ctrl Pts',(6.55223512660553,2.4482515760214,19.6360634662144));
#7901=CARTESIAN_POINT('Ctrl Pts',(6.55778255483201,2.44349192342877,19.6365159964752));
#7902=CARTESIAN_POINT('Ctrl Pts',(6.5688662864211,2.43391650599394,19.63742564692));
#7903=CARTESIAN_POINT('Ctrl Pts',(6.57440241677802,2.4291006348124,19.6378827771027));
#7904=CARTESIAN_POINT('Ctrl Pts',(6.58810309283819,2.41709999615866,19.6390208744963));
#7905=CARTESIAN_POINT('Ctrl Pts',(6.59624774730844,2.40989277842168,19.6397034794654));
#7906=CARTESIAN_POINT('Ctrl Pts',(6.62430453059871,2.38481092206498,19.6420754299712));
#7907=CARTESIAN_POINT('Ctrl Pts',(6.64402981069565,2.36673015301993,19.6437790587012));
#7908=CARTESIAN_POINT('Ctrl Pts',(6.69205800368811,2.32159273968159,19.6480118762703));
#7909=CARTESIAN_POINT('Ctrl Pts',(6.72009682115932,2.29426237771427,19.6505574892609));
#7910=CARTESIAN_POINT('Ctrl Pts',(6.83198874344166,2.18114950111979,19.6609992481329));
#7911=CARTESIAN_POINT('Ctrl Pts',(6.91151600031204,2.09123121786874,19.6690834558953));
#7912=CARTESIAN_POINT('Ctrl Pts',(7.15005330590126,1.78911772960194,19.6951138797229));
#7913=CARTESIAN_POINT('Ctrl Pts',(7.28802045389854,1.56163615300294,19.7129654140903));
#7914=CARTESIAN_POINT('Ctrl Pts',(7.41249373904646,1.28434640594354,19.7322207066652));
#7915=CARTESIAN_POINT('Ctrl Pts',(7.4277642035746,1.24861242055775,19.7346606520895));
#7916=CARTESIAN_POINT('Ctrl Pts',(7.44917336138777,1.19589475783665,19.7382014265732));
#7917=CARTESIAN_POINT('Ctrl Pts',(7.45582110338722,1.17912283033489,19.7393193256318));
#7918=CARTESIAN_POINT('Ctrl Pts',(7.4674016762598,1.14917385464136,19.7413005508085));
#7919=CARTESIAN_POINT('Ctrl Pts',(7.47238966869084,1.13601877640831,19.7421657083397));
#7920=CARTESIAN_POINT('Ctrl Pts',(7.48264437499337,1.10842990715336,19.7439696643334));
#7921=CARTESIAN_POINT('Ctrl Pts',(7.48789434626524,1.09399023909491,19.7449078868439));
#7922=CARTESIAN_POINT('Ctrl Pts',(7.50138495162219,1.05604240740201,19.747358350578));
#7923=CARTESIAN_POINT('Ctrl Pts',(7.50945674196058,1.03247499774353,19.7488649860863));
#7924=CARTESIAN_POINT('Ctrl Pts',(7.54547170056723,0.923204248036363,19.7557834829227));
#7925=CARTESIAN_POINT('Ctrl Pts',(7.5700860779861,0.836441642686329,19.7610859848423));
#7926=CARTESIAN_POINT('Ctrl Pts',(7.64962599100909,0.503458342021578,19.7808852707807));
#7927=CARTESIAN_POINT('Ctrl Pts',(7.67921910621825,0.252160529432019,19.7946332277895));
#7928=CARTESIAN_POINT('Ctrl Pts',(7.67921910621823,5.28268401245313E-12,
19.808946496524));
#7929=CARTESIAN_POINT('Ctrl Pts',(7.67921910621823,-6.1812332959659E-13,
19.5612501365773));
#7930=CARTESIAN_POINT('Ctrl Pts',(7.67921910621824,0.0284028134448205,19.5594599908969));
#7931=CARTESIAN_POINT('Ctrl Pts',(7.67884362626994,0.0568051021141802,19.5576814802244));
#7932=CARTESIAN_POINT('Ctrl Pts',(7.67761897452903,0.103112508301193,19.5548000166224));
#7933=CARTESIAN_POINT('Ctrl Pts',(7.67699584377862,0.121021555604613,19.5536900801427));
#7934=CARTESIAN_POINT('Ctrl Pts',(7.67561927970105,0.152925139774606,19.5517204798415));
#7935=CARTESIAN_POINT('Ctrl Pts',(7.67492387973481,0.166921593822558,19.5508590253468));
#7936=CARTESIAN_POINT('Ctrl Pts',(7.67326251877794,0.196470055880185,19.5490457541829));
#7937=CARTESIAN_POINT('Ctrl Pts',(7.67227501624166,0.212020528141493,19.5480946339856));
#7938=CARTESIAN_POINT('Ctrl Pts',(7.66934537366983,0.253406518687992,19.5455713599666));
#7939=CARTESIAN_POINT('Ctrl Pts',(7.66720438560732,0.279227145878171,19.5440054488619));
#7940=CARTESIAN_POINT('Ctrl Pts',(7.65507507029223,0.406806685643112,19.5363060465622));
#7941=CARTESIAN_POINT('Ctrl Pts',(7.64055891975178,0.508081580129581,19.5303156947538));
#7942=CARTESIAN_POINT('Ctrl Pts',(7.57968009677215,0.824708082173789,19.5117654486567));
#7943=CARTESIAN_POINT('Ctrl Pts',(7.51606598448357,1.03607783163774,19.4996820645383));
#7944=CARTESIAN_POINT('Ctrl Pts',(7.37915361851138,1.36473161287488,19.4795795335781));
#7945=CARTESIAN_POINT('Ctrl Pts',(7.31903328111939,1.48670593372855,19.4717828342671));
#7946=CARTESIAN_POINT('Ctrl Pts',(7.24300181497109,1.61914730139673,19.4625396856323));
#7947=CARTESIAN_POINT('Ctrl Pts',(7.23448274576251,1.63372051199936,19.4615115163708));
#7948=CARTESIAN_POINT('Ctrl Pts',(7.22067260852757,1.65692457062143,19.4598554855769));
#7949=CARTESIAN_POINT('Ctrl Pts',(7.21545455007141,1.66559879594775,19.4592321446015));
#7950=CARTESIAN_POINT('Ctrl Pts',(7.20611294479588,1.68096344046085,19.4581201369868));
#7951=CARTESIAN_POINT('Ctrl Pts',(7.20200567928381,1.68766354811799,19.4576325282135));
#7952=CARTESIAN_POINT('Ctrl Pts',(7.19312142660486,1.70203799921369,19.4565805265562));
#7953=CARTESIAN_POINT('Ctrl Pts',(7.18833672829888,1.70970715743046,19.4560156515672));
#7954=CARTESIAN_POINT('Ctrl Pts',(7.17494340626888,1.73097489109188,19.454439346266));
#7955=CARTESIAN_POINT('Ctrl Pts',(7.1662652205259,1.74452904461202,19.4534235223688));
#7956=CARTESIAN_POINT('Ctrl Pts',(7.11464894778162,1.82383226277776,19.4474164184023));
#7957=CARTESIAN_POINT('Ctrl Pts',(7.06942417959728,1.88805397283022,19.4422930748145));
#7958=CARTESIAN_POINT('Ctrl Pts',(6.89503696942675,2.1174139224218,19.4232028274105));
#7959=CARTESIAN_POINT('Ctrl Pts',(6.75219512034282,2.27149716107704,19.4088336427382));
#7960=CARTESIAN_POINT('Ctrl Pts',(6.47067612865167,2.52128759044676,19.3836595480727));
#7961=CARTESIAN_POINT('Ctrl Pts',(6.33753648553057,2.622121576431,19.3727560120323));
#7962=CARTESIAN_POINT('Ctrl Pts',(6.17425368615352,2.72691678961993,19.3605416897803));
#7963=CARTESIAN_POINT('Ctrl Pts',(6.15115129476806,2.7413338712202,19.3588381531205));
#7964=CARTESIAN_POINT('Ctrl Pts',(6.11294209067534,2.76451073104742,19.3560601364328));
#7965=CARTESIAN_POINT('Ctrl Pts',(6.09794226200795,2.77344338834173,19.3549793730167));
#7966=CARTESIAN_POINT('Ctrl Pts',(6.07081270686615,2.7893023086204,19.3530419576122));
#7967=CARTESIAN_POINT('Ctrl Pts',(6.05870922482919,2.79627238334953,19.3521837328245));
#7968=CARTESIAN_POINT('Ctrl Pts',(6.03276225934852,2.81099077154585,19.3503567607638));
#7969=CARTESIAN_POINT('Ctrl Pts',(6.01890606480431,2.81871601741629,19.3493888583142));
#7970=CARTESIAN_POINT('Ctrl Pts',(5.98113818119996,2.8394086812677,19.3467711719543));
#7971=CARTESIAN_POINT('Ctrl Pts',(5.95711812001484,2.85217637141784,19.3451284965258));
#7972=CARTESIAN_POINT('Ctrl Pts',(5.82515080698649,2.92019392826158,19.3362189774638));
#7973=CARTESIAN_POINT('Ctrl Pts',(5.71430642120297,2.96962493182002,19.3291581123835));
#7974=CARTESIAN_POINT('Ctrl Pts',(5.44905878241921,3.07038700212826,19.3129521507839));
#7975=CARTESIAN_POINT('Ctrl Pts',(5.29304319525379,3.11651347471885,19.3039428106329));
#7976=CARTESIAN_POINT('Ctrl Pts',(5.0517760840782,3.16841240823839,19.2901080260325));
#7977=CARTESIAN_POINT('Ctrl Pts',(4.96867978540304,3.18290223988415,19.285357048519));
#7978=CARTESIAN_POINT('Ctrl Pts',(4.7961623552028,3.20605381663788,19.2753609849281));
#7979=CARTESIAN_POINT('Ctrl Pts',(4.7067583357602,3.21426894372378,19.2701081000082));
#7980=CARTESIAN_POINT('Ctrl Pts',(4.6014022833881,3.21952793714187,19.2637133667542));
#7981=CARTESIAN_POINT('Ctrl Pts',(4.58566227810978,3.22019795439139,19.2627526420184));
#7982=CARTESIAN_POINT('Ctrl Pts',(4.56002857035624,3.22110088775643,19.2611783906873));
#7983=CARTESIAN_POINT('Ctrl Pts',(4.55013738545256,3.22140369080439,19.2605686035396));
#7984=CARTESIAN_POINT('Ctrl Pts',(4.53242193643426,3.22186436300611,19.2594720208778));
#7985=CARTESIAN_POINT('Ctrl Pts',(4.52459831095192,3.22203929448222,19.2589861795267));
#7986=CARTESIAN_POINT('Ctrl Pts',(4.50745303428729,3.22236017733644,19.2579180030989));
#7987=CARTESIAN_POINT('Ctrl Pts',(4.49813148891168,3.22249417596578,19.2573350356344));
#7988=CARTESIAN_POINT('Ctrl Pts',(4.47139727390988,3.22276246922788,19.2556569673354));
#7989=CARTESIAN_POINT('Ctrl Pts',(4.45398423262307,3.22279608061584,19.2545565357168));
#7990=CARTESIAN_POINT('Ctrl Pts',(4.32762242154845,3.22201592298449,19.2465211332876));
#7991=CARTESIAN_POINT('Ctrl Pts',(4.21878769952972,3.21581881108584,19.239333251583));
#7992=CARTESIAN_POINT('Ctrl Pts',(3.88297921849647,3.17955827093561,19.2167184685112));
#7993=CARTESIAN_POINT('Ctrl Pts',(3.6587069476032,3.13082621787041,19.2010442730002));
#7994=CARTESIAN_POINT('Ctrl Pts',(3.32892572613319,3.02139517416331,19.1781380637038));
#7995=CARTESIAN_POINT('Ctrl Pts',(3.21850152632271,2.97785574094803,19.1704813730009));
#7996=CARTESIAN_POINT('Ctrl Pts',(3.08548787489987,2.91672744617726,19.1612816023624));
#7997=CARTESIAN_POINT('Ctrl Pts',(3.06040853826933,2.90480696434155,19.15954779632));
#7998=CARTESIAN_POINT('Ctrl Pts',(3.02099160519675,2.88544323898276,19.1568233537176));
#7999=CARTESIAN_POINT('Ctrl Pts',(3.00655098183327,2.87821399292753,19.1558253557429));
#8000=CARTESIAN_POINT('Ctrl Pts',(2.97974789858912,2.86454295425033,19.153972988634));
#8001=CARTESIAN_POINT('Ctrl Pts',(2.96737177343201,2.85812893427789,19.1531176739155));
#8002=CARTESIAN_POINT('Ctrl Pts',(2.93993540028403,2.84368324200678,19.1512213564351));
#8003=CARTESIAN_POINT('Ctrl Pts',(2.92489648808655,2.83561178494986,19.1501817867059));
#8004=CARTESIAN_POINT('Ctrl Pts',(2.8810704172853,2.81163973676643,19.1471513865489));
#8005=CARTESIAN_POINT('Ctrl Pts',(2.85246114196138,2.7954172513468,19.1451720324541));
#8006=CARTESIAN_POINT('Ctrl Pts',(2.78809754152416,2.75760725675333,19.1407127803965));
#8007=CARTESIAN_POINT('Ctrl Pts',(2.75250415606485,2.7357567754428,19.1382423714925));
#8008=CARTESIAN_POINT('Ctrl Pts',(2.63552980961425,2.66077834018514,19.1300951050013));
#8009=CARTESIAN_POINT('Ctrl Pts',(2.55612543648521,2.60466068879597,19.1245193731635));
#8010=CARTESIAN_POINT('Ctrl Pts',(2.37396676754032,2.46315191822,19.1114506277655));
#8011=CARTESIAN_POINT('Ctrl Pts',(2.27374693985957,2.37479641840688,19.1040346741214));
#8012=CARTESIAN_POINT('Ctrl Pts',(2.12224360462592,2.22351279194915,19.0920343033402));
#8013=CARTESIAN_POINT('Ctrl Pts',(2.06735221619393,2.16442541186132,19.0874942082041));
#8014=CARTESIAN_POINT('Ctrl Pts',(1.95307594700382,2.03176425318163,19.0774610189337));
#8015=CARTESIAN_POINT('Ctrl Pts',(1.89459891611928,1.95751396894585,19.071943188041));
#8016=CARTESIAN_POINT('Ctrl Pts',(1.83016477499899,1.86785907174852,19.0652520520684));
#8017=CARTESIAN_POINT('Ctrl Pts',(1.82095301426016,1.85483876861369,19.0642796320921));
#8018=CARTESIAN_POINT('Ctrl Pts',(1.80614955796381,1.83358199981329,19.0626900151264));
#8019=CARTESIAN_POINT('Ctrl Pts',(1.8004985903824,1.82538688248569,19.0620766794753));
#8020=CARTESIAN_POINT('Ctrl Pts',(1.79047113697588,1.81069977894365,19.0609763453953));
#8021=CARTESIAN_POINT('Ctrl Pts',(1.78608023266023,1.80421787023806,19.0604903299256));
#8022=CARTESIAN_POINT('Ctrl Pts',(1.77653848302074,1.79002107927728,19.0594249220416));
#8023=CARTESIAN_POINT('Ctrl Pts',(1.77139738636968,1.78230004870439,19.0588449215007));
#8024=CARTESIAN_POINT('Ctrl Pts',(1.75682193545894,1.7602040687787,19.0571837057389));
#8025=CARTESIAN_POINT('Ctrl Pts',(1.74746935884358,1.74577591596484,19.0560973206201));
#8026=CARTESIAN_POINT('Ctrl Pts',(1.68307586287662,1.64467306830056,19.0484770270223));
#8027=CARTESIAN_POINT('Ctrl Pts',(1.63209426850302,1.55549414585811,19.0417181555772));
#8028=CARTESIAN_POINT('Ctrl Pts',(1.51923625788486,1.33417828896631,19.0251146507008));
#8029=CARTESIAN_POINT('Ctrl Pts',(1.46190063927246,1.19996987354799,19.0151905873257));
#8030=CARTESIAN_POINT('Ctrl Pts',(1.34652797073386,0.869534611765488,18.9916125838002));
#8031=CARTESIAN_POINT('Ctrl Pts',(1.29767767003671,0.670736596291064,18.9781351894585));
#8032=CARTESIAN_POINT('Ctrl Pts',(1.26399286815807,0.441544956596039,18.9635498492786));
#8033=CARTESIAN_POINT('Ctrl Pts',(1.26035846307727,0.414419244593152,18.9618376356025));
#8034=CARTESIAN_POINT('Ctrl Pts',(1.25496723760914,0.369877761204898,18.9590484201937));
#8035=CARTESIAN_POINT('Ctrl Pts',(1.25300604329656,0.35248857680413,18.9579650488734));
#8036=CARTESIAN_POINT('Ctrl Pts',(1.24973399716544,0.321189462773992,18.9560247902201));
#8037=CARTESIAN_POINT('Ctrl Pts',(1.24837179016518,0.307285455418795,18.9551663106272));
#8038=CARTESIAN_POINT('Ctrl Pts',(1.24565840944089,0.277602272062222,18.9533407302291));
#8039=CARTESIAN_POINT('Ctrl Pts',(1.24433304174656,0.261821063545848,18.952374460107));
#8040=CARTESIAN_POINT('Ctrl Pts',(1.24105709782643,0.219034749994791,18.9497659731991));
#8041=CARTESIAN_POINT('Ctrl Pts',(1.2393303900664,0.192013422287832,18.9481307784456));
#8042=CARTESIAN_POINT('Ctrl Pts',(1.23184263457491,0.0459316960763701,18.9393518022687));
#8043=CARTESIAN_POINT('Ctrl Pts',(1.2323493970452,-0.0733639267330349,18.9324065843272));
#8044=CARTESIAN_POINT('Ctrl Pts',(1.24881839190477,-0.34877783578518,18.9166364767785));
#8045=CARTESIAN_POINT('Ctrl Pts',(1.26956607212594,-0.504301731685991,18.9079330095582));
#8046=CARTESIAN_POINT('Ctrl Pts',(1.33561694647016,-0.821141560418656,18.8898066780825));
#8047=CARTESIAN_POINT('Ctrl Pts',(1.38233454330533,-0.981669399701871,18.8803982146996));
#8048=CARTESIAN_POINT('Ctrl Pts',(1.45078014272268,-1.16304667717598,18.868776835227));
#8049=CARTESIAN_POINT('Ctrl Pts',(1.4606097308252,-1.18813728742322,18.8671461459863));
#8050=CARTESIAN_POINT('Ctrl Pts',(1.47463770315148,-1.22266331602778,18.8648663045421));
#8051=CARTESIAN_POINT('Ctrl Pts',(1.47856884446939,-1.23220701386692,18.8642322788332));
#8052=CARTESIAN_POINT('Ctrl Pts',(1.48539756755589,-1.24856167606506,18.8631389112664));
#8053=CARTESIAN_POINT('Ctrl Pts',(1.48827292118004,-1.25538191452222,18.8626808946013));
#8054=CARTESIAN_POINT('Ctrl Pts',(1.49433993559444,-1.26963529319562,18.8617192633322));
#8055=CARTESIAN_POINT('Ctrl Pts',(1.4975361092922,-1.27706637094985,18.8612153647438));
#8056=CARTESIAN_POINT('Ctrl Pts',(1.5054351826832,-1.29524280598295,18.8599767125325));
#8057=CARTESIAN_POINT('Ctrl Pts',(1.51016880833146,-1.3059746126881,18.8592401279763));
#8058=CARTESIAN_POINT('Ctrl Pts',(1.52758759172565,-1.34488876800186,18.856550722299));
#8059=CARTESIAN_POINT('Ctrl Pts',(1.54061894688311,-1.37291311039747,18.8545784968055));
#8060=CARTESIAN_POINT('Ctrl Pts',(1.57436636151043,-1.44283958007649,18.8495756689546));
#8061=CARTESIAN_POINT('Ctrl Pts',(1.59559438249457,-1.48448565403595,18.8465212560641));
#8062=CARTESIAN_POINT('Ctrl Pts',(1.77556520152065,-1.81935345055736,18.8214289343213));
#8063=CARTESIAN_POINT('Ctrl Pts',(1.9780413249982,-2.08680739637278,18.798298446561));
#8064=CARTESIAN_POINT('Ctrl Pts',(2.26563234168041,-2.36447377002062,18.7725442661621));
#8065=CARTESIAN_POINT('Ctrl Pts',(2.31467651749506,-2.40898889116164,18.7683378607335));
#8066=CARTESIAN_POINT('Ctrl Pts',(2.38266895772846,-2.46698320627207,18.7627463906983));
#8067=CARTESIAN_POINT('Ctrl Pts',(2.40043904753291,-2.48181257119949,18.7613061350128));
#8068=CARTESIAN_POINT('Ctrl Pts',(2.42997088242678,-2.50592236094837,18.7589465747357));
#8069=CARTESIAN_POINT('Ctrl Pts',(2.44164009658245,-2.51531429530023,18.758022779417));
#8070=CARTESIAN_POINT('Ctrl Pts',(2.46450903369547,-2.5334590297333,18.7562287613204));
#8071=CARTESIAN_POINT('Ctrl Pts',(2.47570200084537,-2.54221975256697,18.7553582343435));
#8072=CARTESIAN_POINT('Ctrl Pts',(2.50222665807577,-2.56269904202215,18.7533127457653));
#8073=CARTESIAN_POINT('Ctrl Pts',(2.51760647078688,-2.57435460496161,18.7521402836861));
#8074=CARTESIAN_POINT('Ctrl Pts',(2.56904525256626,-2.6126149211951,18.7482627808874));
#8075=CARTESIAN_POINT('Ctrl Pts',(2.6055552952843,-2.63860642957818,18.7455814365296));
#8076=CARTESIAN_POINT('Ctrl Pts',(2.69400860160376,-2.69883664266446,18.7392414632741));
#8077=CARTESIAN_POINT('Ctrl Pts',(2.74642497978504,-2.73234990690381,18.7356088055959));
#8078=CARTESIAN_POINT('Ctrl Pts',(3.0837497800168,-2.93451198513313,18.7129035866159));
#8079=CARTESIAN_POINT('Ctrl Pts',(3.39219217606696,-3.05989792512018,18.6953187470104));
#8080=CARTESIAN_POINT('Ctrl Pts',(3.75671554730795,-3.1461667447413,18.6731889307832));
#8081=CARTESIAN_POINT('Ctrl Pts',(3.79935984609438,-3.15534898672469,18.6705768903142));
#8082=CARTESIAN_POINT('Ctrl Pts',(3.85577291121581,-3.16630281564717,18.6670754944602));
#8083=CARTESIAN_POINT('Ctrl Pts',(3.86938749318509,-3.16885540893573,18.6662269686365));
#8084=CARTESIAN_POINT('Ctrl Pts',(3.89142656585196,-3.17284060566614,18.6648471053794));
#8085=CARTESIAN_POINT('Ctrl Pts',(3.89984120809032,-3.17432763911187,18.6643187886612));
#8086=CARTESIAN_POINT('Ctrl Pts',(3.91616047543904,-3.17714469268053,18.6632911423174));
#8087=CARTESIAN_POINT('Ctrl Pts',(3.9240642674348,-3.17847870795283,18.6627920390091));
#8088=CARTESIAN_POINT('Ctrl Pts',(3.94316171485472,-3.18162877818692,18.6615828478592));
#8089=CARTESIAN_POINT('Ctrl Pts',(3.95436008541971,-3.18341525446944,18.660871123889));
#8090=CARTESIAN_POINT('Ctrl Pts',(3.99360126614107,-3.18946319742835,18.6583682968408));
#8091=CARTESIAN_POINT('Ctrl Pts',(4.02168980010099,-3.19341337003237,18.6565610616655));
#8092=CARTESIAN_POINT('Ctrl Pts',(4.09114501240988,-3.20224776979922,18.6520595007502));
#8093=CARTESIAN_POINT('Ctrl Pts',(4.13256046724244,-3.20670162922516,18.649346712081));
#8094=CARTESIAN_POINT('Ctrl Pts',(4.30685694327721,-3.22203481229416,18.6378410092712));
#8095=CARTESIAN_POINT('Ctrl Pts',(4.44025521368895,-3.22546514583296,18.6288241015408));
#8096=CARTESIAN_POINT('Ctrl Pts',(4.67216988319575,-3.2170396986303,18.6131238551325));
#8097=CARTESIAN_POINT('Ctrl Pts',(4.77065164042923,-3.20891910176094,18.6064479200548));
#8098=CARTESIAN_POINT('Ctrl Pts',(5.02973886243387,-3.17551166064296,18.5889929843748));
#8099=CARTESIAN_POINT('Ctrl Pts',(5.18908686061228,-3.14257819092676,18.578380896443));
#8100=CARTESIAN_POINT('Ctrl Pts',(5.37135960031064,-3.09027966229791,18.5664442057519));
#8101=CARTESIAN_POINT('Ctrl Pts',(5.39733207173869,-3.08247140452727,18.5647477379578));
#8102=CARTESIAN_POINT('Ctrl Pts',(5.43982506973266,-3.06910935044628,18.5619788477785));
#8103=CARTESIAN_POINT('Ctrl Pts',(5.456404191201,-3.06374786836112,18.5609002118603));
#8104=CARTESIAN_POINT('Ctrl Pts',(5.48619032871492,-3.05384786034121,18.5589651105043));
#8105=CARTESIAN_POINT('Ctrl Pts',(5.49941277458038,-3.04935748388561,18.5581070881436));
#8106=CARTESIAN_POINT('Ctrl Pts',(5.52761502782939,-3.03957502938459,18.5562789541222));
#8107=CARTESIAN_POINT('Ctrl Pts',(5.54258577479633,-3.03425782375398,18.5553096989619));
#8108=CARTESIAN_POINT('Ctrl Pts',(5.58184263461627,-3.01998707422332,18.5527708216865));
#8109=CARTESIAN_POINT('Ctrl Pts',(5.60606156715453,-3.01085116536941,18.5512072804521));
#8110=CARTESIAN_POINT('Ctrl Pts',(5.72081351659151,-2.96597771025322,18.5438088551703));
#8111=CARTESIAN_POINT('Ctrl Pts',(5.80981170062668,-2.92644101777471,18.53810221279));
#8112=CARTESIAN_POINT('Ctrl Pts',(6.08107114380992,-2.79090964207324,18.5206326629969));
#8113=CARTESIAN_POINT('Ctrl Pts',(6.25600715633322,-2.68144991614729,18.5092828111469));
#8114=CARTESIAN_POINT('Ctrl Pts',(6.54122512580693,-2.46242533557525,18.489062015714));
#8115=CARTESIAN_POINT('Ctrl Pts',(6.65627179950778,-2.36021229459978,18.4803049468223));
#8116=CARTESIAN_POINT('Ctrl Pts',(6.77654386822955,-2.23689870377663,18.469880098456));
#8117=CARTESIAN_POINT('Ctrl Pts',(6.78940000652789,-2.2234873711176,18.4687479413034));
#8118=CARTESIAN_POINT('Ctrl Pts',(6.80878187051918,-2.20291535449392,18.4670123469773));
#8119=CARTESIAN_POINT('Ctrl Pts',(6.81539269116201,-2.19583490154854,18.4664151787582));
#8120=CARTESIAN_POINT('Ctrl Pts',(6.82728087634721,-2.18298653960332,18.4653316422684));
#8121=CARTESIAN_POINT('Ctrl Pts',(6.83256928120214,-2.17722911910111,18.464846125054));
#8122=CARTESIAN_POINT('Ctrl Pts',(6.84424036793362,-2.1644297836629,18.4637667897289));
#8123=CARTESIAN_POINT('Ctrl Pts',(6.85061279840961,-2.15737893342536,18.4631722456997));
#8124=CARTESIAN_POINT('Ctrl Pts',(6.868571778697,-2.13733044898643,18.4614820778406));
#8125=CARTESIAN_POINT('Ctrl Pts',(6.88008410594439,-2.12426718011805,18.4603812254201));
#8126=CARTESIAN_POINT('Ctrl Pts',(6.96367984521711,-2.02784530129074,18.4522629875831));
#8127=CARTESIAN_POINT('Ctrl Pts',(7.0315442423832,-1.94093925228313,18.4449877250534));
#8128=CARTESIAN_POINT('Ctrl Pts',(7.19396226978649,-1.7094018381902,18.4260422844694));
#8129=CARTESIAN_POINT('Ctrl Pts',(7.2815902684104,-1.5603257326243,18.414261610783));
#8130=CARTESIAN_POINT('Ctrl Pts',(7.43054058563359,-1.25283052626814,18.3913955725114));
#8131=CARTESIAN_POINT('Ctrl Pts',(7.49215259885276,-1.09513780678663,18.3803367662456));
#8132=CARTESIAN_POINT('Ctrl Pts',(7.54901462110506,-0.907206656555523,18.3679754710214));
#8133=CARTESIAN_POINT('Ctrl Pts',(7.5565829108954,-0.880997247951465,18.3662688514602));
#8134=CARTESIAN_POINT('Ctrl Pts',(7.56845146465908,-0.837847625456554,18.3634868554092));
#8135=CARTESIAN_POINT('Ctrl Pts',(7.57294821698209,-0.820963345194926,18.362405164962));
#8136=CARTESIAN_POINT('Ctrl Pts',(7.58079235911721,-0.790516841477836,18.3604667397016));
#8137=CARTESIAN_POINT('Ctrl Pts',(7.58418928022844,-0.776967945348729,18.3596084251712));
#8138=CARTESIAN_POINT('Ctrl Pts',(7.59125350125708,-0.747994456986186,18.3577819518879));
#8139=CARTESIAN_POINT('Ctrl Pts',(7.59489529453537,-0.732563980546522,18.3568146329101));
#8140=CARTESIAN_POINT('Ctrl Pts',(7.60209524151769,-0.701017919631405,18.354847777982));
#8141=CARTESIAN_POINT('Ctrl Pts',(7.60564377269254,-0.684900607586468,18.3538485726264));
#8142=CARTESIAN_POINT('Ctrl Pts',(7.61424658985375,-0.644345884572817,18.3513481536081));
#8143=CARTESIAN_POINT('Ctrl Pts',(7.61914119440518,-0.619875446692365,18.3498519651881));
#8144=CARTESIAN_POINT('Ctrl Pts',(7.66064905192815,-0.399052284398737,18.3364563363126));
#8145=CARTESIAN_POINT('Ctrl Pts',(7.67921910620918,-0.199750373277688,18.3251566808499));
#8146=CARTESIAN_POINT('Ctrl Pts',(7.67921910621823,-1.45987597011121E-10,
18.3139723139554));
#8147=CARTESIAN_POINT('Origin',(4.45646910621825,-5.13094777615093E-16,
-2.31077344927308));
#8148=CARTESIAN_POINT('',(7.67921904541622,-0.000626018863251772,17.0671267778236));
#8149=CARTESIAN_POINT('',(7.67921910621823,1.77253683985415E-10,17.3115866477388));
#8150=CARTESIAN_POINT('',(7.67921910621823,-3.51191647465084E-13,-2.31077344927308));
#8151=CARTESIAN_POINT('Ctrl Pts',(7.67921910621823,1.77258589750817E-10,
17.3115866477388));
#8152=CARTESIAN_POINT('Ctrl Pts',(7.67921910622848,-0.186420830783714,17.3241302593115));
#8153=CARTESIAN_POINT('Ctrl Pts',(7.66304408358115,-0.372522916221347,17.336428873084));
#8154=CARTESIAN_POINT('Ctrl Pts',(7.62644079621295,-0.581422353333308,17.3498435584536));
#8155=CARTESIAN_POINT('Ctrl Pts',(7.62172382977166,-0.606576511156904,17.351452896662));
#8156=CARTESIAN_POINT('Ctrl Pts',(7.61342130711023,-0.648113788347165,17.3541009479764));
#8157=CARTESIAN_POINT('Ctrl Pts',(7.61000667899512,-0.66452951440673,17.3551450134735));
#8158=CARTESIAN_POINT('Ctrl Pts',(7.6030750777652,-0.696595792055698,17.3571798672976));
#8159=CARTESIAN_POINT('Ctrl Pts',(7.5995690681753,-0.712248188271752,17.3581709731876));
#8160=CARTESIAN_POINT('Ctrl Pts',(7.59279576613295,-0.741462898034154,17.3600170071803));
#8161=CARTESIAN_POINT('Ctrl Pts',(7.58955700422825,-0.75503137674913,17.3608728258405));
#8162=CARTESIAN_POINT('Ctrl Pts',(7.58212511123354,-0.785295100588523,17.3627784000746));
#8163=CARTESIAN_POINT('Ctrl Pts',(7.57788609335654,-0.80197871978988,17.3638266540774));
#8164=CARTESIAN_POINT('Ctrl Pts',(7.56680151022728,-0.844184880978747,17.3664733104739));
#8165=CARTESIAN_POINT('Ctrl Pts',(7.55977526634653,-0.869658965258959,17.368065872046));
#8166=CARTESIAN_POINT('Ctrl Pts',(7.51283540917338,-1.03202439684236,17.3781904264158));
#8167=CARTESIAN_POINT('Ctrl Pts',(7.46418491208713,-1.16623413737935,17.3864305006333));
#8168=CARTESIAN_POINT('Ctrl Pts',(7.36008960238266,-1.40306098963202,17.4010965748994));
#8169=CARTESIAN_POINT('Ctrl Pts',(7.3076722618481,-1.50672943085777,17.4075665322756));
#8170=CARTESIAN_POINT('Ctrl Pts',(7.16179562435811,-1.7602395622959,17.4239294390725));
#8171=CARTESIAN_POINT('Ctrl Pts',(7.06142110399511,-1.90563505192807,17.4338212469983));
#8172=CARTESIAN_POINT('Ctrl Pts',(6.93068215346667,-2.0652567904974,17.4461581226165));
#8173=CARTESIAN_POINT('Ctrl Pts',(6.91136961550979,-2.08817603594508,17.4479686638805));
#8174=CARTESIAN_POINT('Ctrl Pts',(6.88405247088113,-2.11969204555891,17.4505188087015));
#8175=CARTESIAN_POINT('Ctrl Pts',(6.8763156199805,-2.12852019025575,17.4512398951258));
#8176=CARTESIAN_POINT('Ctrl Pts',(6.86316444797489,-2.14336197855872,17.452464027224));
#8177=CARTESIAN_POINT('Ctrl Pts',(6.85777529809564,-2.14939796460141,17.4529652179073));
#8178=CARTESIAN_POINT('Ctrl Pts',(6.84741375375233,-2.1609155529316,17.4539281423202));
#8179=CARTESIAN_POINT('Ctrl Pts',(6.84244512575294,-2.16640041683573,17.4543895770759));
#8180=CARTESIAN_POINT('Ctrl Pts',(6.83050516873597,-2.17949002490294,17.4554975858097));
#8181=CARTESIAN_POINT('Ctrl Pts',(6.82351618001147,-2.18707844816694,17.4561454645131));
#8182=CARTESIAN_POINT('Ctrl Pts',(6.79816967737895,-2.21433507795057,17.4584921841782));
#8183=CARTESIAN_POINT('Ctrl Pts',(6.77960305237923,-2.23380616010508,17.460205743448));
#8184=CARTESIAN_POINT('Ctrl Pts',(6.63766692459036,-2.37897309807701,17.4732492449244));
#8185=CARTESIAN_POINT('Ctrl Pts',(6.50443354318551,-2.49458757580444,17.4851617202718));
#8186=CARTESIAN_POINT('Ctrl Pts',(6.34242047661592,-2.61341181388632,17.4987544719417));
#8187=CARTESIAN_POINT('Ctrl Pts',(6.32223270782824,-2.62786226201846,17.5004339739429));
#8188=CARTESIAN_POINT('Ctrl Pts',(6.17041707209726,-2.73390084889562,17.5129517060931));
#8189=CARTESIAN_POINT('Ctrl Pts',(6.03227208164215,-2.81579231687521,17.5237020720199));
#8190=CARTESIAN_POINT('Ctrl Pts',(5.83729536214465,-2.91251011829875,17.5378531217607));
#8191=CARTESIAN_POINT('Ctrl Pts',(5.78532771960922,-2.93658505229964,17.5415344416708));
#8192=CARTESIAN_POINT('Ctrl Pts',(5.69438281561168,-2.97580786713871,17.5478223068354));
#8193=CARTESIAN_POINT('Ctrl Pts',(5.65570273264038,-2.991605219019,17.5504496919431));
#8194=CARTESIAN_POINT('Ctrl Pts',(5.59968004556968,-3.0132242038267,17.5541897869111));
#8195=CARTESIAN_POINT('Ctrl Pts',(5.58257927845958,-3.01965681102916,17.5553228306677));
#8196=CARTESIAN_POINT('Ctrl Pts',(5.55206995970538,-3.0308379415139,17.557329289839));
#8197=CARTESIAN_POINT('Ctrl Pts',(5.53868305267685,-3.03564372782525,17.5582045935896));
#8198=CARTESIAN_POINT('Ctrl Pts',(5.51114686843535,-3.04532368080307,17.5599948007428));
#8199=CARTESIAN_POINT('Ctrl Pts',(5.4969945618617,-3.05018823861609,17.5609093681771));
#8200=CARTESIAN_POINT('Ctrl Pts',(5.46093768559787,-3.06230187379469,17.5632257896918));
#8201=CARTESIAN_POINT('Ctrl Pts',(5.43898797996414,-3.06941469963751,17.5646231405301));
#8202=CARTESIAN_POINT('Ctrl Pts',(5.35428866523754,-3.09585992022371,17.569968181992));
#8203=CARTESIAN_POINT('Ctrl Pts',(5.29102773750733,-3.11350949590961,17.5738611954626));
#8204=CARTESIAN_POINT('Ctrl Pts',(4.90278901022853,-3.20914181941009,17.597248442036));
#8205=CARTESIAN_POINT('Ctrl Pts',(4.56790416102437,-3.23810679314254,17.6150524391799));
#8206=CARTESIAN_POINT('Ctrl Pts',(4.18792085897161,-3.21188209951904,17.637171667383));
#8207=CARTESIAN_POINT('Ctrl Pts',(4.14134200844061,-3.20764699781071,17.6399205202443));
#8208=CARTESIAN_POINT('Ctrl Pts',(4.06415002123486,-3.19893096325816,17.6445623167685));
#8209=CARTESIAN_POINT('Ctrl Pts',(4.03347865215829,-3.19501995107382,17.6464294604565));
#8210=CARTESIAN_POINT('Ctrl Pts',(3.99125406113507,-3.18901711692318,17.6490372343265));
#8211=CARTESIAN_POINT('Ctrl Pts',(3.97964783001051,-3.18730241283627,17.649757934463));
#8212=CARTESIAN_POINT('Ctrl Pts',(3.96005437429916,-3.18429826378558,17.650981602362));
#8213=CARTESIAN_POINT('Ctrl Pts',(3.9520620295563,-3.18304202266579,17.6514827184227));
#8214=CARTESIAN_POINT('Ctrl Pts',(3.93676652502225,-3.18057881238802,17.6524456554492));
#8215=CARTESIAN_POINT('Ctrl Pts',(3.92946266984737,-3.1793767578132,17.6529071784147));
#8216=CARTESIAN_POINT('Ctrl Pts',(3.91198415150622,-3.17643829409671,17.654015605431));
#8217=CARTESIAN_POINT('Ctrl Pts',(3.90181363655509,-3.17467815774732,17.6546638163495));
#8218=CARTESIAN_POINT('Ctrl Pts',(3.86512649035585,-3.1681473084216,17.6570132941445));
#8219=CARTESIAN_POINT('Ctrl Pts',(3.83866231254647,-3.16309312426167,17.6587293245425));
#8220=CARTESIAN_POINT('Ctrl Pts',(3.64138543984744,-3.12284670258013,17.671664996519));
#8221=CARTESIAN_POINT('Ctrl Pts',(3.47363262213271,-3.07417535280573,17.6834558230224));
#8222=CARTESIAN_POINT('Ctrl Pts',(3.14246145812883,-2.94820029907648,17.7074269182828));
#8223=CARTESIAN_POINT('Ctrl Pts',(2.97990245470859,-2.87023775754521,17.7195606389978));
#8224=CARTESIAN_POINT('Ctrl Pts',(2.77201839537422,-2.74817651579871,17.7352757873257));
#8225=CARTESIAN_POINT('Ctrl Pts',(2.72023385177468,-2.71575703577067,17.7392110544193));
#8226=CARTESIAN_POINT('Ctrl Pts',(2.63262073791459,-2.6573761422031,17.7459042697384));
#8227=CARTESIAN_POINT('Ctrl Pts',(2.59634885542461,-2.63211394047536,17.7486862558223));
#8228=CARTESIAN_POINT('Ctrl Pts',(2.5450859248808,-2.59482181831947,17.7526358336519));
#8229=CARTESIAN_POINT('Ctrl Pts',(2.52966618264017,-2.58339243127525,17.7538262466253));
#8230=CARTESIAN_POINT('Ctrl Pts',(2.50301939509041,-2.56327005079055,17.7558878869497));
#8231=CARTESIAN_POINT('Ctrl Pts',(2.49174611659163,-2.55463944842961,17.7567615147971));
#8232=CARTESIAN_POINT('Ctrl Pts',(2.46866660798003,-2.53672708615607,17.7585531931258));
#8233=CARTESIAN_POINT('Ctrl Pts',(2.45686746986413,-2.52743672314683,17.7594708740152));
#8234=CARTESIAN_POINT('Ctrl Pts',(2.4269151950109,-2.50351196458591,17.7618050976878));
#8235=CARTESIAN_POINT('Ctrl Pts',(2.40885495882912,-2.48876225913214,17.7632169956674));
#8236=CARTESIAN_POINT('Ctrl Pts',(2.33911369912581,-2.43053181889291,17.7686886278154));
#8237=CARTESIAN_POINT('Ctrl Pts',(2.2886424201401,-2.38562512967248,17.7726902158919));
#8238=CARTESIAN_POINT('Ctrl Pts',(1.99869771392132,-2.11084112312122,17.7960321724947));
#8239=CARTESIAN_POINT('Ctrl Pts',(1.79453086865377,-1.84670966079781,17.8137236163597));
#8240=CARTESIAN_POINT('Ctrl Pts',(1.61175235161855,-1.51521716828888,17.8357084465921));
#8241=CARTESIAN_POINT('Ctrl Pts',(1.59010546486741,-1.47385736307143,17.8384522625202));
#8242=CARTESIAN_POINT('Ctrl Pts',(1.55564563536271,-1.40438387922067,17.8430863442203));
#8243=CARTESIAN_POINT('Ctrl Pts',(1.54232452801917,-1.37652900700457,17.8449509196504));
#8244=CARTESIAN_POINT('Ctrl Pts',(1.52449979469413,-1.33783818730869,17.8475556761839));
#8245=CARTESIAN_POINT('Ctrl Pts',(1.51965160308294,-1.32716163392025,17.8482759875876));
#8246=CARTESIAN_POINT('Ctrl Pts',(1.51155750145409,-1.30907548998749,17.8494991884379));
#8247=CARTESIAN_POINT('Ctrl Pts',(1.50828096963643,-1.30167957190674,17.8500002294915));
#8248=CARTESIAN_POINT('Ctrl Pts',(1.50205903236507,-1.28749116139494,17.8509631795987));
#8249=CARTESIAN_POINT('Ctrl Pts',(1.4991091378223,-1.28070074173037,17.8514247916337));
#8250=CARTESIAN_POINT('Ctrl Pts',(1.49210058904709,-1.26441429320765,17.8525336407789));
#8251=CARTESIAN_POINT('Ctrl Pts',(1.4880641595107,-1.25490887159543,17.8531821869194));
#8252=CARTESIAN_POINT('Ctrl Pts',(1.47364702426217,-1.22049907019421,17.8555344705486));
#8253=CARTESIAN_POINT('Ctrl Pts',(1.46353381447304,-1.19548474761618,17.8572530177058));
#8254=CARTESIAN_POINT('Ctrl Pts',(1.39346545725631,-1.01571200390295,17.8696497279452));
#8255=CARTESIAN_POINT('Ctrl Pts',(1.34523547499512,-0.856666250735065,17.8808458304981));
#8256=CARTESIAN_POINT('Ctrl Pts',(1.27555594069633,-0.540986327088179,17.9027136101999));
#8257=CARTESIAN_POINT('Ctrl Pts',(1.25293717047129,-0.385051760889612,17.9133527290673));
#8258=CARTESIAN_POINT('Ctrl Pts',(1.2333471343102,-0.108940420664665,17.9315949290285));
#8259=CARTESIAN_POINT('Ctrl Pts',(1.23152306440408,0.0105874729040621,17.9393014113896));
#8260=CARTESIAN_POINT('Ctrl Pts',(1.23743273313204,0.157023417474341,17.9485039317567));
#8261=CARTESIAN_POINT('Ctrl Pts',(1.23886649681224,0.184078909287284,17.9501944273286));
#8262=CARTESIAN_POINT('Ctrl Pts',(1.24167900192721,0.22692088750235,17.9528564762268));
#8263=CARTESIAN_POINT('Ctrl Pts',(1.24283325991198,0.242720344189877,17.9538350008638));
#8264=CARTESIAN_POINT('Ctrl Pts',(1.24522468973586,0.272437259254777,17.955669675151));
#8265=CARTESIAN_POINT('Ctrl Pts',(1.2464359603021,0.286356376670746,17.956526614417));
#8266=CARTESIAN_POINT('Ctrl Pts',(1.24936786985855,0.317687489166557,17.9584503135568));
#8267=CARTESIAN_POINT('Ctrl Pts',(1.25113987271493,0.33509432203065,17.9595154378778));
#8268=CARTESIAN_POINT('Ctrl Pts',(1.2560454368601,0.379676389091274,17.9622345930253));
#8269=CARTESIAN_POINT('Ctrl Pts',(1.2593834291921,0.406828055700854,17.963882203253));
#8270=CARTESIAN_POINT('Ctrl Pts',(1.29053669609954,0.636090529680842,17.9777305180821));
#8271=CARTESIAN_POINT('Ctrl Pts',(1.33714061063732,0.835191021539577,17.9892963366749));
#8272=CARTESIAN_POINT('Ctrl Pts',(1.45920127007577,1.1976340710183,18.0107191484895));
#8273=CARTESIAN_POINT('Ctrl Pts',(1.53007234596313,1.36166624933642,18.0205835818753));
#8274=CARTESIAN_POINT('Ctrl Pts',(1.63711278150622,1.56196110220808,18.033749924833));
#8275=CARTESIAN_POINT('Ctrl Pts',(1.66105345875509,1.60441373940812,18.0366101428136));
#8276=CARTESIAN_POINT('Ctrl Pts',(1.70222774360734,1.67370484823327,18.041422128217));
#8277=CARTESIAN_POINT('Ctrl Pts',(1.71891419068282,1.70086046234113,18.0433456105338));
#8278=CARTESIAN_POINT('Ctrl Pts',(1.74236458308648,1.73778454982884,18.0460194931395));
#8279=CARTESIAN_POINT('Ctrl Pts',(1.7487844834652,1.74777071653791,18.0467486167704));
#8280=CARTESIAN_POINT('Ctrl Pts',(1.75968706003402,1.76452544993902,18.0479824264597));
#8281=CARTESIAN_POINT('Ctrl Pts',(1.76414048133063,1.77131308403381,18.0484851887683));
#8282=CARTESIAN_POINT('Ctrl Pts',(1.77268758470191,1.7842333575583,18.0494479351513));
#8283=CARTESIAN_POINT('Ctrl Pts',(1.77677674311759,1.79036889104188,18.0499076003301));
#8284=CARTESIAN_POINT('Ctrl Pts',(1.78657916328238,1.80496801343385,18.0510071675534));
#8285=CARTESIAN_POINT('Ctrl Pts',(1.79231162628024,1.81341852654092,18.0516483311739));
#8286=CARTESIAN_POINT('Ctrl Pts',(1.81289648258903,1.84345542798716,18.0539436907664));
#8287=CARTESIAN_POINT('Ctrl Pts',(1.82797140842111,1.86488709641623,18.0556117910376));
#8288=CARTESIAN_POINT('Ctrl Pts',(1.96077779876963,2.04888529092708,18.0701813412165));
#8289=CARTESIAN_POINT('Ctrl Pts',(2.09318804749009,2.2002944137908,18.0838390809187));
#8290=CARTESIAN_POINT('Ctrl Pts',(2.35581890646096,2.44936598455359,18.108308221133));
#8291=CARTESIAN_POINT('Ctrl Pts',(2.48100889545633,2.55140980236907,18.1191227658204));
#8292=CARTESIAN_POINT('Ctrl Pts',(2.66045001376294,2.67651513657042,18.1333472322813));
#8293=CARTESIAN_POINT('Ctrl Pts',(2.70844767165986,2.70810627057053,18.1370410058114));
#8294=CARTESIAN_POINT('Ctrl Pts',(2.79309806424371,2.76063263788371,18.1433661548506));
#8295=CARTESIAN_POINT('Ctrl Pts',(2.82936362209553,2.78216171327825,18.1460181919573));
#8296=CARTESIAN_POINT('Ctrl Pts',(2.88242826343463,2.81227095310713,18.1498178017836));
#8297=CARTESIAN_POINT('Ctrl Pts',(2.89889530364076,2.82142452710083,18.1509858758511));
#8298=CARTESIAN_POINT('Ctrl Pts',(2.92786111434785,2.83719493948615,18.1530216300262));
#8299=CARTESIAN_POINT('Ctrl Pts',(2.94032480097321,2.84387481673461,18.1538915391528));
#8300=CARTESIAN_POINT('Ctrl Pts',(2.96460580694255,2.856683155031,18.155574697084));
#8301=CARTESIAN_POINT('Ctrl Pts',(2.9764179060678,2.86282084756358,18.1563882592165));
#8302=CARTESIAN_POINT('Ctrl Pts',(3.00807495259627,2.87902188451017,18.1585548810051));
#8303=CARTESIAN_POINT('Ctrl Pts',(3.02798688440838,2.88895330800317,18.1599033056961));
#8304=CARTESIAN_POINT('Ctrl Pts',(3.10176861641895,2.92480387814324,18.1648487421524));
#8305=CARTESIAN_POINT('Ctrl Pts',(3.15625558582648,2.94942988063635,18.168401227318));
#8306=CARTESIAN_POINT('Ctrl Pts',(3.52629583588521,3.10442464018978,18.1919431062201));
#8307=CARTESIAN_POINT('Ctrl Pts',(3.86009815043818,3.18543169748073,18.2101076606996));
#8308=CARTESIAN_POINT('Ctrl Pts',(4.24725345507066,3.21629586340303,18.2326569091821));
#8309=CARTESIAN_POINT('Ctrl Pts',(4.29421804560129,3.21900674499806,18.2354211642744));
#8310=CARTESIAN_POINT('Ctrl Pts',(4.37225484965584,3.22179914761503,18.2400865422355));
#8311=CARTESIAN_POINT('Ctrl Pts',(4.40330010815037,3.22246096704296,18.2419615284009));
#8312=CARTESIAN_POINT('Ctrl Pts',(4.44610043648753,3.22275474736778,18.2445785140417));
#8313=CARTESIAN_POINT('Ctrl Pts',(4.45785225870054,3.22277112869508,18.2453003986375));
#8314=CARTESIAN_POINT('Ctrl Pts',(4.47769799622732,3.22269024504698,18.2465254901713));
#8315=CARTESIAN_POINT('Ctrl Pts',(4.48579207778506,3.22262676132734,18.2470268353177));
#8316=CARTESIAN_POINT('Ctrl Pts',(4.50128328850569,3.22244689358093,18.2479897348765));
#8317=CARTESIAN_POINT('Ctrl Pts',(4.50868038289312,3.22233553076978,18.2484509883077));
#8318=CARTESIAN_POINT('Ctrl Pts',(4.52638107799941,3.22200808352567,18.2495581365008));
#8319=CARTESIAN_POINT('Ctrl Pts',(4.53668407920401,3.22176804339415,18.2502053315818));
#8320=CARTESIAN_POINT('Ctrl Pts',(4.57380187564839,3.22072511475752,18.2525464466231));
#8321=CARTESIAN_POINT('Ctrl Pts',(4.6006067126288,3.21963685611386,18.2542549934808));
#8322=CARTESIAN_POINT('Ctrl Pts',(4.80916559087941,3.20855994778415,18.2676719831817));
#8323=CARTESIAN_POINT('Ctrl Pts',(4.98977627395893,3.18352372355826,18.2800022053041));
#8324=CARTESIAN_POINT('Ctrl Pts',(5.33736362501278,3.10492298519491,18.3041104649829));
#8325=CARTESIAN_POINT('Ctrl Pts',(5.50405278947946,3.05272046722543,18.3158488470475));
#8326=CARTESIAN_POINT('Ctrl Pts',(5.74974893418431,2.95326330277609,18.3331158729495));
#8327=CARTESIAN_POINT('Ctrl Pts',(5.83231819952626,2.91571238762201,18.338916852701));
#8328=CARTESIAN_POINT('Ctrl Pts',(5.93546206766403,2.86344551062101,18.3461639569532));
#8329=CARTESIAN_POINT('Ctrl Pts',(5.95759191940309,2.85190650764038,18.3477190117708));
#8330=CARTESIAN_POINT('Ctrl Pts',(5.99313477734857,2.83284530850656,18.3502174052531));
#8331=CARTESIAN_POINT('Ctrl Pts',(6.00663155622794,2.82548231606796,18.3511663209502));
#8332=CARTESIAN_POINT('Ctrl Pts',(6.03237465478157,2.81119851853907,18.3529768058081));
#8333=CARTESIAN_POINT('Ctrl Pts',(6.04462933227762,2.80429358571775,18.353838914319));
#8334=CARTESIAN_POINT('Ctrl Pts',(6.07247998116988,2.78835993841448,18.3557989695407));
#8335=CARTESIAN_POINT('Ctrl Pts',(6.08804630553277,2.77928015091319,18.3568950488875));
#8336=CARTESIAN_POINT('Ctrl Pts',(6.1368385592051,2.75026857462006,18.3603331596537));
#8337=CARTESIAN_POINT('Ctrl Pts',(6.16978242951311,2.72986746585732,18.3626581336002));
#8338=CARTESIAN_POINT('Ctrl Pts',(6.42599016402845,2.56474049801035,18.3807897360878));
#8339=CARTESIAN_POINT('Ctrl Pts',(6.6309173361166,2.39346940108887,18.3954839606383));
#8340=CARTESIAN_POINT('Ctrl Pts',(6.92775042164736,2.07543469982288,18.419876075711));
#8341=CARTESIAN_POINT('Ctrl Pts',(7.0331205750862,1.94306779650924,18.4294342190971));
#8342=CARTESIAN_POINT('Ctrl Pts',(7.13875264781814,1.78658014987017,18.440845502285));
#8343=CARTESIAN_POINT('Ctrl Pts',(7.14973381822924,1.76998270475036,18.44205722001));
#8344=CARTESIAN_POINT('Ctrl Pts',(7.16591065360235,1.74503317587486,18.4438824795525));
#8345=CARTESIAN_POINT('Ctrl Pts',(7.17122317378577,1.73675692895483,18.4444885692249));
#8346=CARTESIAN_POINT('Ctrl Pts',(7.18028893838699,1.72249036412953,18.4455346341585));
#8347=CARTESIAN_POINT('Ctrl Pts',(7.18406047435073,1.71651182919033,18.4459733918043));
#8348=CARTESIAN_POINT('Ctrl Pts',(7.19262104145066,1.70284239772997,18.4469775238051));
#8349=CARTESIAN_POINT('Ctrl Pts',(7.19739724115002,1.69514382828959,18.4475437068857));
#8350=CARTESIAN_POINT('Ctrl Pts',(7.21039331357081,1.67399744150392,18.4491004764101));
#8351=CARTESIAN_POINT('Ctrl Pts',(7.21854697087583,1.66050950616903,18.4500951823816));
#8352=CARTESIAN_POINT('Ctrl Pts',(7.25990987014407,1.59093859332788,18.4552326238555));
#8353=CARTESIAN_POINT('Ctrl Pts',(7.29150885086439,1.53392113941218,18.4594651813617));
#8354=CARTESIAN_POINT('Ctrl Pts',(7.33699852857038,1.44562598211644,18.4660095916498));
#8355=CARTESIAN_POINT('Ctrl Pts',(7.35215779216634,1.41501630349278,18.4682766470177));
#8356=CARTESIAN_POINT('Ctrl Pts',(7.48610796830902,1.13337291816072,18.4890865528718));
#8357=CARTESIAN_POINT('Ctrl Pts',(7.57249072918749,0.868155303675707,18.5081892131244));
#8358=CARTESIAN_POINT('Ctrl Pts',(7.64009809065663,0.508352915344718,18.5320130836027));
#8359=CARTESIAN_POINT('Ctrl Pts',(7.65283313618465,0.420922318484652,18.5376596092375));
#8360=CARTESIAN_POINT('Ctrl Pts',(7.66451877335594,0.308459403168151,18.5447447508743));
#8361=CARTESIAN_POINT('Ctrl Pts',(7.66679266168259,0.283817889359796,18.5462864146476));
#8362=CARTESIAN_POINT('Ctrl Pts',(7.67001513608912,0.243873782052595,18.548768613953));
#8363=CARTESIAN_POINT('Ctrl Pts',(7.67113870729234,0.228586693745645,18.5497145953185));
#8364=CARTESIAN_POINT('Ctrl Pts',(7.67308499922083,0.199243534041357,18.5515229323804));
#8365=CARTESIAN_POINT('Ctrl Pts',(7.67392475307572,0.185188982965779,18.552385801271));
#8366=CARTESIAN_POINT('Ctrl Pts',(7.67563430860804,0.153039605947283,18.5543523147175));
#8367=CARTESIAN_POINT('Ctrl Pts',(7.67644370459281,0.134941942603784,18.5554540476084));
#8368=CARTESIAN_POINT('Ctrl Pts',(7.67852384032242,0.0776032069004583,18.5589287054524));
#8369=CARTESIAN_POINT('Ctrl Pts',(7.67923017083788,0.0383443493416745,18.5612840410069));
#8370=CARTESIAN_POINT('Ctrl Pts',(7.67921897520336,-0.000918943050559805,
18.563618782904));
#8371=CARTESIAN_POINT('',(7.67921766478722,0.00291592938798334,18.3138092652699));
#8372=CARTESIAN_POINT('Ctrl Pts',(7.67921910621823,-1.45987529487438E-10,
18.3139723139554));
#8373=CARTESIAN_POINT('Ctrl Pts',(7.67921910621828,0.000972342785896192,
18.3139178708026));
#8374=CARTESIAN_POINT('Ctrl Pts',(7.67921866616676,0.00194469629559445,
18.3138634295123));
#8375=CARTESIAN_POINT('Ctrl Pts',(7.67921778603496,0.00291706008692861,
18.3138089900028));
#8376=CARTESIAN_POINT('Ctrl Pts',(7.67921778706881,0.00291591766745765,
18.3138090539631));
#8377=CARTESIAN_POINT('Ctrl Pts',(7.67902220457112,0.219078823587967,18.3017067902972));
#8378=CARTESIAN_POINT('Ctrl Pts',(7.65707889795432,0.434655820836481,18.2897863540716));
#8379=CARTESIAN_POINT('Ctrl Pts',(7.60880514919697,0.670446050244141,18.2754737311236));
#8380=CARTESIAN_POINT('Ctrl Pts',(7.60360584464707,0.694442732277932,18.2740017270286));
#8381=CARTESIAN_POINT('Ctrl Pts',(7.59513947807702,0.731468530665847,18.2717033529349));
#8382=CARTESIAN_POINT('Ctrl Pts',(7.59206418507794,0.744541068146832,18.2708866133773));
#8383=CARTESIAN_POINT('Ctrl Pts',(7.58614991284442,0.768994929362721,18.2693482721318));
#8384=CARTESIAN_POINT('Ctrl Pts',(7.58333031306333,0.780380763472973,18.2686277203827));
#8385=CARTESIAN_POINT('Ctrl Pts',(7.57846130622866,0.799592210917159,18.2674042705642));
#8386=CARTESIAN_POINT('Ctrl Pts',(7.57644444096982,0.807426101546395,18.2669032232013));
#8387=CARTESIAN_POINT('Ctrl Pts',(7.57252575545191,0.822413098394386,18.2659403930044));
#8388=CARTESIAN_POINT('Ctrl Pts',(7.57062875634282,0.829567367105543,18.2654789079425));
#8389=CARTESIAN_POINT('Ctrl Pts',(7.56602742070546,0.846682457257635,18.2643705415024));
#8390=CARTESIAN_POINT('Ctrl Pts',(7.56329986360912,0.85663687332996,18.2637223532187));
#8391=CARTESIAN_POINT('Ctrl Pts',(7.55327919942814,0.892530587111473,18.2613727282853));
#8392=CARTESIAN_POINT('Ctrl Pts',(7.5457088918796,0.918390460999878,18.2596565244853));
#8393=CARTESIAN_POINT('Ctrl Pts',(7.48794461673195,1.10691080639361,18.246988664533));
#8394=CARTESIAN_POINT('Ctrl Pts',(7.42526105832655,1.26544805290942,18.2354923274378));
#8395=CARTESIAN_POINT('Ctrl Pts',(7.29434462630614,1.53257348785622,18.2153676248116));
#8396=CARTESIAN_POINT('Ctrl Pts',(7.23160392027629,1.64345636269755,18.206761026444));
#8397=CARTESIAN_POINT('Ctrl Pts',(7.08615438131089,1.86831876536636,18.1889721971483));
#8398=CARTESIAN_POINT('Ctrl Pts',(7.00220115682713,1.98119085147181,18.1798438399361));
#8399=CARTESIAN_POINT('Ctrl Pts',(6.89244629127531,2.11020489532854,18.1691845424563));
#8400=CARTESIAN_POINT('Ctrl Pts',(6.87346167709424,2.13192320349972,18.1673814204658));
#8401=CARTESIAN_POINT('Ctrl Pts',(6.84505988469014,2.16354761042593,18.1647421610638));
#8402=CARTESIAN_POINT('Ctrl Pts',(6.83586759705272,2.17365291631261,18.1638966949583));
#8403=CARTESIAN_POINT('Ctrl Pts',(6.81709601361245,2.19402720247581,18.1621876219829));
#8404=CARTESIAN_POINT('Ctrl Pts',(6.80751328993501,2.20429263421184,18.1613241877605));
#8405=CARTESIAN_POINT('Ctrl Pts',(6.78724524961101,2.22572211320399,18.1595166326087));
#8406=CARTESIAN_POINT('Ctrl Pts',(6.77654609366499,2.23687262515404,18.15857313812));
#8407=CARTESIAN_POINT('Ctrl Pts',(6.74810491163968,2.26609003721838,18.1560927149251));
#8408=CARTESIAN_POINT('Ctrl Pts',(6.73022922821239,2.28402576273897,18.1545616513924));
#8409=CARTESIAN_POINT('Ctrl Pts',(6.65155945073906,2.36112078272651,18.1479405916881));
#8410=CARTESIAN_POINT('Ctrl Pts',(6.58865157296379,2.4180803777475,18.1429457569334));
#8411=CARTESIAN_POINT('Ctrl Pts',(6.31176948151111,2.64956388523367,18.1220375232401));
#8412=CARTESIAN_POINT('Ctrl Pts',(6.07811950043421,2.7986724024515,18.10708729565));
#8413=CARTESIAN_POINT('Ctrl Pts',(5.73727478898837,2.95901699600314,18.0855554388898));
#8414=CARTESIAN_POINT('Ctrl Pts',(5.64426619493235,2.99756213033704,18.0796916195761));
#8415=CARTESIAN_POINT('Ctrl Pts',(5.53311088446696,3.03764183810505,18.0725292580392));
#8416=CARTESIAN_POINT('Ctrl Pts',(5.5165563622763,3.04345863011925,18.0714586069918));
#8417=CARTESIAN_POINT('Ctrl Pts',(5.49110846461714,3.05216749199089,18.0698055558867));
#8418=CARTESIAN_POINT('Ctrl Pts',(5.48224833056234,3.05515662100498,18.0692286815634));
#8419=CARTESIAN_POINT('Ctrl Pts',(5.46595113524696,3.06057589529458,18.0681649226179));
#8420=CARTESIAN_POINT('Ctrl Pts',(5.4585181170781,3.06301755688028,18.0676787194975));
#8421=CARTESIAN_POINT('Ctrl Pts',(5.44169634814991,3.06847553180218,18.0665760672837));
#8422=CARTESIAN_POINT('Ctrl Pts',(5.43230266207107,3.07147581347142,18.0659587119084));
#8423=CARTESIAN_POINT('Ctrl Pts',(5.40797556983524,3.07912286413166,18.0643560486737));
#8424=CARTESIAN_POINT('Ctrl Pts',(5.39302203928985,3.08370406225967,18.0633671444802));
#8425=CARTESIAN_POINT('Ctrl Pts',(5.2939231292201,3.11327694979502,18.0567914066732));
#8426=CARTESIAN_POINT('Ctrl Pts',(5.20882724713966,3.13492854096393,18.0510403580686));
#8427=CARTESIAN_POINT('Ctrl Pts',(4.84349384724895,3.21215221840393,18.0261977317667));
#8428=CARTESIAN_POINT('Ctrl Pts',(4.55735162783163,3.2338171590074,18.0065091569289));
#8429=CARTESIAN_POINT('Ctrl Pts',(4.18289842369977,3.21236057737842,17.9820903032113));
#8430=CARTESIAN_POINT('Ctrl Pts',(4.09393743207977,3.20354095965228,17.9763753043247));
#8431=CARTESIAN_POINT('Ctrl Pts',(3.9808574037683,3.187558310022,17.9692183985274));
#8432=CARTESIAN_POINT('Ctrl Pts',(3.95630465989973,3.18379805474869,17.9676708537229));
#8433=CARTESIAN_POINT('Ctrl Pts',(3.91665490350325,3.17725569056913,17.9651816097251));
#8434=CARTESIAN_POINT('Ctrl Pts',(3.90153036724323,3.17464897361847,17.9642344067374));
#8435=CARTESIAN_POINT('Ctrl Pts',(3.87257519088137,3.16944529300161,17.9624253061553));
#8436=CARTESIAN_POINT('Ctrl Pts',(3.85874184493001,3.16686559562092,17.9615628836103));
#8437=CARTESIAN_POINT('Ctrl Pts',(3.82718417983331,3.1607664515855,17.9595995422138));
#8438=CARTESIAN_POINT('Ctrl Pts',(3.80947157588261,3.15718835301531,17.9585005143452));
#8439=CARTESIAN_POINT('Ctrl Pts',(3.75360868578368,3.14541370073778,17.9550429803124));
#8440=CARTESIAN_POINT('Ctrl Pts',(3.71557579329625,3.13667298521232,17.9527018148995));
#8441=CARTESIAN_POINT('Ctrl Pts',(3.42213901394682,3.063600118789,17.9347170930903));
#8442=CARTESIAN_POINT('Ctrl Pts',(3.17533609678247,2.96887128092349,17.9201593579953));
#8443=CARTESIAN_POINT('Ctrl Pts',(2.83596270779622,2.78831852162408,17.8986121307256));
#8444=CARTESIAN_POINT('Ctrl Pts',(2.73242371016655,2.72551360085741,17.8917844149911));
#8445=CARTESIAN_POINT('Ctrl Pts',(2.60022057258223,2.63476904710498,17.8824082052472));
#8446=CARTESIAN_POINT('Ctrl Pts',(2.56818412795226,2.61190469154603,17.8800812907266));
#8447=CARTESIAN_POINT('Ctrl Pts',(2.5147440117586,2.57226749424362,17.8760913002418));
#8448=CARTESIAN_POINT('Ctrl Pts',(2.49311870978285,2.55579958414268,17.8744456716623));
#8449=CARTESIAN_POINT('Ctrl Pts',(2.46292076423575,2.53219408545717,17.872099464602));
#8450=CARTESIAN_POINT('Ctrl Pts',(2.45417226063277,2.52528200640435,17.8714139445679));
#8451=CARTESIAN_POINT('Ctrl Pts',(2.43922269831306,2.51334402810182,17.8702321644941));
#8452=CARTESIAN_POINT('Ctrl Pts',(2.43300402619923,2.50834015688915,17.8697374624734));
#8453=CARTESIAN_POINT('Ctrl Pts',(2.42094245123594,2.49856073438672,17.8687717638766));
#8454=CARTESIAN_POINT('Ctrl Pts',(2.41509767778883,2.49378772051554,17.8683009701457));
#8455=CARTESIAN_POINT('Ctrl Pts',(2.39915331634107,2.48067347350706,17.8670090030699));
#8456=CARTESIAN_POINT('Ctrl Pts',(2.38908786531271,2.47229123131293,17.8661849455991));
#8457=CARTESIAN_POINT('Ctrl Pts',(2.35020441156416,2.43950662138524,17.8629695050356));
#8458=CARTESIAN_POINT('Ctrl Pts',(2.32176630714562,2.41466088535133,17.86054888641));
#8459=CARTESIAN_POINT('Ctrl Pts',(2.13208175656911,2.24296783296895,17.8439673343767));
#8460=CARTESIAN_POINT('Ctrl Pts',(1.98567366264413,2.08058705567431,17.8290320257688));
#8461=CARTESIAN_POINT('Ctrl Pts',(1.7752746792486,1.79341521202182,17.8050485566151));
#8462=CARTESIAN_POINT('Ctrl Pts',(1.70097776999226,1.67702597657883,17.79586790053));
#8463=CARTESIAN_POINT('Ctrl Pts',(1.59632712291983,1.48724895090778,17.7818272118218));
#8464=CARTESIAN_POINT('Ctrl Pts',(1.56083122172959,1.41689963434564,17.7768060278843));
#8465=CARTESIAN_POINT('Ctrl Pts',(1.51800495768735,1.32367411810515,17.7703829241998));
#8466=CARTESIAN_POINT('Ctrl Pts',(1.50830346973981,1.30192325116869,17.7689001576579));
#8467=CARTESIAN_POINT('Ctrl Pts',(1.49283651507568,1.26618646566647,17.7664892402141));
#8468=CARTESIAN_POINT('Ctrl Pts',(1.48692696672514,1.25226426737094,17.7655562060874));
#8469=CARTESIAN_POINT('Ctrl Pts',(1.47567917383837,1.22523839398297,17.7637567709461));
#8470=CARTESIAN_POINT('Ctrl Pts',(1.4703287970387,1.21214017631349,17.7628899753721));
#8471=CARTESIAN_POINT('Ctrl Pts',(1.45815513908929,1.18176809877748,17.7608920834409));
#8472=CARTESIAN_POINT('Ctrl Pts',(1.45139453105396,1.1644695379604,17.7597631140323));
#8473=CARTESIAN_POINT('Ctrl Pts',(1.4299005674612,1.10803826772325,17.7561083681613));
#8474=CARTESIAN_POINT('Ctrl Pts',(1.41577879806514,1.06867610361099,17.7536029297105));
#8475=CARTESIAN_POINT('Ctrl Pts',(1.33882591074292,0.840292977266851,17.7392969084463));
#8476=CARTESIAN_POINT('Ctrl Pts',(1.29285791951042,0.646040299189059,17.7280666575537));
#8477=CARTESIAN_POINT('Ctrl Pts',(1.24177440756993,0.282766235200084,17.7075407972883));
#8478=CARTESIAN_POINT('Ctrl Pts',(1.23142063369164,0.115209047531944,17.6982406204294));
#8479=CARTESIAN_POINT('Ctrl Pts',(1.23491218439861,-0.099588574865565,17.6857698812959));
#8480=CARTESIAN_POINT('Ctrl Pts',(1.23671692944911,-0.146773165160949,17.6829956328373));
#8481=CARTESIAN_POINT('Ctrl Pts',(1.2414307941622,-0.224979417776491,17.6783150012011));
#8482=CARTESIAN_POINT('Ctrl Pts',(1.24375444266111,-0.256030102910681,17.6764349754495));
#8483=CARTESIAN_POINT('Ctrl Pts',(1.24757526952819,-0.298757917447027,17.6738121190046));
#8484=CARTESIAN_POINT('Ctrl Pts',(1.24868716037419,-0.310468881436922,17.6730895229081));
#8485=CARTESIAN_POINT('Ctrl Pts',(1.25067247219531,-0.330228784207575,17.6718636154967));
#8486=CARTESIAN_POINT('Ctrl Pts',(1.25151216779087,-0.33828113992184,17.671362172308));
#8487=CARTESIAN_POINT('Ctrl Pts',(1.25317682238448,-0.353681754737367,17.6703994048724));
#8488=CARTESIAN_POINT('Ctrl Pts',(1.25399674267614,-0.361030466090661,17.6699383835343));
#8489=CARTESIAN_POINT('Ctrl Pts',(1.25601859844113,-0.378602796511614,17.6688322184066));
#8490=CARTESIAN_POINT('Ctrl Pts',(1.25724423375604,-0.388823531853105,17.6681857789811));
#8491=CARTESIAN_POINT('Ctrl Pts',(1.26183070545722,-0.425580198028187,17.6658504379682));
#8492=CARTESIAN_POINT('Ctrl Pts',(1.26547280382327,-0.452079093527858,17.6641470018324));
#8493=CARTESIAN_POINT('Ctrl Pts',(1.29707206589123,-0.662531810227149,17.6504766306551));
#8494=CARTESIAN_POINT('Ctrl Pts',(1.34058069505014,-0.843780325644675,17.6378602622274));
#8495=CARTESIAN_POINT('Ctrl Pts',(1.45375320281548,-1.18288293458307,17.6136778585585));
#8496=CARTESIAN_POINT('Ctrl Pts',(1.52092979962837,-1.34094567840818,17.6021452578269));
#8497=CARTESIAN_POINT('Ctrl Pts',(1.62792381585929,-1.5456346646578,17.5871051655424));
#8498=CARTESIAN_POINT('Ctrl Pts',(1.65693103694159,-1.59757387770947,17.583276644109));
#8499=CARTESIAN_POINT('Ctrl Pts',(1.70951460006085,-1.68589259241211,17.5767457805));
#8500=CARTESIAN_POINT('Ctrl Pts',(1.73241700917572,-1.72265299977992,17.574020923687));
#8501=CARTESIAN_POINT('Ctrl Pts',(1.76644492888785,-1.77489434223392,17.5701372479022));
#8502=CARTESIAN_POINT('Ctrl Pts',(1.77697688180983,-1.79075443458514,17.5689566412206));
#8503=CARTESIAN_POINT('Ctrl Pts',(1.79559236605462,-1.81825557749611,17.5669064672318));
#8504=CARTESIAN_POINT('Ctrl Pts',(1.80361320342808,-1.82993823411243,17.5660345744349));
#8505=CARTESIAN_POINT('Ctrl Pts',(1.82032296617973,-1.8539358748889,17.5642414173779));
#8506=CARTESIAN_POINT('Ctrl Pts',(1.82902175739814,-1.86624359104744,17.5633205572675));
#8507=CARTESIAN_POINT('Ctrl Pts',(1.8515456418621,-1.89764245389676,17.5609679044192));
#8508=CARTESIAN_POINT('Ctrl Pts',(1.86549457261731,-1.91664398086319,17.5595409055754));
#8509=CARTESIAN_POINT('Ctrl Pts',(1.92137920327115,-1.99104604014653,17.553938313669));
#8510=CARTESIAN_POINT('Ctrl Pts',(1.96489507265508,-2.04523960035997,17.549824562917));
#8511=CARTESIAN_POINT('Ctrl Pts',(2.22469752876772,-2.34817975736258,17.5265287183775));
#8512=CARTESIAN_POINT('Ctrl Pts',(2.47633822250584,-2.56394151868802,17.5089533273866));
#8513=CARTESIAN_POINT('Ctrl Pts',(2.79586405862106,-2.76236828748259,17.4871071519419));
#8514=CARTESIAN_POINT('Ctrl Pts',(2.83596485755118,-2.7860820577079,17.4843686844615));
#8515=CARTESIAN_POINT('Ctrl Pts',(2.90343386677729,-2.82403072669977,17.4797428349941));
#8516=CARTESIAN_POINT('Ctrl Pts',(2.93051863454886,-2.8387572984458,17.4778810282201));
#8517=CARTESIAN_POINT('Ctrl Pts',(2.96818340877761,-2.85854168429103,17.4752795717097));
#8518=CARTESIAN_POINT('Ctrl Pts',(2.97858693377309,-2.86393420883834,17.4745597272107));
#8519=CARTESIAN_POINT('Ctrl Pts',(2.99621952325265,-2.87295216092306,17.4733371270332));
#8520=CARTESIAN_POINT('Ctrl Pts',(3.00343337450779,-2.87660739833033,17.4728362160438));
#8521=CARTESIAN_POINT('Ctrl Pts',(3.01727804234486,-2.88355708536792,17.4718733616419));
#8522=CARTESIAN_POINT('Ctrl Pts',(3.02390656422465,-2.88685589241467,17.4714117142145));
#8523=CARTESIAN_POINT('Ctrl Pts',(3.03981106022875,-2.89470279525032,17.4703025785089));
#8524=CARTESIAN_POINT('Ctrl Pts',(3.04909758371662,-2.89922915322747,17.4696537793842));
#8525=CARTESIAN_POINT('Ctrl Pts',(3.08274736120653,-2.91543067326408,17.4672990189206));
#8526=CARTESIAN_POINT('Ctrl Pts',(3.10723466031358,-2.92684364842147,17.4655782058228));
#8527=CARTESIAN_POINT('Ctrl Pts',(3.28247572896301,-3.0058531191887,17.4532271512054));
#8528=CARTESIAN_POINT('Ctrl Pts',(3.43807472845809,-3.06207053171948,17.4420837889553));
#8529=CARTESIAN_POINT('Ctrl Pts',(3.63264751888794,-3.11589187379188,17.4284281942839));
#8530=CARTESIAN_POINT('Ctrl Pts',(3.66818020068284,-3.12507036535704,17.4259447738114));
#8531=CARTESIAN_POINT('Ctrl Pts',(3.85898907870392,-3.17089698573329,17.4126808919315));
#8532=CARTESIAN_POINT('Ctrl Pts',(4.01668296255306,-3.19658693281915,17.4019879880243));
#8533=CARTESIAN_POINT('Ctrl Pts',(4.2614399572273,-3.21799600106738,17.3860154573004));
#8534=CARTESIAN_POINT('Ctrl Pts',(4.34750688112334,-3.22205898574124,17.3805125245574));
#8535=CARTESIAN_POINT('Ctrl Pts',(4.45818015856971,-3.22284298054387,17.373578590175));
#8536=CARTESIAN_POINT('Ctrl Pts',(4.48272188194024,-3.22273651579276,17.3720498664936));
#8537=CARTESIAN_POINT('Ctrl Pts',(4.52254084771386,-3.22210887974095,17.369583383438));
#8538=CARTESIAN_POINT('Ctrl Pts',(4.53781944168036,-3.22175933981559,17.3686403034034));
#8539=CARTESIAN_POINT('Ctrl Pts',(4.56718031021658,-3.22087863184655,17.3668341624359));
#8540=CARTESIAN_POINT('Ctrl Pts',(4.58126268649436,-3.22036375337563,17.3659706136328));
#8541=CARTESIAN_POINT('Ctrl Pts',(4.61353120282899,-3.21897197010636,17.3639979208628));
#8542=CARTESIAN_POINT('Ctrl Pts',(4.63171430059792,-3.21803327973238,17.3628907319167));
#8543=CARTESIAN_POINT('Ctrl Pts',(4.68958626687517,-3.21455370787104,17.3593801653059));
#8544=CARTESIAN_POINT('Ctrl Pts',(4.72923742370364,-3.21143220472174,17.3569949096965));
#8545=CARTESIAN_POINT('Ctrl Pts',(5.02331932522896,-3.18279460040851,17.3394310924527));
#8546=CARTESIAN_POINT('Ctrl Pts',(5.27396187208866,-3.12781403392186,17.3252646958498));
#8547=CARTESIAN_POINT('Ctrl Pts',(5.63441523565642,-3.00240168649888,17.3038890654157));
#8548=CARTESIAN_POINT('Ctrl Pts',(5.75080522490167,-2.95409247797503,17.296798655125));
#8549=CARTESIAN_POINT('Ctrl Pts',(5.90030753851901,-2.88150509558005,17.2870897457788));
#8550=CARTESIAN_POINT('Ctrl Pts',(5.93621866209718,-2.86322929491492,17.2847093826322));
#8551=CARTESIAN_POINT('Ctrl Pts',(5.99619368212348,-2.83127731533167,17.2806361880545));
#8552=CARTESIAN_POINT('Ctrl Pts',(6.02044184046601,-2.81795531828166,17.2789617692416));
#8553=CARTESIAN_POINT('Ctrl Pts',(6.05428516475463,-2.79879036087014,17.276581419683));
#8554=CARTESIAN_POINT('Ctrl Pts',(6.06402663050121,-2.79320647973406,17.2758911426017));
#8555=CARTESIAN_POINT('Ctrl Pts',(6.08065452762133,-2.7835594496884,17.2747037602563));
#8556=CARTESIAN_POINT('Ctrl Pts',(6.08755549184291,-2.77952130672651,17.2742082521505));
#8557=CARTESIAN_POINT('Ctrl Pts',(6.1009210053411,-2.77163347562565,17.2732431625058));
#8558=CARTESIAN_POINT('Ctrl Pts',(6.10738716690114,-2.7677867919894,17.2727737975309));
#8559=CARTESIAN_POINT('Ctrl Pts',(6.12497710498134,-2.7572390654458,17.2714903885631));
#8560=CARTESIAN_POINT('Ctrl Pts',(6.13607380042161,-2.75049345822574,17.2706735240382));
#8561=CARTESIAN_POINT('Ctrl Pts',(6.17858499059505,-2.72429800399969,17.2675171843821));
#8562=CARTESIAN_POINT('Ctrl Pts',(6.20970358930844,-2.70437632555377,17.2651497808155));
#8563=CARTESIAN_POINT('Ctrl Pts',(6.42270387977984,-2.5627952617542,17.2485838177806));
#8564=CARTESIAN_POINT('Ctrl Pts',(6.59211552015056,-2.42342820268489,17.233598352804));
#8565=CARTESIAN_POINT('Ctrl Pts',(6.84331554104593,-2.16983124576322,17.2095497425833));
#8566=CARTESIAN_POINT('Ctrl Pts',(6.93413517870308,-2.06552205300968,17.2003534785003));
#8567=CARTESIAN_POINT('Ctrl Pts',(7.06583416808997,-1.89302624096835,17.1862924756662));
#8568=CARTESIAN_POINT('Ctrl Pts',(7.11136860825697,-1.82861825969781,17.1812659963406));
#8569=CARTESIAN_POINT('Ctrl Pts',(7.16752747256039,-1.74265534651719,17.1748372435296));
#8570=CARTESIAN_POINT('Ctrl Pts',(7.18033584657732,-1.72256644347301,17.1733539461284));
#8571=CARTESIAN_POINT('Ctrl Pts',(7.20091045736917,-1.68949342297908,17.1709423870277));
#8572=CARTESIAN_POINT('Ctrl Pts',(7.20880993584666,-1.67659366758962,17.1700092371288));
#8573=CARTESIAN_POINT('Ctrl Pts',(7.22392173916218,-1.65152161558649,17.1682097292093));
#8574=CARTESIAN_POINT('Ctrl Pts',(7.23114528870851,-1.6393565245945,17.1673429755271));
#8575=CARTESIAN_POINT('Ctrl Pts',(7.24766323351348,-1.61111689879409,17.1653453955555));
#8576=CARTESIAN_POINT('Ctrl Pts',(7.25689934362201,-1.59500872273912,17.1642166940894));
#8577=CARTESIAN_POINT('Ctrl Pts',(7.28646769057199,-1.54239158409041,17.1605637460476));
#8578=CARTESIAN_POINT('Ctrl Pts',(7.30622968094536,-1.50556590502938,17.158059809029));
#8579=CARTESIAN_POINT('Ctrl Pts',(7.41986887847896,-1.28354460694213,17.1432540232464));
#8580=CARTESIAN_POINT('Ctrl Pts',(7.49638975284808,-1.09000943486189,17.1315784981138));
#8581=CARTESIAN_POINT('Ctrl Pts',(7.61036373587296,-0.693562947500273,17.1085083507381));
#8582=CARTESIAN_POINT('Ctrl Pts',(7.64805616436984,-0.491764102507658,17.0971512371842));
#8583=CARTESIAN_POINT('Ctrl Pts',(7.6692386096317,-0.255500116449311,17.0829964143166));
#8584=CARTESIAN_POINT('Ctrl Pts',(7.67164570852725,-0.22317577015947,17.0810409566029));
#8585=CARTESIAN_POINT('Ctrl Pts',(7.67427227269532,-0.178894157323701,17.0783296688662));
#8586=CARTESIAN_POINT('Ctrl Pts',(7.67491342058057,-0.166962638465749,17.0775958997524));
#8587=CARTESIAN_POINT('Ctrl Pts',(7.67587942940681,-0.146904327247348,17.076356519675));
#8588=CARTESIAN_POINT('Ctrl Pts',(7.676239910841,-0.138779227190497,17.0758528727562));
#8589=CARTESIAN_POINT('Ctrl Pts',(7.67686790054002,-0.123301654468929,17.0748902681147));
#8590=CARTESIAN_POINT('Ctrl Pts',(7.67714099376114,-0.115949483331574,17.0744316406517));
#8591=CARTESIAN_POINT('Ctrl Pts',(7.67773096357435,-0.0984512680055124,
17.0733369479978));
#8592=CARTESIAN_POINT('Ctrl Pts',(7.67802508056954,-0.0883046061388677,
17.0726996457262));
#8593=CARTESIAN_POINT('Ctrl Pts',(7.67889809343006,-0.0523170574305221,
17.0704307528381));
#8594=CARTESIAN_POINT('Ctrl Pts',(7.67921402492626,-0.0264715562262677,
17.06878565696));
#8595=CARTESIAN_POINT('Ctrl Pts',(7.67921904541626,-0.000626018462678653,
17.0671267777979));
#8596=CARTESIAN_POINT('Origin',(4.45646910621825,-5.13094777615093E-16,
-2.31077344927308));
#8597=CARTESIAN_POINT('',(7.67921910621823,-2.74841093364834E-11,15.8122671767608));
#8598=CARTESIAN_POINT('',(7.67921901097264,-0.000783521410691963,16.0578089001723));
#8599=CARTESIAN_POINT('',(7.67921910621823,-3.51191647465084E-13,-2.31077344927308));
#8600=CARTESIAN_POINT('',(7.67921774902577,0.00295766498587945,17.311387620665));
#8601=CARTESIAN_POINT('Ctrl Pts',(7.6792190109727,-0.000783520933934101,
16.0578089001435));
#8602=CARTESIAN_POINT('Ctrl Pts',(7.67921491899289,-0.0176145039721776,
16.0588276805675));
#8603=CARTESIAN_POINT('Ctrl Pts',(7.67907897611209,-0.0344447885085603,
16.0598528746788));
#8604=CARTESIAN_POINT('Ctrl Pts',(7.67865038393961,-0.0613805116184825,
16.0615050578984));
#8605=CARTESIAN_POINT('Ctrl Pts',(7.6784419992823,-0.0714872271008963,16.0621275601583));
#8606=CARTESIAN_POINT('Ctrl Pts',(7.67798711827065,-0.0894483808643351,
16.0632386841219));
#8607=CARTESIAN_POINT('Ctrl Pts',(7.67775944040108,-0.0973031149845316,
16.0637262548862));
#8608=CARTESIAN_POINT('Ctrl Pts',(7.67720772453566,-0.114202549861549,16.0647789061789));
#8609=CARTESIAN_POINT('Ctrl Pts',(7.67687432041597,-0.123246588449949,16.065344474249));
#8610=CARTESIAN_POINT('Ctrl Pts',(7.67584024310604,-0.148416969419151,16.0669244641013));
#8611=CARTESIAN_POINT('Ctrl Pts',(7.67505651110471,-0.164539374364985,16.0679433113746));
#8612=CARTESIAN_POINT('Ctrl Pts',(7.66970318492263,-0.259888642933266,16.0740065108407));
#8613=CARTESIAN_POINT('Ctrl Pts',(7.6623298918754,-0.338924387070562,16.0791857297162));
#8614=CARTESIAN_POINT('Ctrl Pts',(7.62421756467202,-0.630569443723733,16.0986801740901));
#8615=CARTESIAN_POINT('Ctrl Pts',(7.57516724304894,-0.840222401023601,16.1134122761078));
#8616=CARTESIAN_POINT('Ctrl Pts',(7.45350925688677,-1.19573261401036,16.1385094717261));
#8617=CARTESIAN_POINT('Ctrl Pts',(7.3900524302319,-1.34392284283161,16.1490192470493));
#8618=CARTESIAN_POINT('Ctrl Pts',(7.30328453056901,-1.51079205072159,16.160858081982));
#8619=CARTESIAN_POINT('Ctrl Pts',(7.29049079432192,-1.53465690761307,16.1625518163035));
#8620=CARTESIAN_POINT('Ctrl Pts',(7.26897798259115,-1.57359923656831,16.1653172388882));
#8621=CARTESIAN_POINT('Ctrl Pts',(7.26043496188212,-1.5887719270955,16.1663951132472));
#8622=CARTESIAN_POINT('Ctrl Pts',(7.24481966077702,-1.61598692630935,16.1683294721022));
#8623=CARTESIAN_POINT('Ctrl Pts',(7.23779132982529,-1.62805382568155,16.1691875072791));
#8624=CARTESIAN_POINT('Ctrl Pts',(7.22259419896889,-1.65376004166844,16.1710163338651));
#8625=CARTESIAN_POINT('Ctrl Pts',(7.21440243324587,-1.66738540295784,16.1719862636914));
#8626=CARTESIAN_POINT('Ctrl Pts',(7.19184339508827,-1.70428671664892,16.1746150715596));
#8627=CARTESIAN_POINT('Ctrl Pts',(7.17727988634051,-1.7274416000197,16.1762667371265));
#8628=CARTESIAN_POINT('Ctrl Pts',(7.09519107377515,-1.854342550025,16.1853354552417));
#8629=CARTESIAN_POINT('Ctrl Pts',(7.0220227803968,-1.95432323047479,16.1925372813961));
#8630=CARTESIAN_POINT('Ctrl Pts',(6.84826378034748,-2.16512110206393,16.208126209407));
#8631=CARTESIAN_POINT('Ctrl Pts',(6.74534957900526,-2.27364446777784,16.2164290720521));
#8632=CARTESIAN_POINT('Ctrl Pts',(6.51061621612745,-2.48902010157701,16.2342667571056));
#8633=CARTESIAN_POINT('Ctrl Pts',(6.37715500206396,-2.59339412895388,16.2437929356195));
#8634=CARTESIAN_POINT('Ctrl Pts',(6.21368521430928,-2.70167254249933,16.2555472990377));
#8635=CARTESIAN_POINT('Ctrl Pts',(6.19104605459125,-2.71626318314095,16.2571771699683));
#8636=CARTESIAN_POINT('Ctrl Pts',(6.15948311670992,-2.73604958968973,16.2594561077038));
#8637=CARTESIAN_POINT('Ctrl Pts',(6.15071255162724,-2.74148923363464,16.2600900652648));
#8638=CARTESIAN_POINT('Ctrl Pts',(6.13560723047503,-2.75075762466987,16.2611833786475));
#8639=CARTESIAN_POINT('Ctrl Pts',(6.12928506965769,-2.75460688663026,16.2616414099417));
#8640=CARTESIAN_POINT('Ctrl Pts',(6.11602457029854,-2.76261808558821,16.2626031493102));
#8641=CARTESIAN_POINT('Ctrl Pts',(6.10908377317528,-2.76677570154484,16.2631071419028));
#8642=CARTESIAN_POINT('Ctrl Pts',(6.09203882948686,-2.77689879638773,16.2643461597925));
#8643=CARTESIAN_POINT('Ctrl Pts',(6.08191767322952,-2.78283527918043,16.2650830179291));
#8644=CARTESIAN_POINT('Ctrl Pts',(6.04500058880823,-2.80421859373254,16.2677742105272));
#8645=CARTESIAN_POINT('Ctrl Pts',(6.01801601511951,-2.81933419085409,16.2697479807669));
#8646=CARTESIAN_POINT('Ctrl Pts',(5.94967408228979,-2.85633429467298,16.2747554829605));
#8647=CARTESIAN_POINT('Ctrl Pts',(5.90805069298341,-2.87771040174079,16.2778130769657));
#8648=CARTESIAN_POINT('Ctrl Pts',(5.5650595794132,-3.04452223994572,16.3029879822869));
#8649=CARTESIAN_POINT('Ctrl Pts',(5.24315974360506,-3.14313291685941,16.3262020408946));
#8650=CARTESIAN_POINT('Ctrl Pts',(4.84721290872578,-3.19963914254381,16.3519556504451));
#8651=CARTESIAN_POINT('Ctrl Pts',(4.78237768933826,-3.20689194468982,16.3560975010557));
#8652=CARTESIAN_POINT('Ctrl Pts',(4.69442392759861,-3.21403558476308,16.3616180247218));
#8653=CARTESIAN_POINT('Ctrl Pts',(4.67146504238629,-3.21565297081346,16.3630501076816));
#8654=CARTESIAN_POINT('Ctrl Pts',(4.63356461364472,-3.21791521236215,16.3653998703246));
#8655=CARTESIAN_POINT('Ctrl Pts',(4.61863269892055,-3.2187022406429,16.3663219661153));
#8656=CARTESIAN_POINT('Ctrl Pts',(4.58948111051868,-3.22003537942379,16.3681152252426));
#8657=CARTESIAN_POINT('Ctrl Pts',(4.57526225164126,-3.22059128683993,16.3689866745974));
#8658=CARTESIAN_POINT('Ctrl Pts',(4.54166707317465,-3.22168194808148,16.3710382793572));
#8659=CARTESIAN_POINT('Ctrl Pts',(4.52228855360779,-3.2221361072898,16.3722158932403));
#8660=CARTESIAN_POINT('Ctrl Pts',(4.45759824733044,-3.2230683482113,16.3761286368861));
#8661=CARTESIAN_POINT('Ctrl Pts',(4.41227941174319,-3.22276564906168,16.3788394633201));
#8662=CARTESIAN_POINT('Ctrl Pts',(4.30388834749897,-3.21975470141702,16.385261517645));
#8663=CARTESIAN_POINT('Ctrl Pts',(4.24085903161981,-3.21614897381777,16.3889458313074));
#8664=CARTESIAN_POINT('Ctrl Pts',(3.85027391676939,-3.18226960371922,16.4115671507917));
#8665=CARTESIAN_POINT('Ctrl Pts',(3.52891645917528,-3.10385270046426,16.4290497005579));
#8666=CARTESIAN_POINT('Ctrl Pts',(3.18435944694149,-2.9613833180992,16.4510698935684));
#8667=CARTESIAN_POINT('Ctrl Pts',(3.14404313847831,-2.94373772429456,16.4537045261762));
#8668=CARTESIAN_POINT('Ctrl Pts',(3.09148671883608,-2.91944067165926,16.4572321280126));
#8669=CARTESIAN_POINT('Ctrl Pts',(3.07890851981518,-2.91352665473817,16.4580835067525));
#8670=CARTESIAN_POINT('Ctrl Pts',(3.05864991386217,-2.90384095236538,16.4594669192179));
#8671=CARTESIAN_POINT('Ctrl Pts',(3.05094542771825,-2.90011964517514,16.459995904293));
#8672=CARTESIAN_POINT('Ctrl Pts',(3.03605578319789,-2.89285460039557,16.4610239479468));
#8673=CARTESIAN_POINT('Ctrl Pts',(3.02886891249811,-2.88931469879349,16.46152277358));
#8674=CARTESIAN_POINT('Ctrl Pts',(3.01156531959131,-2.88071147408355,16.4627299793861));
#8675=CARTESIAN_POINT('Ctrl Pts',(3.00146196346637,-2.87562162932976,16.4634399820211));
#8676=CARTESIAN_POINT('Ctrl Pts',(2.96627685460063,-2.85766326082043,16.4659299885911));
#8677=CARTESIAN_POINT('Ctrl Pts',(2.94133812734378,-2.84451933548115,16.4677259100044));
#8678=CARTESIAN_POINT('Ctrl Pts',(2.88028716338874,-2.81131188963385,16.4721935582341));
#8679=CARTESIAN_POINT('Ctrl Pts',(2.84438281915184,-2.79087827402263,16.4748834102314));
#8680=CARTESIAN_POINT('Ctrl Pts',(2.69593574253986,-2.70257486529262,16.4862385244467));
#8681=CARTESIAN_POINT('Ctrl Pts',(2.58721013952809,-2.62854631929875,16.4951225665968));
#8682=CARTESIAN_POINT('Ctrl Pts',(2.40432756615846,-2.48692833352997,16.5107710290758));
#8683=CARTESIAN_POINT('Ctrl Pts',(2.32822561469016,-2.42212268483333,16.5175260758181));
#8684=CARTESIAN_POINT('Ctrl Pts',(2.13566062501915,-2.24204728690098,16.5351478272682));
#8685=CARTESIAN_POINT('Ctrl Pts',(2.02474934220106,-2.12124522009336,16.5458466548834));
#8686=CARTESIAN_POINT('Ctrl Pts',(1.90669806434585,-1.97117292032354,16.5578663316139));
#8687=CARTESIAN_POINT('Ctrl Pts',(1.89017807050392,-1.94961674190697,16.5595651932827));
#8688=CARTESIAN_POINT('Ctrl Pts',(1.86350165986471,-1.91388124257981,16.5623372368716));
#8689=CARTESIAN_POINT('Ctrl Pts',(1.85318462124812,-1.89982407027428,16.5634166554299));
#8690=CARTESIAN_POINT('Ctrl Pts',(1.83481014416316,-1.87435773124241,16.5653526918951));
#8691=CARTESIAN_POINT('Ctrl Pts',(1.82671188677445,-1.86297868869068,16.5662108720084));
#8692=CARTESIAN_POINT('Ctrl Pts',(1.80956361804907,-1.83854864281835,16.5680388454591));
#8693=CARTESIAN_POINT('Ctrl Pts',(1.80053556451908,-1.82548262426834,16.5690077857424));
#8694=CARTESIAN_POINT('Ctrl Pts',(1.77626545503593,-1.78979605603409,16.57163101249));
#8695=CARTESIAN_POINT('Ctrl Pts',(1.7612131813262,-1.7670475666259,16.573278139314));
#8696=CARTESIAN_POINT('Ctrl Pts',(1.68016425333615,-1.64111283404236,16.5822649008892));
#8697=CARTESIAN_POINT('Ctrl Pts',(1.61979865577896,-1.53441377099373,16.589394103827));
#8698=CARTESIAN_POINT('Ctrl Pts',(1.49644110327114,-1.28408189946112,16.6053266455819));
#8699=CARTESIAN_POINT('Ctrl Pts',(1.43755833075741,-1.13877639725991,16.614018535334));
#8700=CARTESIAN_POINT('Ctrl Pts',(1.38684647765155,-0.981635108186533,16.6232699458685));
#8701=CARTESIAN_POINT('Ctrl Pts',(1.38425471873931,-0.973493361195649,16.623748903725));
#8702=CARTESIAN_POINT('Ctrl Pts',(1.36000183104895,-0.896243861082445,16.6282904877374));
#8703=CARTESIAN_POINT('Ctrl Pts',(1.34064433330498,-0.826436890287925,16.6323728992154));
#8704=CARTESIAN_POINT('Ctrl Pts',(1.31760300182023,-0.730960160716594,16.6379944089174));
#8705=CARTESIAN_POINT('Ctrl Pts',(1.31185206768902,-0.705809327432867,16.6394788068208));
#8706=CARTESIAN_POINT('Ctrl Pts',(1.29089341995096,-0.608804009030981,16.6452267605403));
#8707=CARTESIAN_POINT('Ctrl Pts',(1.27784283678885,-0.536511894026225,16.6495579506666));
#8708=CARTESIAN_POINT('Ctrl Pts',(1.26492277517286,-0.44767890112563,16.6550065264959));
#8709=CARTESIAN_POINT('Ctrl Pts',(1.26269475730998,-0.431497119722543,16.6560041328377));
#8710=CARTESIAN_POINT('Ctrl Pts',(1.25940556124783,-0.406185571052742,16.6575735223661));
#8711=CARTESIAN_POINT('Ctrl Pts',(1.25826023038957,-0.397066758091685,16.6581407233909));
#8712=CARTESIAN_POINT('Ctrl Pts',(1.25621033275057,-0.380161533656425,16.6591958037145));
#8713=CARTESIAN_POINT('Ctrl Pts',(1.25529515518352,-0.372376609991201,16.6596830853476));
#8714=CARTESIAN_POINT('Ctrl Pts',(1.25326895626629,-0.354581169288587,16.6608001527638));
#8715=CARTESIAN_POINT('Ctrl Pts',(1.25217646003025,-0.344568770241947,16.6614309491695));
#8716=CARTESIAN_POINT('Ctrl Pts',(1.2489392959599,-0.313553505739142,16.6633917042396));
#8717=CARTESIAN_POINT('Ctrl Pts',(1.24695411542745,-0.292535046970126,16.6647300387172));
#8718=CARTESIAN_POINT('Ctrl Pts',(1.24279173168614,-0.243302368684655,16.6678849016947));
#8719=CARTESIAN_POINT('Ctrl Pts',(1.24077938528471,-0.215076297795103,16.6697089915932));
#8720=CARTESIAN_POINT('Ctrl Pts',(1.23496653061059,-0.114974445106646,16.6762239787322));
#8721=CARTESIAN_POINT('Ctrl Pts',(1.23320255836729,-0.0430051241223538,
16.6809915057223));
#8722=CARTESIAN_POINT('Ctrl Pts',(1.23586096321087,0.252837590994247,16.7007863128731));
#8723=CARTESIAN_POINT('Ctrl Pts',(1.26119837873316,0.475922231887378,16.7161232468502));
#8724=CARTESIAN_POINT('Ctrl Pts',(1.33649777901908,0.817090503063733,16.73921193732));
#8725=CARTESIAN_POINT('Ctrl Pts',(1.3706708412395,0.937930545330958,16.7473271362832));
#8726=CARTESIAN_POINT('Ctrl Pts',(1.42104743404263,1.08310995181859,16.7569880328314));
#8727=CARTESIAN_POINT('Ctrl Pts',(1.4306358121081,1.10961473177599,16.7587483672855));
#8728=CARTESIAN_POINT('Ctrl Pts',(1.44629694242589,1.15119285542561,16.7615051098234));
#8729=CARTESIAN_POINT('Ctrl Pts',(1.45213792204609,1.16635140387094,16.7625091714518));
#8730=CARTESIAN_POINT('Ctrl Pts',(1.46320198621567,1.1944302817629,16.7643674101083));
#8731=CARTESIAN_POINT('Ctrl Pts',(1.46839471712496,1.20736208511777,16.7652225794241));
#8732=CARTESIAN_POINT('Ctrl Pts',(1.48009071404442,1.23595172653589,16.7671119407984));
#8733=CARTESIAN_POINT('Ctrl Pts',(1.48663401916398,1.25159281579153,16.7681447543351));
#8734=CARTESIAN_POINT('Ctrl Pts',(1.50601174020839,1.29690553630237,16.7711349302513));
#8735=CARTESIAN_POINT('Ctrl Pts',(1.51916978412621,1.32643712454552,16.7730812867879));
#8736=CARTESIAN_POINT('Ctrl Pts',(1.62094443247679,1.54591326767384,16.7875394114354));
#8737=CARTESIAN_POINT('Ctrl Pts',(1.72746040481548,1.72701327297481,16.7993848451652));
#8738=CARTESIAN_POINT('Ctrl Pts',(1.98489644326414,2.0807097893377,16.8238695613919));
#8739=CARTESIAN_POINT('Ctrl Pts',(2.13810542493385,2.2501521667208,16.8364299771638));
#8740=CARTESIAN_POINT('Ctrl Pts',(2.32610370919936,2.41831751652797,16.8515891434468));
#8741=CARTESIAN_POINT('Ctrl Pts',(2.34452634094959,2.43442272624639,16.8530726225572));
#8742=CARTESIAN_POINT('Ctrl Pts',(2.37067070633125,2.45675822220885,16.8551780374351));
#8743=CARTESIAN_POINT('Ctrl Pts',(2.37824105586183,2.46316546177386,16.8557876971535));
#8744=CARTESIAN_POINT('Ctrl Pts',(2.39198996927544,2.47469348651566,16.8568952167836));
#8745=CARTESIAN_POINT('Ctrl Pts',(2.39815837816735,2.47982638583456,16.8573922052445));
#8746=CARTESIAN_POINT('Ctrl Pts',(2.41080481654098,2.49027013514356,16.8584114864115));
#8747=CARTESIAN_POINT('Ctrl Pts',(2.4172844671751,2.49557883789633,16.8589339166768));
#8748=CARTESIAN_POINT('Ctrl Pts',(2.43393955250154,2.5091159826995,16.8602770538247));
#8749=CARTESIAN_POINT('Ctrl Pts',(2.44414442840857,2.51730772605329,16.8611003025124));
#8750=CARTESIAN_POINT('Ctrl Pts',(2.48673433922446,2.55107138848306,16.86453628635));
#8751=CARTESIAN_POINT('Ctrl Pts',(2.51955760066113,2.57608107967437,16.8671847029899));
#8752=CARTESIAN_POINT('Ctrl Pts',(2.60927894634575,2.64176013822776,16.8744051995576));
#8753=CARTESIAN_POINT('Ctrl Pts',(2.66703406841434,2.68121784923661,16.8790330463247));
#8754=CARTESIAN_POINT('Ctrl Pts',(2.90633382545134,2.83352803699428,16.8979958404373));
#8755=CARTESIAN_POINT('Ctrl Pts',(3.09763113592772,2.93008008421822,16.9126328085388));
#8756=CARTESIAN_POINT('Ctrl Pts',(3.42539847577577,3.05645630560851,16.9359402172646));
#8757=CARTESIAN_POINT('Ctrl Pts',(3.55676772965079,3.09767298171816,16.9448651093177));
#8758=CARTESIAN_POINT('Ctrl Pts',(3.71589013979323,3.13661438758767,16.9551692861969));
#8759=CARTESIAN_POINT('Ctrl Pts',(3.74147096200509,3.14254431015215,16.9568109132848));
#8760=CARTESIAN_POINT('Ctrl Pts',(3.78388719923026,3.15183211617565,16.9595089632226));
#8761=CARTESIAN_POINT('Ctrl Pts',(3.80068168535266,3.1553692314905,16.9605710683739));
#8762=CARTESIAN_POINT('Ctrl Pts',(3.83117310908494,3.16153712164049,16.9624884552676));
#8763=CARTESIAN_POINT('Ctrl Pts',(3.84486029919415,3.16421344608838,16.9633451698897));
#8764=CARTESIAN_POINT('Ctrl Pts',(3.87436357327933,3.1697837806709,16.9651834881935));
#8765=CARTESIAN_POINT('Ctrl Pts',(3.89018486237877,3.17264845791358,16.9661641390154));
#8766=CARTESIAN_POINT('Ctrl Pts',(3.93379659584765,3.18020837732226,16.9688535580683));
#8767=CARTESIAN_POINT('Ctrl Pts',(3.96162862690468,3.18465772928577,16.9705545290887));
#8768=CARTESIAN_POINT('Ctrl Pts',(4.12750874490642,3.20894888438156,16.9806069581989));
#8769=CARTESIAN_POINT('Ctrl Pts',(4.2666764764671,3.2201790951297,16.9886806596702));
#8770=CARTESIAN_POINT('Ctrl Pts',(4.60205663584287,3.22541645961004,17.0077236362952));
#8771=CARTESIAN_POINT('Ctrl Pts',(4.79782855491159,3.21060393429043,17.0184902924625));
#8772=CARTESIAN_POINT('Ctrl Pts',(4.99797654072554,3.17693826758358,17.0300083129923));
#8773=CARTESIAN_POINT('Ctrl Pts',(5.0049104941181,3.17574858906294,17.0304080232));
#8774=CARTESIAN_POINT('Ctrl Pts',(5.12233761275765,3.1552052232168,17.0371894357207));
#8775=CARTESIAN_POINT('Ctrl Pts',(5.23173856450615,3.13012023375716,17.0436904259202));
#8776=CARTESIAN_POINT('Ctrl Pts',(5.35551541183524,3.0948517389064,17.0514838283109));
#8777=CARTESIAN_POINT('Ctrl Pts',(5.37139867645919,3.09019342448474,17.0524923502591));
#8778=CARTESIAN_POINT('Ctrl Pts',(5.3969482886031,3.08248587878171,17.0541293637971));
#8779=CARTESIAN_POINT('Ctrl Pts',(5.40663759181386,3.079512969267,17.0547536072247));
#8780=CARTESIAN_POINT('Ctrl Pts',(5.42380067694891,3.07415821400138,17.055865717006));
#8781=CARTESIAN_POINT('Ctrl Pts',(5.43127999164253,3.07179472431323,17.0563525125577));
#8782=CARTESIAN_POINT('Ctrl Pts',(5.4474615219152,3.06661625300323,17.0574104523252));
#8783=CARTESIAN_POINT('Ctrl Pts',(5.45616026659733,3.06379157093752,17.0579821354754));
#8784=CARTESIAN_POINT('Ctrl Pts',(5.48059778168218,3.05574099670985,17.0595962881212));
#8785=CARTESIAN_POINT('Ctrl Pts',(5.49630814662072,3.05043067871627,17.0606434895841));
#8786=CARTESIAN_POINT('Ctrl Pts',(5.59415427940313,3.01651365814902,17.0672219763189));
#8787=CARTESIAN_POINT('Ctrl Pts',(5.67513792586523,2.98471534237057,17.0729150331263));
#8788=CARTESIAN_POINT('Ctrl Pts',(6.00657120860778,2.83883996430468,17.0969889751586));
#8789=CARTESIAN_POINT('Ctrl Pts',(6.24322709943132,2.696174500723,17.1159506978192));
#8790=CARTESIAN_POINT('Ctrl Pts',(6.53602593173005,2.46399209950647,17.1403930355583));
#8791=CARTESIAN_POINT('Ctrl Pts',(6.61034199618662,2.39930167728656,17.1467137827531));
#8792=CARTESIAN_POINT('Ctrl Pts',(6.70085850170048,2.31290804866073,17.1545678442539));
#8793=CARTESIAN_POINT('Ctrl Pts',(6.71990319911003,2.29427408470581,17.1562298506081));
#8794=CARTESIAN_POINT('Ctrl Pts',(6.74983050238031,2.26425681348666,17.1588575094436));
#8795=CARTESIAN_POINT('Ctrl Pts',(6.76086421660871,2.2530265422505,17.1598298297017));
#8796=CARTESIAN_POINT('Ctrl Pts',(6.78057078306631,2.23267270142353,17.1615730456373));
#8797=CARTESIAN_POINT('Ctrl Pts',(6.78927325487103,2.22357837890843,17.1623452243043));
#8798=CARTESIAN_POINT('Ctrl Pts',(6.80708943077453,2.20474026614787,17.1639311145326));
#8799=CARTESIAN_POINT('Ctrl Pts',(6.81619636841305,2.19499038900004,17.1647445276665));
#8800=CARTESIAN_POINT('Ctrl Pts',(6.84248303574186,2.16649523370265,17.1671007451851));
#8801=CARTESIAN_POINT('Ctrl Pts',(6.8595020469077,2.14760257305164,17.1686367461373));
#8802=CARTESIAN_POINT('Ctrl Pts',(6.94732801149363,2.04775637483486,17.1766224599676));
#8803=CARTESIAN_POINT('Ctrl Pts',(7.0142775468229,1.96349273402446,17.1829121363089));
#8804=CARTESIAN_POINT('Ctrl Pts',(7.16599305054544,1.75157787881706,17.1978739101318));
#8805=CARTESIAN_POINT('Ctrl Pts',(7.24611658206469,1.62093028059307,17.2064034615225));
#8806=CARTESIAN_POINT('Ctrl Pts',(7.40135874376193,1.3219424323807,17.2252468936189));
#8807=CARTESIAN_POINT('Ctrl Pts',(7.47194111602398,1.15187592294832,17.2355408039456));
#8808=CARTESIAN_POINT('Ctrl Pts',(7.53574442367407,0.95126042667185,17.2481630464968));
#8809=CARTESIAN_POINT('Ctrl Pts',(7.5435325092681,0.925673981602462,17.2497817417243));
#8810=CARTESIAN_POINT('Ctrl Pts',(7.55387580989565,0.890109683910482,17.2520476952803));
#8811=CARTESIAN_POINT('Ctrl Pts',(7.55670323230842,0.880211278117644,17.252680073126));
#8812=CARTESIAN_POINT('Ctrl Pts',(7.56148014415612,0.86317941506813,17.2537713855274));
#8813=CARTESIAN_POINT('Ctrl Pts',(7.56345261391421,0.856052409973881,17.2542290065089));
#8814=CARTESIAN_POINT('Ctrl Pts',(7.56753345450884,0.841107454072355,17.2551907445052));
#8815=CARTESIAN_POINT('Ctrl Pts',(7.56963690535174,0.833288292193715,17.255695151277));
#8816=CARTESIAN_POINT('Ctrl Pts',(7.57472458335335,0.814087701768747,17.2569366367466));
#8817=CARTESIAN_POINT('Ctrl Pts',(7.57767597202928,0.802697762290085,17.2576755646251));
#8818=CARTESIAN_POINT('Ctrl Pts',(7.58387513030834,0.778222902142665,17.2592682943036));
#8819=CARTESIAN_POINT('Ctrl Pts',(7.58710328473699,0.765133289675284,17.2601231166666));
#8820=CARTESIAN_POINT('Ctrl Pts',(7.59601060132286,0.728015367292673,17.262554857176));
#8821=CARTESIAN_POINT('Ctrl Pts',(7.60149577315092,0.703942014637659,17.2641411485596));
#8822=CARTESIAN_POINT('Ctrl Pts',(7.65470592180679,0.457366147888939,17.2804662012447));
#8823=CARTESIAN_POINT('Ctrl Pts',(7.67900893588414,0.230485891480088,17.2960755674744));
#8824=CARTESIAN_POINT('Ctrl Pts',(7.67921774902577,0.00295766498587945,
17.311387620665));
#8825=CARTESIAN_POINT('Ctrl Pts',(7.67921775054129,0.00295601317713016,
17.3113877318274));
#8826=CARTESIAN_POINT('Ctrl Pts',(7.67921865433409,0.00197066675129393,
17.3114540430529));
#8827=CARTESIAN_POINT('Ctrl Pts',(7.67921910621818,0.000985328982374648,
17.3115203483787));
#8828=CARTESIAN_POINT('Ctrl Pts',(7.67921910621823,1.77253683985415E-10,
17.3115866477388));
#8829=CARTESIAN_POINT('',(7.67921808440022,-0.00256634505910285,15.8124366820589));
#8830=CARTESIAN_POINT('Ctrl Pts',(7.67921904541626,-0.000626018462678653,
17.0671267777979));
#8831=CARTESIAN_POINT('Ctrl Pts',(7.67922641406151,0.0373078484470186,17.0646920170307));
#8832=CARTESIAN_POINT('Ctrl Pts',(7.67856402138696,0.075237246115982,17.0622278733309));
#8833=CARTESIAN_POINT('Ctrl Pts',(7.67323678195464,0.226882242818845,17.0522795707411));
#8834=CARTESIAN_POINT('Ctrl Pts',(7.66321943395884,0.340321869569866,17.0446232903118));
#8835=CARTESIAN_POINT('Ctrl Pts',(7.60856111414402,0.72532554062384,17.0183407329052));
#8836=CARTESIAN_POINT('Ctrl Pts',(7.53517991272287,0.991654912655422,16.9997719067977));
#8837=CARTESIAN_POINT('Ctrl Pts',(7.41426989485969,1.2802158947923,16.9799671985172));
#8838=CARTESIAN_POINT('Ctrl Pts',(7.39909439897466,1.31472233668693,16.9776016405544));
#8839=CARTESIAN_POINT('Ctrl Pts',(7.37577552032328,1.36531761791377,16.9741358388106));
#8840=CARTESIAN_POINT('Ctrl Pts',(7.3680973423903,1.38161614519426,16.9730197946706));
#8841=CARTESIAN_POINT('Ctrl Pts',(7.35419959433934,1.41048653855108,16.9710433609457));
#8842=CARTESIAN_POINT('Ctrl Pts',(7.34803392117042,1.42308368974656,16.9701811349579));
#8843=CARTESIAN_POINT('Ctrl Pts',(7.33486864043715,1.44954296880113,16.9683702607652));
#8844=CARTESIAN_POINT('Ctrl Pts',(7.32785066294614,1.46339559446265,16.9674222804288));
#8845=CARTESIAN_POINT('Ctrl Pts',(7.30896822931891,1.50000835669644,16.9649166483615));
#8846=CARTESIAN_POINT('Ctrl Pts',(7.2969313865771,1.52267869536871,16.9633650827658));
#8847=CARTESIAN_POINT('Ctrl Pts',(7.23708751791692,1.63220976509306,16.9558648204866));
#8848=CARTESIAN_POINT('Ctrl Pts',(7.18555782115261,1.71698137789989,16.9500501588548));
#8849=CARTESIAN_POINT('Ctrl Pts',(7.02031498388442,1.96253632921389,16.93299963691));
#8850=CARTESIAN_POINT('Ctrl Pts',(6.89570686350565,2.11541409271351,16.9221247996718));
#8851=CARTESIAN_POINT('Ctrl Pts',(6.64392977320399,2.37226752492125,16.901933322919));
#8852=CARTESIAN_POINT('Ctrl Pts',(6.52129668612906,2.4797399633072,16.892689240058));
#8853=CARTESIAN_POINT('Ctrl Pts',(6.37763035591441,2.58757419174573,16.8818159626182));
#8854=CARTESIAN_POINT('Ctrl Pts',(6.36409314120027,2.59757026060535,16.8807909451575));
#8855=CARTESIAN_POINT('Ctrl Pts',(6.34230079643208,2.61339980887416,16.8791390273104));
#8856=CARTESIAN_POINT('Ctrl Pts',(6.3340952266952,2.61930140879531,16.8785166120754));
#8857=CARTESIAN_POINT('Ctrl Pts',(6.31946177290653,2.62972196712906,16.8774056316543));
#8858=CARTESIAN_POINT('Ctrl Pts',(6.31304494880182,2.63425614543059,16.8769181170332));
#8859=CARTESIAN_POINT('Ctrl Pts',(6.29920189307179,2.64396205158955,16.8758655769903));
#8860=CARTESIAN_POINT('Ctrl Pts',(6.29177056694333,2.64912589310753,16.8753000640578));
#8861=CARTESIAN_POINT('Ctrl Pts',(6.27102449420952,2.66341262622154,16.8737202085112));
#8862=CARTESIAN_POINT('Ctrl Pts',(6.25766302559902,2.67246674687792,16.8727014409875));
#8863=CARTESIAN_POINT('Ctrl Pts',(6.17820650817433,2.72544226456296,16.8666383823714));
#8864=CARTESIAN_POINT('Ctrl Pts',(6.11058068254245,2.76700702524492,16.8614592249629));
#8865=CARTESIAN_POINT('Ctrl Pts',(5.85448428938577,2.91166684309748,16.8419645268294));
#8866=CARTESIAN_POINT('Ctrl Pts',(5.65738124971003,2.99834352835722,16.8272320737738));
#8867=CARTESIAN_POINT('Ctrl Pts',(5.30004442139763,3.11454768893864,16.8021344607464));
#8868=CARTESIAN_POINT('Ctrl Pts',(5.14344046603789,3.15279408585368,16.7916246017548));
#8869=CARTESIAN_POINT('Ctrl Pts',(4.95790383448904,3.18361646477717,16.7797858096471));
#8870=CARTESIAN_POINT('Ctrl Pts',(4.93114006569536,3.18771675868674,16.7780921921655));
#8871=CARTESIAN_POINT('Ctrl Pts',(4.8870857183136,3.19389887380402,16.7753269828155));
#8872=CARTESIAN_POINT('Ctrl Pts',(4.86982471785276,3.19617863081447,16.7742492054875));
#8873=CARTESIAN_POINT('Ctrl Pts',(4.8386889941141,3.20003444918757,16.7723150365975));
#8874=CARTESIAN_POINT('Ctrl Pts',(4.82482099829171,3.20166041485179,16.7714570945202));
#8875=CARTESIAN_POINT('Ctrl Pts',(4.79514333238217,3.20494461853492,16.769628484665));
#8876=CARTESIAN_POINT('Ctrl Pts',(4.77933103136297,3.20657612271916,16.7686586781367));
#8877=CARTESIAN_POINT('Ctrl Pts',(4.73628349514404,3.21069609002996,16.7660302544208));
#8878=CARTESIAN_POINT('Ctrl Pts',(4.70902723647941,3.21295501610915,16.764378847195));
#8879=CARTESIAN_POINT('Ctrl Pts',(4.5583050755029,3.22351658916916,16.7553128179693));
#8880=CARTESIAN_POINT('Ctrl Pts',(4.43446163323033,3.22505045876536,16.7481132726778));
#8881=CARTESIAN_POINT('Ctrl Pts',(4.16157060515671,3.21270524461674,16.7325247338358));
#8882=CARTESIAN_POINT('Ctrl Pts',(4.01296221363759,3.19558188573533,16.7242201881454));
#8883=CARTESIAN_POINT('Ctrl Pts',(3.69973414324459,3.13721224565233,16.7063796869382));
#8884=CARTESIAN_POINT('Ctrl Pts',(3.53611007594965,3.09316564909594,16.6968524006383));
#8885=CARTESIAN_POINT('Ctrl Pts',(3.35134576716687,3.02746516622017,16.6850968248043));
#8886=CARTESIAN_POINT('Ctrl Pts',(3.32608481046238,3.01812427901765,16.6834670082483));
#8887=CARTESIAN_POINT('Ctrl Pts',(3.29131125786159,3.00476808555454,16.6811881776379));
#8888=CARTESIAN_POINT('Ctrl Pts',(3.28169566036188,3.00102172663583,16.6805542721145));
#8889=CARTESIAN_POINT('Ctrl Pts',(3.26521517066546,2.99450937551738,16.6794610568537));
#8890=CARTESIAN_POINT('Ctrl Pts',(3.25834143881846,2.99176577108572,16.6790030714752));
#8891=CARTESIAN_POINT('Ctrl Pts',(3.24397417543344,2.98597371920525,16.6780414406995));
#8892=CARTESIAN_POINT('Ctrl Pts',(3.23648262181709,2.98292071328848,16.6775375109211));
#8893=CARTESIAN_POINT('Ctrl Pts',(3.21815508496292,2.97537116785434,16.6762986724637));
#8894=CARTESIAN_POINT('Ctrl Pts',(3.20733206849318,2.97084362643378,16.6755619316185));
#8895=CARTESIAN_POINT('Ctrl Pts',(3.16807305158767,2.95416813190016,16.6728713185009));
#8896=CARTESIAN_POINT('Ctrl Pts',(3.13978855706311,2.94167059891326,16.6708980196557));
#8897=CARTESIAN_POINT('Ctrl Pts',(3.06918152884888,2.90925052600755,16.665891882294));
#8898=CARTESIAN_POINT('Ctrl Pts',(3.02710560509746,2.88881030585627,16.6628351956092));
#8899=CARTESIAN_POINT('Ctrl Pts',(2.68805127607453,2.7148790933123,16.6376829799644));
#8900=CARTESIAN_POINT('Ctrl Pts',(2.41613355028699,2.51693835727205,16.6144918129322));
#8901=CARTESIAN_POINT('Ctrl Pts',(2.13312914806322,2.23439000998588,16.5887378609379));
#8902=CARTESIAN_POINT('Ctrl Pts',(2.08819818628284,2.18671011517095,16.5845781627209));
#8903=CARTESIAN_POINT('Ctrl Pts',(2.02945986120961,2.12044216232553,16.5790380798669));
#8904=CARTESIAN_POINT('Ctrl Pts',(2.01435605574204,2.10302941780383,16.5776037947891));
#8905=CARTESIAN_POINT('Ctrl Pts',(1.98976024570209,2.07405128203211,16.5752514422341));
#8906=CARTESIAN_POINT('Ctrl Pts',(1.98015984364921,2.06257939754902,16.5743289382351));
#8907=CARTESIAN_POINT('Ctrl Pts',(1.96158721152768,2.04006965747755,16.5725356103906));
#8908=CARTESIAN_POINT('Ctrl Pts',(1.95260751073425,2.02903844140608,16.5716644953924));
#8909=CARTESIAN_POINT('Ctrl Pts',(1.93158060697397,2.00285554035508,16.5696148065946));
#8910=CARTESIAN_POINT('Ctrl Pts',(1.91959621498516,1.98765394577629,16.5684387618598));
#8911=CARTESIAN_POINT('Ctrl Pts',(1.88010806687893,1.93662624876962,16.5645364598637));
#8912=CARTESIAN_POINT('Ctrl Pts',(1.85321979075694,1.90032911275274,16.5618343266463));
#8913=CARTESIAN_POINT('Ctrl Pts',(1.79076293463419,1.81220248180522,16.5554364330263));
#8914=CARTESIAN_POINT('Ctrl Pts',(1.75592973124965,1.75987357654044,16.5517673084653));
#8915=CARTESIAN_POINT('Ctrl Pts',(1.53979864105369,1.41364205541139,16.5282127079555));
#8916=CARTESIAN_POINT('Ctrl Pts',(1.40524808344095,1.0933087138168,16.5099635909658));
#8917=CARTESIAN_POINT('Ctrl Pts',(1.31662246469314,0.726970786267712,16.4874714180596));
#8918=CARTESIAN_POINT('Ctrl Pts',(1.30962058478797,0.696037116993631,16.4855583468564));
#8919=CARTESIAN_POINT('Ctrl Pts',(1.30055572149833,0.653052466898911,16.4828745708855));
#8920=CARTESIAN_POINT('Ctrl Pts',(1.29810282509281,0.641084424641773,16.4821246228284));
#8921=CARTESIAN_POINT('Ctrl Pts',(1.29427852376111,0.621870297003964,16.4809158472514));
#8922=CARTESIAN_POINT('Ctrl Pts',(1.29286381304861,0.614632811139181,16.4804594489211));
#8923=CARTESIAN_POINT('Ctrl Pts',(1.28994446143114,0.599420634049377,16.4794977705213));
#8924=CARTESIAN_POINT('Ctrl Pts',(1.28844509031062,0.591445054350981,16.4789921854979));
#8925=CARTESIAN_POINT('Ctrl Pts',(1.28482857373238,0.57179941378067,16.4777435425726));
#8926=CARTESIAN_POINT('Ctrl Pts',(1.28274571153156,0.560123236981401,16.4769985875384));
#8927=CARTESIAN_POINT('Ctrl Pts',(1.27531578931681,0.517099963512778,16.4742438794933));
#8928=CARTESIAN_POINT('Ctrl Pts',(1.27036852724751,0.485686854722369,16.4722135024611));
#8929=CARTESIAN_POINT('Ctrl Pts',(1.25903963461298,0.406106944184073,16.4670304563079));
#8930=CARTESIAN_POINT('Ctrl Pts',(1.25328109350122,0.357860505628887,16.4638518828767));
#8931=CARTESIAN_POINT('Ctrl Pts',(1.23158769793012,0.133020067484351,16.4489239582926));
#8932=CARTESIAN_POINT('Ctrl Pts',(1.22915353331832,-0.0445635137069391,
16.4368243235861));
#8933=CARTESIAN_POINT('Ctrl Pts',(1.25543118670765,-0.42609201261151,16.4110572820287));
#8934=CARTESIAN_POINT('Ctrl Pts',(1.28903556867776,-0.628959367318881,16.3975156666417));
#8935=CARTESIAN_POINT('Ctrl Pts',(1.3487584313166,-0.853818267286595,16.3828661723043));
#8936=CARTESIAN_POINT('Ctrl Pts',(1.35614478696317,-0.880261587718025,16.3811483898693));
#8937=CARTESIAN_POINT('Ctrl Pts',(1.36879846741136,-0.923425538789335,16.3783519896799));
#8938=CARTESIAN_POINT('Ctrl Pts',(1.37386577871841,-0.940202873933742,16.3772669467542));
#8939=CARTESIAN_POINT('Ctrl Pts',(1.38321870183408,-0.970280757814361,16.3753248618623));
#8940=CARTESIAN_POINT('Ctrl Pts',(1.38745440601782,-0.983596246811233,16.3744662151625));
#8941=CARTESIAN_POINT('Ctrl Pts',(1.39666986875715,-1.01192708686171,16.3726415082342));
#8942=CARTESIAN_POINT('Ctrl Pts',(1.40167386871266,-1.02693421092204,16.3716762697239));
#8943=CARTESIAN_POINT('Ctrl Pts',(1.41551567054076,-1.06744953137409,16.3690735943346));
#8944=CARTESIAN_POINT('Ctrl Pts',(1.42456392449426,-1.09288486874238,16.3674431251106));
#8945=CARTESIAN_POINT('Ctrl Pts',(1.47484581757222,-1.2287982856096,16.3587450092682));
#8946=CARTESIAN_POINT('Ctrl Pts',(1.52180227840496,-1.33707056967685,16.3518714117494));
#8947=CARTESIAN_POINT('Ctrl Pts',(1.64318873995305,-1.57957478895859,16.3363637561783));
#8948=CARTESIAN_POINT('Ctrl Pts',(1.72147424354537,-1.7115514171787,16.3278430505824));
#8949=CARTESIAN_POINT('Ctrl Pts',(1.83584925075604,-1.87635576206542,16.3166133813224));
#8950=CARTESIAN_POINT('Ctrl Pts',(1.86369827092408,-1.91465366338749,16.3139577287342));
#8951=CARTESIAN_POINT('Ctrl Pts',(1.97571474945083,-2.06177076008277,16.3035219680895));
#8952=CARTESIAN_POINT('Ctrl Pts',(2.06596138160749,-2.16575724238562,16.2956334840394));
#8953=CARTESIAN_POINT('Ctrl Pts',(2.17556917385983,-2.27683026385919,16.2861887481779));
#8954=CARTESIAN_POINT('Ctrl Pts',(2.18869057571657,-2.2898997907435,16.2850600790611));
#8955=CARTESIAN_POINT('Ctrl Pts',(2.2088364926239,-2.30962308412409,16.2833287797662));
#8956=CARTESIAN_POINT('Ctrl Pts',(2.21577978402201,-2.31635975447106,16.2827323718179));
#8957=CARTESIAN_POINT('Ctrl Pts',(2.22838840867981,-2.32848342987639,16.2816496051689));
#8958=CARTESIAN_POINT('Ctrl Pts',(2.2340431208246,-2.33388119117334,16.2811640912687));
#8959=CARTESIAN_POINT('Ctrl Pts',(2.24662453340216,-2.34580371626504,16.2800840115047));
#8960=CARTESIAN_POINT('Ctrl Pts',(2.25356043847634,-2.35231832611619,16.2794887136877));
#8961=CARTESIAN_POINT('Ctrl Pts',(2.2739446666903,-2.37129517350995,16.2777398226892));
#8962=CARTESIAN_POINT('Ctrl Pts',(2.2874703543471,-2.38367323829133,16.2765801975406));
#8963=CARTESIAN_POINT('Ctrl Pts',(2.41116174664401,-2.49494526825097,16.2659889793383));
#8964=CARTESIAN_POINT('Ctrl Pts',(2.52790257640491,-2.58624346523975,16.2560963959517));
#8965=CARTESIAN_POINT('Ctrl Pts',(2.84934969901315,-2.80373582047553,16.2299067850006));
#8966=CARTESIAN_POINT('Ctrl Pts',(3.06265755433671,-2.91566243922233,16.2135905008431));
#8967=CARTESIAN_POINT('Ctrl Pts',(3.35563057078021,-3.02981624967571,16.1932506727074));
#8968=CARTESIAN_POINT('Ctrl Pts',(3.42573815898686,-3.0543783574797,16.1885202448652));
#8969=CARTESIAN_POINT('Ctrl Pts',(3.51968190060118,-3.08368773874728,16.1823570932969));
#8970=CARTESIAN_POINT('Ctrl Pts',(3.54280766752579,-3.09061857321385,16.1808537023805));
#8971=CARTESIAN_POINT('Ctrl Pts',(3.58061305738885,-3.10148748678316,16.1784178519824));
#8972=CARTESIAN_POINT('Ctrl Pts',(3.59524617456329,-3.10558263833907,16.1774803146664));
#8973=CARTESIAN_POINT('Ctrl Pts',(3.62353336297406,-3.11328363999004,16.1756779682489));
#8974=CARTESIAN_POINT('Ctrl Pts',(3.6371832167726,-3.11690353023258,16.1748127221981));
#8975=CARTESIAN_POINT('Ctrl Pts',(3.66898453856791,-3.12511378101737,16.1728070366949));
#8976=CARTESIAN_POINT('Ctrl Pts',(3.68715320815639,-3.12963594695978,16.1716688173208));
#8977=CARTESIAN_POINT('Ctrl Pts',(3.74573563746546,-3.14367607750028,16.1680225862752));
#8978=CARTESIAN_POINT('Ctrl Pts',(3.78629524026609,-3.15257173912639,16.1655344785044));
#8979=CARTESIAN_POINT('Ctrl Pts',(3.88223293692778,-3.17167780810815,16.1597265159112));
#8980=CARTESIAN_POINT('Ctrl Pts',(3.93772972516147,-3.18122574904888,16.1564269864891));
#8981=CARTESIAN_POINT('Ctrl Pts',(4.14760198313647,-3.2116945939568,16.1441327759674));
#8982=CARTESIAN_POINT('Ctrl Pts',(4.30318056163093,-3.22286958099581,16.1354020817183));
#8983=CARTESIAN_POINT('Ctrl Pts',(4.66805769108854,-3.22258723559974,16.1149984210397));
#8984=CARTESIAN_POINT('Ctrl Pts',(4.87661252494764,-3.20207650358121,16.1033947757592));
#8985=CARTESIAN_POINT('Ctrl Pts',(5.10688501374531,-3.15653875206495,16.0893056471989));
#8986=CARTESIAN_POINT('Ctrl Pts',(5.13202950220742,-3.15125305290691,16.0877493940194));
#8987=CARTESIAN_POINT('Ctrl Pts',(5.16699051503377,-3.14346614676949,16.0855573089383));
#8988=CARTESIAN_POINT('Ctrl Pts',(5.17686324906427,-3.14121829245557,16.084935122761));
#8989=CARTESIAN_POINT('Ctrl Pts',(5.19388465584204,-3.1372583418769,16.0838567097469));
#8990=CARTESIAN_POINT('Ctrl Pts',(5.20103843492549,-3.13556822740279,16.0834017264841));
#8991=CARTESIAN_POINT('Ctrl Pts',(5.21610198429949,-3.13195493526759,16.0824398750062));
#8992=CARTESIAN_POINT('Ctrl Pts',(5.22401031822904,-3.13002624736643,16.0819326827216));
#8993=CARTESIAN_POINT('Ctrl Pts',(5.24354246690118,-3.12518426487896,16.0806746544945));
#8994=CARTESIAN_POINT('Ctrl Pts',(5.25515742218511,-3.12223607817374,16.0799218590965));
#8995=CARTESIAN_POINT('Ctrl Pts',(5.29836265679485,-3.11101257513069,16.077104784977));
#8996=CARTESIAN_POINT('Ctrl Pts',(5.32984184554701,-3.10232233328631,16.0750186812156));
#8997=CARTESIAN_POINT('Ctrl Pts',(5.56138182832711,-3.03459951166415,16.0594527609299));
#8998=CARTESIAN_POINT('Ctrl Pts',(5.75540933622093,-2.9567498010121,16.0452124171109));
#8999=CARTESIAN_POINT('Ctrl Pts',(6.12115497022625,-2.76700914860504,16.0173949068354));
#9000=CARTESIAN_POINT('Ctrl Pts',(6.29251561768555,-2.6564029695707,16.0038770104438));
#9001=CARTESIAN_POINT('Ctrl Pts',(6.48516421461196,-2.50444874309693,15.9883020570688));
#9002=CARTESIAN_POINT('Ctrl Pts',(6.5175012381913,-2.47790519690094,15.9856717093837));
#9003=CARTESIAN_POINT('Ctrl Pts',(6.56343901095801,-2.43867595575881,15.9819099321802));
#9004=CARTESIAN_POINT('Ctrl Pts',(6.57746011071931,-2.42649124842,15.9807582653019));
#9005=CARTESIAN_POINT('Ctrl Pts',(6.60197444646242,-2.40481279769704,15.9787382092371));
#9006=CARTESIAN_POINT('Ctrl Pts',(6.61251186465673,-2.3953699904015,15.9778677379683));
#9007=CARTESIAN_POINT('Ctrl Pts',(6.62701260150798,-2.38220235652645,15.9766667455594));
#9008=CARTESIAN_POINT('Ctrl Pts',(6.63102907483247,-2.37853654078653,15.9763337546958));
#9009=CARTESIAN_POINT('Ctrl Pts',(6.63516905759745,-2.37473874706899,15.9759901715923));
#9010=CARTESIAN_POINT('Ctrl Pts',(6.63530183483533,-2.37461692398534,15.9759791518434));
#9011=CARTESIAN_POINT('Ctrl Pts',(6.6355505740188,-2.37438866741806,15.9759585072144));
#9012=CARTESIAN_POINT('Ctrl Pts',(6.63566653838777,-2.3742822365719,15.9759488822222));
#9013=CARTESIAN_POINT('Ctrl Pts',(6.63601831946668,-2.37395932821101,15.975919683675));
#9014=CARTESIAN_POINT('Ctrl Pts',(6.63625411176207,-2.37374282401828,15.9759001112467));
#9015=CARTESIAN_POINT('Ctrl Pts',(6.6367195680249,-2.37331531482025,15.975861472739));
#9016=CARTESIAN_POINT('Ctrl Pts',(6.63694923362345,-2.37310431160528,15.9758424065845));
#9017=CARTESIAN_POINT('Ctrl Pts',(6.63740284295748,-2.37268744064295,15.9758047470573));
#9018=CARTESIAN_POINT('Ctrl Pts',(6.63762678818554,-2.37248157451798,15.9757861536155));
#9019=CARTESIAN_POINT('Ctrl Pts',(6.63806933446912,-2.37207463938442,15.9757494083159));
#9020=CARTESIAN_POINT('Ctrl Pts',(6.63828793686706,-2.37187357187125,15.9757312563967));
#9021=CARTESIAN_POINT('Ctrl Pts',(6.63872014902901,-2.37147591868992,15.9756953650982));
#9022=CARTESIAN_POINT('Ctrl Pts',(6.63893376004545,-2.3712793343615,15.9756776256607));
#9023=CARTESIAN_POINT('Ctrl Pts',(6.65118788630558,-2.35999891192853,15.9746599190801));
#9024=CARTESIAN_POINT('Ctrl Pts',(6.66314399515584,-2.34882339435336,15.9736638447136));
#9025=CARTESIAN_POINT('Ctrl Pts',(6.69956824020663,-2.31425360994013,15.9706191685637));
#9026=CARTESIAN_POINT('Ctrl Pts',(6.72375381992902,-2.29056404702819,15.9685833007541));
#9027=CARTESIAN_POINT('Ctrl Pts',(6.7784411270563,-2.23528327040371,15.9639427127593));
#9028=CARTESIAN_POINT('Ctrl Pts',(6.80867974004409,-2.20344066359967,15.9613491415253));
#9029=CARTESIAN_POINT('Ctrl Pts',(6.90884871479582,-2.0935453657806,15.9526457062803));
#9030=CARTESIAN_POINT('Ctrl Pts',(6.97562262876506,-2.01270115083615,15.9466538201267));
#9031=CARTESIAN_POINT('Ctrl Pts',(7.09678512877229,-1.85050934541222,15.9352175767197));
#9032=CARTESIAN_POINT('Ctrl Pts',(7.15164262398297,-1.76965921483505,15.929769300325));
#9033=CARTESIAN_POINT('Ctrl Pts',(7.29928061992343,-1.52923912603593,15.9139890834805));
#9034=CARTESIAN_POINT('Ctrl Pts',(7.38212834925727,-1.36405654697205,15.9036608613047));
#9035=CARTESIAN_POINT('Ctrl Pts',(7.46028614308617,-1.16786834777868,15.8909987464818));
#9036=CARTESIAN_POINT('Ctrl Pts',(7.46987694698813,-1.14289384828441,15.8893796186732));
#9037=CARTESIAN_POINT('Ctrl Pts',(7.48272608057905,-1.10814812602912,15.8871132042093));
#9038=CARTESIAN_POINT('Ctrl Pts',(7.48625044451607,-1.09847557074047,15.88648080724));
#9039=CARTESIAN_POINT('Ctrl Pts',(7.49222655331929,-1.08182667940829,15.8853895028788));
#9040=CARTESIAN_POINT('Ctrl Pts',(7.49470076718004,-1.0748584156261,15.8849319093865));
#9041=CARTESIAN_POINT('Ctrl Pts',(7.49983361350887,-1.0602431717831,15.8839702802484));
#9042=CARTESIAN_POINT('Ctrl Pts',(7.50248743093015,-1.0525946361421,15.8834659552202));
#9043=CARTESIAN_POINT('Ctrl Pts',(7.50892633163067,-1.03380888742789,15.8822247615977));
#9044=CARTESIAN_POINT('Ctrl Pts',(7.5126792901654,-1.02266085784129,15.8814860452424));
#9045=CARTESIAN_POINT('Ctrl Pts',(7.52614200752061,-0.98193432200351,15.8787801314));
#9046=CARTESIAN_POINT('Ctrl Pts',(7.5354837229138,-0.952237132554293,15.8767932248743));
#9047=CARTESIAN_POINT('Ctrl Pts',(7.55790404277916,-0.877181349564938,15.8717450753413));
#9048=CARTESIAN_POINT('Ctrl Pts',(7.57041869710981,-0.831662958558692,15.8686595037599));
#9049=CARTESIAN_POINT('Ctrl Pts',(7.64633250482876,-0.529755630087821,15.8481056545554));
#9050=CARTESIAN_POINT('Ctrl Pts',(7.67900776168187,-0.266684111778894,15.8298838378527));
#9051=CARTESIAN_POINT('Ctrl Pts',(7.67921808440022,-0.00256634505910285,
15.8124366820589));
#9052=CARTESIAN_POINT('Ctrl Pts',(7.67921808747992,-0.00256247473102081,
15.8124364263919));
#9053=CARTESIAN_POINT('Ctrl Pts',(7.67921876664087,-0.0017083140070543,
15.8123800020577));
#9054=CARTESIAN_POINT('Ctrl Pts',(7.67921910621822,-0.000854155705641013,
15.8123235855046));
#9055=CARTESIAN_POINT('Ctrl Pts',(7.67921910621823,-2.74841093364834E-11,
15.8122671767608));
#9056=CARTESIAN_POINT('Origin',(4.45646910621825,-5.13094777615093E-16,
-2.31077344927308));
#9057=CARTESIAN_POINT('',(7.67921910621823,-1.84544675223763E-11,14.5621759541225));
#9058=CARTESIAN_POINT('',(7.67921910621823,2.3786865083016E-11,14.8122635502411));
#9059=CARTESIAN_POINT('',(7.67921910621823,-3.51191647465084E-13,-2.31077344927308));
#9060=CARTESIAN_POINT('',(7.67921816783712,-0.00245933620175732,14.8124033118825));
#9061=CARTESIAN_POINT('Ctrl Pts',(7.67921910621823,2.3786865083016E-11,
14.8122635502411));
#9062=CARTESIAN_POINT('Ctrl Pts',(7.67921910621823,-0.000819775054184794,
14.8123101427297));
#9063=CARTESIAN_POINT('Ctrl Pts',(7.67921879342738,-0.00163955385536296,
14.8123567299308));
#9064=CARTESIAN_POINT('Ctrl Pts',(7.67921816783712,-0.00245933620180352,
14.8124033118825));
#9065=CARTESIAN_POINT('Ctrl Pts',(7.67921817065546,-0.00245564023983482,
14.8124031018693));
#9066=CARTESIAN_POINT('Ctrl Pts',(7.67916398677161,-0.0735658371379256,
14.8164437511175));
#9067=CARTESIAN_POINT('Ctrl Pts',(7.67675624121047,-0.144657283957908,14.8204417577807));
#9068=CARTESIAN_POINT('Ctrl Pts',(7.65693647847182,-0.440237452401183,14.8370364533687));
#9069=CARTESIAN_POINT('Ctrl Pts',(7.61838122542217,-0.662635818713972,14.8494220805179));
#9070=CARTESIAN_POINT('Ctrl Pts',(7.54779577275092,-0.911565043813883,14.8648442997905));
#9071=CARTESIAN_POINT('Ctrl Pts',(7.53810318523207,-0.943812792510002,14.8668740737785));
#9072=CARTESIAN_POINT('Ctrl Pts',(7.52423546229692,-0.98745845462968,14.8696722761627));
#9073=CARTESIAN_POINT('Ctrl Pts',(7.52049821901749,-0.998994594656731,14.8704167681455));
#9074=CARTESIAN_POINT('Ctrl Pts',(7.51413420502902,-1.01826738091487,14.8716691762343));
#9075=CARTESIAN_POINT('Ctrl Pts',(7.51154291478027,-1.02601575870491,14.8721750353399));
#9076=CARTESIAN_POINT('Ctrl Pts',(7.50657224872985,-1.04069306414792,14.873137854759));
#9077=CARTESIAN_POINT('Ctrl Pts',(7.504198657536,-1.04762388919386,14.8735944597521));
#9078=CARTESIAN_POINT('Ctrl Pts',(7.49852091192929,-1.0640201532557,14.8746791691481));
#9079=CARTESIAN_POINT('Ctrl Pts',(7.49519620189542,-1.07347832158151,14.8753084595267));
#9080=CARTESIAN_POINT('Ctrl Pts',(7.48339423735058,-1.10655848395182,14.8775215847288));
#9081=CARTESIAN_POINT('Ctrl Pts',(7.47468547390956,-1.13009614451067,14.8791180971225));
#9082=CARTESIAN_POINT('Ctrl Pts',(7.38664412992046,-1.35977137215666,14.8948945341084));
#9083=CARTESIAN_POINT('Ctrl Pts',(7.2865986428985,-1.55732365816941,14.9099930932462));
#9084=CARTESIAN_POINT('Ctrl Pts',(7.08712282114353,-1.8675308530798,14.9348850835941));
#9085=CARTESIAN_POINT('Ctrl Pts',(6.99861212849077,-1.98633520196457,14.9447662312501));
#9086=CARTESIAN_POINT('Ctrl Pts',(6.86667537881657,-2.14009490638359,14.9579145561792));
#9087=CARTESIAN_POINT('Ctrl Pts',(6.83006004188112,-2.18063456779403,14.9614205251225));
#9088=CARTESIAN_POINT('Ctrl Pts',(6.76471952787671,-2.24938112752681,14.9674359063435));
#9089=CARTESIAN_POINT('Ctrl Pts',(6.7364645212211,-2.27801593685362,14.9699639235607));
#9090=CARTESIAN_POINT('Ctrl Pts',(6.69467183484033,-2.31881361055144,14.9736004166451));
#9091=CARTESIAN_POINT('Ctrl Pts',(6.68155647049997,-2.33140177959777,14.9747274430352));
#9092=CARTESIAN_POINT('Ctrl Pts',(6.65803514022487,-2.35359833533061,14.9767239242144));
#9093=CARTESIAN_POINT('Ctrl Pts',(6.64767111715006,-2.36325027951491,14.9775952442196));
#9094=CARTESIAN_POINT('Ctrl Pts',(6.62612832506414,-2.38304937996144,14.9793893634656));
#9095=CARTESIAN_POINT('Ctrl Pts',(6.61494118668094,-2.39318694699945,14.9803117437174));
#9096=CARTESIAN_POINT('Ctrl Pts',(6.586021710273,-2.41902546387145,14.9826727183195));
#9097=CARTESIAN_POINT('Ctrl Pts',(6.56818658696452,-2.43461040324936,14.9841064524206));
#9098=CARTESIAN_POINT('Ctrl Pts',(6.49667708818337,-2.49572078105314,14.989769350504));
#9099=CARTESIAN_POINT('Ctrl Pts',(6.44168728269488,-2.53968121904806,14.9939349224885));
#9100=CARTESIAN_POINT('Ctrl Pts',(6.12210599978859,-2.7784355454532,15.01721009849));
#9101=CARTESIAN_POINT('Ctrl Pts',(5.83043737062552,-2.93363660032036,15.0347322344474));
#9102=CARTESIAN_POINT('Ctrl Pts',(5.47644648393849,-3.05743844316518,15.0565147558549));
#9103=CARTESIAN_POINT('Ctrl Pts',(5.43218856466564,-3.07184875875863,15.0592507877455));
#9104=CARTESIAN_POINT('Ctrl Pts',(5.35814160150145,-3.09419673881673,15.0638729440253));
#9105=CARTESIAN_POINT('Ctrl Pts',(5.32852189574028,-3.10267473658088,15.0657335470274));
#9106=CARTESIAN_POINT('Ctrl Pts',(5.28747778554708,-3.1137885927299,15.0683336358798));
#9107=CARTESIAN_POINT('Ctrl Pts',(5.27615270024326,-3.11678899208406,15.0690533451905));
#9108=CARTESIAN_POINT('Ctrl Pts',(5.25698295075369,-3.12175600446902,15.0702758228254));
#9109=CARTESIAN_POINT('Ctrl Pts',(5.2491466463116,-3.12375499718228,15.070776747878));
#9110=CARTESIAN_POINT('Ctrl Pts',(5.23412019655623,-3.12752796768631,15.0717397190164));
#9111=CARTESIAN_POINT('Ctrl Pts',(5.22693134139263,-3.12930668815255,15.0722014696066));
#9112=CARTESIAN_POINT('Ctrl Pts',(5.209695343519,-3.1335083555683,15.0733109749551));
#9113=CARTESIAN_POINT('Ctrl Pts',(5.19964262458101,-3.13590776231487,15.0739600421062));
#9114=CARTESIAN_POINT('Ctrl Pts',(5.16324526498061,-3.14441032879497,15.0763167312534));
#9115=CARTESIAN_POINT('Ctrl Pts',(5.13683643246793,-3.15022999866435,15.078039235676));
#9116=CARTESIAN_POINT('Ctrl Pts',(4.94902443312715,-3.18914613116777,15.0903631142691));
#9117=CARTESIAN_POINT('Ctrl Pts',(4.78537925197181,-3.21015133415179,15.1014746765021));
#9118=CARTESIAN_POINT('Ctrl Pts',(4.48179962305897,-3.22565733684048,15.122036005141));
#9119=CARTESIAN_POINT('Ctrl Pts',(4.3424133502767,-3.22374042586903,15.131457439967));
#9120=CARTESIAN_POINT('Ctrl Pts',(4.11318825098388,-3.20569766475699,15.1467016091323));
#9121=CARTESIAN_POINT('Ctrl Pts',(4.02312898995123,-3.19477040685419,15.1526286579963));
#9122=CARTESIAN_POINT('Ctrl Pts',(3.87518073051021,-3.17044660910166,15.1622457337651));
#9123=CARTESIAN_POINT('Ctrl Pts',(3.81699100714112,-3.15922401578979,15.1659975467593));
#9124=CARTESIAN_POINT('Ctrl Pts',(3.73815318799753,-3.14175140790295,15.1710415994763));
#9125=CARTESIAN_POINT('Ctrl Pts',(3.71721248781034,-3.13689007705289,15.1723776313622));
#9126=CARTESIAN_POINT('Ctrl Pts',(3.68210168877383,-3.12836807024229,15.1746117886382));
#9127=CARTESIAN_POINT('Ctrl Pts',(3.66790528539886,-3.12481980150151,15.1755134896691));
#9128=CARTESIAN_POINT('Ctrl Pts',(3.63990958932302,-3.11761958146123,15.1772886055435));
#9129=CARTESIAN_POINT('Ctrl Pts',(3.62610942759744,-3.11397240093494,15.1781621509356));
#9130=CARTESIAN_POINT('Ctrl Pts',(3.59263237828971,-3.10488653676805,15.180277876917));
#9131=CARTESIAN_POINT('Ctrl Pts',(3.57298189287824,-3.09935229881371,15.1815169389064));
#9132=CARTESIAN_POINT('Ctrl Pts',(3.51730052904785,-3.08309795347374,15.1850208001341));
#9133=CARTESIAN_POINT('Ctrl Pts',(3.4814020997098,-3.07193344900454,15.187271214329));
#9134=CARTESIAN_POINT('Ctrl Pts',(3.25867460225429,-2.99836671792159,15.2011958885521));
#9135=CARTESIAN_POINT('Ctrl Pts',(3.07769267005492,-2.91957230184472,15.2123094245236));
#9136=CARTESIAN_POINT('Ctrl Pts',(2.71679310047202,-2.72135312549109,15.2353514374189));
#9137=CARTESIAN_POINT('Ctrl Pts',(2.53939296715385,-2.59942900765162,15.2472123668693));
#9138=CARTESIAN_POINT('Ctrl Pts',(2.3502247670444,-2.43945574961192,15.261987120572));
#9139=CARTESIAN_POINT('Ctrl Pts',(2.32532299546861,-2.41773150531196,15.2639799050779));
#9140=CARTESIAN_POINT('Ctrl Pts',(2.29181148491297,-2.38757615299691,15.2667349022613));
#9141=CARTESIAN_POINT('Ctrl Pts',(2.28290754403098,-2.37947318298986,15.2674741218123));
#9142=CARTESIAN_POINT('Ctrl Pts',(2.26805092895519,-2.36580005546202,15.2687201365073));
#9143=CARTESIAN_POINT('Ctrl Pts',(2.26207350663044,-2.36025675956711,15.269224920633));
#9144=CARTESIAN_POINT('Ctrl Pts',(2.25075312463964,-2.34967837588233,15.2701876575358));
#9145=CARTESIAN_POINT('Ctrl Pts',(2.24540622322211,-2.34464760387622,15.2706452672557));
#9146=CARTESIAN_POINT('Ctrl Pts',(2.23275363500033,-2.33266131671862,15.2717348951321));
#9147=CARTESIAN_POINT('Ctrl Pts',(2.22546337364863,-2.32568973217038,15.2723681242489));
#9148=CARTESIAN_POINT('Ctrl Pts',(2.19988690652591,-2.30100035787233,15.2746084055066));
#9149=CARTESIAN_POINT('Ctrl Pts',(2.18177860318924,-2.28310071890812,15.276228534302));
#9150=CARTESIAN_POINT('Ctrl Pts',(2.01306099467025,-2.11232756960067,15.291631139164));
#9151=CARTESIAN_POINT('Ctrl Pts',(1.8778746534446,-1.94499561999119,15.3062799670444));
#9152=CARTESIAN_POINT('Ctrl Pts',(1.63873268111013,-1.57979345273465,15.335760523392));
#9153=CARTESIAN_POINT('Ctrl Pts',(1.53662570504871,-1.38200353901985,15.3504889999615));
#9154=CARTESIAN_POINT('Ctrl Pts',(1.44400241626756,-1.14550545677039,15.3664998642962));
#9155=CARTESIAN_POINT('Ctrl Pts',(1.43279408778,-1.11558406697368,15.3684991252655));
#9156=CARTESIAN_POINT('Ctrl Pts',(1.41634800651187,-1.06961023670867,15.371531765673));
#9157=CARTESIAN_POINT('Ctrl Pts',(1.41078860101692,-1.05367577409899,15.3725757628642));
#9158=CARTESIAN_POINT('Ctrl Pts',(1.40091075172541,-1.0246322121648,15.3744659844511));
#9159=CARTESIAN_POINT('Ctrl Pts',(1.39655089369322,-1.01153772542836,15.3753135592133));
#9160=CARTESIAN_POINT('Ctrl Pts',(1.38723785354293,-0.982955475485766,15.3771537046914));
#9161=CARTESIAN_POINT('Ctrl Pts',(1.38231748019399,-0.967457360575087,15.3781451787012));
#9162=CARTESIAN_POINT('Ctrl Pts',(1.3691694997775,-0.924930750841023,15.3808489745612));
#9163=CARTESIAN_POINT('Ctrl Pts',(1.36117956201714,-0.897829865947965,15.3825535311901));
#9164=CARTESIAN_POINT('Ctrl Pts',(1.31930693117452,-0.748595398889713,15.3918441941649));
#9165=CARTESIAN_POINT('Ctrl Pts',(1.29229332272023,-0.624642692087423,15.3992051302605));
#9166=CARTESIAN_POINT('Ctrl Pts',(1.23810632496545,-0.279191222249639,15.4191270217043));
#9167=CARTESIAN_POINT('Ctrl Pts',(1.22650555388356,-0.0559962116658821,
15.4313123565139));
#9168=CARTESIAN_POINT('Ctrl Pts',(1.24350940002346,0.272487247807755,15.4500777972967));
#9169=CARTESIAN_POINT('Ctrl Pts',(1.25421206541333,0.378027060073327,15.4562438562687));
#9170=CARTESIAN_POINT('Ctrl Pts',(1.27268806453745,0.499955667475999,15.4637212285154));
#9171=CARTESIAN_POINT('Ctrl Pts',(1.27542016680174,0.517054161047396,15.4647780004967));
#9172=CARTESIAN_POINT('Ctrl Pts',(1.27983162273718,0.543303228168585,15.466414079682));
#9173=CARTESIAN_POINT('Ctrl Pts',(1.28141308503983,0.552470231326708,15.4669880367354));
#9174=CARTESIAN_POINT('Ctrl Pts',(1.28439842666182,0.569338605951417,15.4680491655432));
#9175=CARTESIAN_POINT('Ctrl Pts',(1.28579069763014,0.577041826573964,15.4685356811352));
#9176=CARTESIAN_POINT('Ctrl Pts',(1.28901156523218,0.594498751472163,15.4696425879379));
#9177=CARTESIAN_POINT('Ctrl Pts',(1.2908571447149,0.604249073216228,15.4702639161204));
#9178=CARTESIAN_POINT('Ctrl Pts',(1.29576630894026,0.629544621579493,15.4718835763839));
#9179=CARTESIAN_POINT('Ctrl Pts',(1.29889951367914,0.645075846705851,15.4728856281999));
#9180=CARTESIAN_POINT('Ctrl Pts',(1.3209783302041,0.750503478900806,15.4797364699548));
#9181=CARTESIAN_POINT('Ctrl Pts',(1.34364436939426,0.839569415432615,15.4857648979553));
#9182=CARTESIAN_POINT('Ctrl Pts',(1.45116918186101,1.19735947953262,15.5106570506489));
#9183=CARTESIAN_POINT('Ctrl Pts',(1.56731088601597,1.45543868967549,15.5300570237345));
#9184=CARTESIAN_POINT('Ctrl Pts',(1.74650013688679,1.74517910261711,15.5522316704088));
#9185=CARTESIAN_POINT('Ctrl Pts',(1.77882599492155,1.79438289729783,15.5560191474207));
#9186=CARTESIAN_POINT('Ctrl Pts',(1.83704714393673,1.87792220657212,15.5624874975784));
#9187=CARTESIAN_POINT('Ctrl Pts',(1.86231436145487,1.91267474411123,15.5651903114901));
#9188=CARTESIAN_POINT('Ctrl Pts',(1.89973544563385,1.96203739895868,15.5690486229272));
#9189=CARTESIAN_POINT('Ctrl Pts',(1.91133454074299,1.97706040231578,15.5702255144003));
#9190=CARTESIAN_POINT('Ctrl Pts',(1.93181970906803,2.00311346668988,15.5722714590117));
#9191=CARTESIAN_POINT('Ctrl Pts',(1.94064694636333,2.0141889209122,15.5731428086271));
#9192=CARTESIAN_POINT('Ctrl Pts',(1.95903325834408,2.03694860674731,15.5749368931426));
#9193=CARTESIAN_POINT('Ctrl Pts',(1.96860200889535,2.04862460177561,15.5758592097129));
#9194=CARTESIAN_POINT('Ctrl Pts',(1.99338998167762,2.07844159879424,15.5782198226448));
#9195=CARTESIAN_POINT('Ctrl Pts',(2.00872790470422,2.09648308114642,15.5796532616922));
#9196=CARTESIAN_POINT('Ctrl Pts',(2.07040961426932,2.16743741313799,15.5853133263687));
#9197=CARTESIAN_POINT('Ctrl Pts',(2.11828329299251,2.21899820097414,15.5894764437169));
#9198=CARTESIAN_POINT('Ctrl Pts',(2.39914382956457,2.5022980747393,15.6127525369564));
#9199=CARTESIAN_POINT('Ctrl Pts',(2.66476548795755,2.69885961722462,15.6302771501956));
#9200=CARTESIAN_POINT('Ctrl Pts',(2.99666883167572,2.87354607291331,15.6520626329592));
#9201=CARTESIAN_POINT('Ctrl Pts',(3.0383189194704,2.89432781418454,15.6547987805471));
#9202=CARTESIAN_POINT('Ctrl Pts',(3.10826234086195,2.92735466362218,15.6594211141058));
#9203=CARTESIAN_POINT('Ctrl Pts',(3.13630846254418,2.94010927095211,15.6612817761825));
#9204=CARTESIAN_POINT('Ctrl Pts',(3.17526538630308,2.95715604202562,15.6638819344545));
#9205=CARTESIAN_POINT('Ctrl Pts',(3.18602417479616,2.96179413450565,15.6646016527264));
#9206=CARTESIAN_POINT('Ctrl Pts',(3.20425177444704,2.96953442835968,15.6658241411236));
#9207=CARTESIAN_POINT('Ctrl Pts',(3.2117075407422,2.97266742347229,15.6663250679011));
#9208=CARTESIAN_POINT('Ctrl Pts',(3.22601311531618,2.97861552754672,15.6672880387195));
#9209=CARTESIAN_POINT('Ctrl Pts',(3.23286094785519,2.98143513742272,15.6677497872422));
#9210=CARTESIAN_POINT('Ctrl Pts',(3.24928852999123,2.98813310159381,15.6688592828029));
#9211=CARTESIAN_POINT('Ctrl Pts',(3.25887726665417,2.9919889965436,15.6695083421836));
#9212=CARTESIAN_POINT('Ctrl Pts',(3.2936214155095,3.0057667995058,15.6718649652339));
#9213=CARTESIAN_POINT('Ctrl Pts',(3.3188821243309,3.01541780722588,15.673587410236));
#9214=CARTESIAN_POINT('Ctrl Pts',(3.49891374656644,3.0816159371021,15.685912244743));
#9215=CARTESIAN_POINT('Ctrl Pts',(3.65768640977057,3.1265324128846,15.697024925187));
#9216=CARTESIAN_POINT('Ctrl Pts',(3.95570321320723,3.18665160919139,15.7175893014402));
#9217=CARTESIAN_POINT('Ctrl Pts',(4.09387694156978,3.20531527989227,15.7270126673056));
#9218=CARTESIAN_POINT('Ctrl Pts',(4.323258641263,3.22127138336444,15.7422567663711));
#9219=CARTESIAN_POINT('Ctrl Pts',(4.41391757009788,3.22374410640866,15.7481819746428));
#9220=CARTESIAN_POINT('Ctrl Pts',(4.56379553996563,3.22150700926882,15.757796432196));
#9221=CARTESIAN_POINT('Ctrl Pts',(4.62299141574046,3.21899012709779,15.7615474245602));
#9222=CARTESIAN_POINT('Ctrl Pts',(4.70352972195975,3.21333792889785,15.7665905678146));
#9223=CARTESIAN_POINT('Ctrl Pts',(4.72495669281635,3.21161860203254,15.767926490416));
#9224=CARTESIAN_POINT('Ctrl Pts',(4.76093836755449,3.20836876600046,15.7701605166629));
#9225=CARTESIAN_POINT('Ctrl Pts',(4.77550250593776,3.20695328479521,15.7710621950245));
#9226=CARTESIAN_POINT('Ctrl Pts',(4.80425394586561,3.20396114408532,15.7728373051744));
#9227=CARTESIAN_POINT('Ctrl Pts',(4.81844140237559,3.20238932277656,15.7737108672417));
#9228=CARTESIAN_POINT('Ctrl Pts',(4.85289422398696,3.19834042691797,15.7758267007739));
#9229=CARTESIAN_POINT('Ctrl Pts',(4.87314756679253,3.1957649241662,15.777065852861));
#9230=CARTESIAN_POINT('Ctrl Pts',(4.93062448544956,3.18790020372233,15.7805701413381));
#9231=CARTESIAN_POINT('Ctrl Pts',(4.96778258405081,3.18215174611032,15.7828208874788));
#9232=CARTESIAN_POINT('Ctrl Pts',(5.21316504250359,3.13978107849448,15.7976033829535));
#9233=CARTESIAN_POINT('Ctrl Pts',(5.41745873030948,3.08339525977471,15.8094782179626));
#9234=CARTESIAN_POINT('Ctrl Pts',(5.80274165822397,2.93500252859362,15.8325659842394));
#9235=CARTESIAN_POINT('Ctrl Pts',(5.98348285575964,2.84515349319922,15.8437480808564));
#9236=CARTESIAN_POINT('Ctrl Pts',(6.18199055873875,2.72208181252755,15.857688050087));
#9237=CARTESIAN_POINT('Ctrl Pts',(6.20909121548159,2.70471241350369,15.8596302339857));
#9238=CARTESIAN_POINT('Ctrl Pts',(6.2458620876556,2.68036048827521,15.8623260277433));
#9239=CARTESIAN_POINT('Ctrl Pts',(6.25576143949166,2.67372524358928,15.8630579042713));
#9240=CARTESIAN_POINT('Ctrl Pts',(6.27234954527477,2.66247288219343,15.8642950368265));
#9241=CARTESIAN_POINT('Ctrl Pts',(6.27905816691606,2.65788501087693,15.8647983454083));
#9242=CARTESIAN_POINT('Ctrl Pts',(6.29181241666764,2.64909168023801,15.8657610664351));
#9243=CARTESIAN_POINT('Ctrl Pts',(6.29786110274209,2.64489079360161,15.866220153304));
#9244=CARTESIAN_POINT('Ctrl Pts',(6.31223395401858,2.63483547095914,15.8673169395816));
#9245=CARTESIAN_POINT('Ctrl Pts',(6.32054483272826,2.62896230643553,15.8679558863853));
#9246=CARTESIAN_POINT('Ctrl Pts',(6.34998446106017,2.60794801412565,15.8702357492567));
#9247=CARTESIAN_POINT('Ctrl Pts',(6.37095704520445,2.59259118943021,15.8718903340276));
#9248=CARTESIAN_POINT('Ctrl Pts',(6.55531774909965,2.45413934154408,15.8866906939704));
#9249=CARTESIAN_POINT('Ctrl Pts',(6.70681294335107,2.31601053395622,15.9006226174699));
#9250=CARTESIAN_POINT('Ctrl Pts',(6.95076845518491,2.04689358348651,15.9251721949746));
#9251=CARTESIAN_POINT('Ctrl Pts',(7.04853299112394,1.92159232861858,15.9358060395362));
#9252=CARTESIAN_POINT('Ctrl Pts',(7.18434943544674,1.71818436432412,15.9517045869608));
#9253=CARTESIAN_POINT('Ctrl Pts',(7.22915534981766,1.64490176510289,15.9571899674633));
#9254=CARTESIAN_POINT('Ctrl Pts',(7.28292755144546,1.54849969638027,15.9641055038649));
#9255=CARTESIAN_POINT('Ctrl Pts',(7.29462621547439,1.52695216979027,15.9656327383442));
#9256=CARTESIAN_POINT('Ctrl Pts',(7.31321419106842,1.49176355521575,15.9680974879967));
#9257=CARTESIAN_POINT('Ctrl Pts',(7.32025420768364,1.47820360232922,15.9690403089542));
#9258=CARTESIAN_POINT('Ctrl Pts',(7.3336031132064,1.45203861313983,15.9708463948364));
#9259=CARTESIAN_POINT('Ctrl Pts',(7.33992624175181,1.43944127553771,15.971710144428));
#9260=CARTESIAN_POINT('Ctrl Pts',(7.35423364050562,1.41046456113806,15.9736839093621));
#9261=CARTESIAN_POINT('Ctrl Pts',(7.36216209700713,1.39405804715089,15.974791963404));
#9262=CARTESIAN_POINT('Ctrl Pts',(7.38698202081989,1.34156589152543,15.9783077808639));
#9263=CARTESIAN_POINT('Ctrl Pts',(7.4033440510622,1.30523302658718,15.9806973455743));
#9264=CARTESIAN_POINT('Ctrl Pts',(7.5193582668769,1.03430624520518,15.99821559639));
#9265=CARTESIAN_POINT('Ctrl Pts',(7.59154100052254,0.788934775008786,16.0123398231549));
#9266=CARTESIAN_POINT('Ctrl Pts',(7.66416188569981,0.359695869536868,16.0367207869367));
#9267=CARTESIAN_POINT('Ctrl Pts',(7.67926286618053,0.179600130261551,16.0468902667977));
#9268=CARTESIAN_POINT('Ctrl Pts',(7.6792190109727,-0.000783520933935085,
16.0578089001435));
#9269=CARTESIAN_POINT('Ctrl Pts',(7.67921910621823,-2.74841093364834E-11,
15.8122671767608));
#9270=CARTESIAN_POINT('Ctrl Pts',(7.67921910621895,0.0842650733278685,15.8067022814364));
#9271=CARTESIAN_POINT('Ctrl Pts',(7.67591422296171,0.168504703978227,15.801214720458));
#9272=CARTESIAN_POINT('Ctrl Pts',(7.66563399803438,0.299298265355216,15.7928221212079));
#9273=CARTESIAN_POINT('Ctrl Pts',(7.66093664709852,0.345986854884521,15.7898514449779));
#9274=CARTESIAN_POINT('Ctrl Pts',(7.65302786761198,0.410431366001335,15.7857844094348));
#9275=CARTESIAN_POINT('Ctrl Pts',(7.65068464403456,0.428286049699491,15.7846611645038));
#9276=CARTESIAN_POINT('Ctrl Pts',(7.64628536217112,0.459760257945463,15.7826871631853));
#9277=CARTESIAN_POINT('Ctrl Pts',(7.64429143132403,0.473387868997891,15.7818344736633));
#9278=CARTESIAN_POINT('Ctrl Pts',(7.64018893903769,0.500224444763774,15.7801591172514));
#9279=CARTESIAN_POINT('Ctrl Pts',(7.63808538195312,0.513433882381725,15.7793363103066));
#9280=CARTESIAN_POINT('Ctrl Pts',(7.63343583664471,0.54150464592363,15.7775915504833));
#9281=CARTESIAN_POINT('Ctrl Pts',(7.63086766532932,0.556362011489941,15.7766703214067));
#9282=CARTESIAN_POINT('Ctrl Pts',(7.62401251917557,0.594426801702553,15.7743155707005));
#9283=CARTESIAN_POINT('Ctrl Pts',(7.61957467945073,0.617606406591507,15.7728868599203));
#9284=CARTESIAN_POINT('Ctrl Pts',(7.60102989959306,0.709020207630493,15.7672709705227));
#9285=CARTESIAN_POINT('Ctrl Pts',(7.58496580574802,0.776840836270749,15.7631460077259));
#9286=CARTESIAN_POINT('Ctrl Pts',(7.54167806563526,0.936344328961776,15.7534995467753));
#9287=CARTESIAN_POINT('Ctrl Pts',(7.51254823862863,1.02744207392575,15.7480348531459));
#9288=CARTESIAN_POINT('Ctrl Pts',(7.43390192305887,1.24026101818886,15.7352108874529));
#9289=CARTESIAN_POINT('Ctrl Pts',(7.38091148706979,1.36051118353049,15.7279206843769));
#9290=CARTESIAN_POINT('Ctrl Pts',(7.24567551781377,1.62273230924428,15.7113667334707));
#9291=CARTESIAN_POINT('Ctrl Pts',(7.15964302471967,1.76231927900727,15.7020852857202));
#9292=CARTESIAN_POINT('Ctrl Pts',(7.0514954424338,1.91111627420558,15.6909718891952));
#9293=CARTESIAN_POINT('Ctrl Pts',(7.039443945683,1.92737334999577,15.689740095815));
#9294=CARTESIAN_POINT('Ctrl Pts',(7.02126984890355,1.95141300962047,15.6878904860991));
#9295=CARTESIAN_POINT('Ctrl Pts',(7.0152629300453,1.95928296702558,15.6872804180134));
#9296=CARTESIAN_POINT('Ctrl Pts',(7.00490123341382,1.97272940774302,15.6862299938113));
#9297=CARTESIAN_POINT('Ctrl Pts',(7.0005642163603,1.97831941111292,15.6857908864));
#9298=CARTESIAN_POINT('Ctrl Pts',(6.99066122321391,1.99099700843951,15.6847894581584));
#9299=CARTESIAN_POINT('Ctrl Pts',(6.98508401189751,1.99807543090164,15.6842263536444));
#9300=CARTESIAN_POINT('Ctrl Pts',(6.96980018926268,2.01730670473776,15.6826858336296));
#9301=CARTESIAN_POINT('Ctrl Pts',(6.96003531502426,2.02941264642906,15.6817044342856));
#9302=CARTESIAN_POINT('Ctrl Pts',(6.91040666148698,2.0900361528138,15.6767328374561));
#9303=CARTESIAN_POINT('Ctrl Pts',(6.86922116389314,2.13744870580446,15.6726592925865));
#9304=CARTESIAN_POINT('Ctrl Pts',(6.78609401677653,2.22767892795889,15.6645855040948));
#9305=CARTESIAN_POINT('Ctrl Pts',(6.74428883167371,2.27059153463945,15.6605919620065));
#9306=CARTESIAN_POINT('Ctrl Pts',(6.56128389896565,2.44825685468741,15.643469474081));
#9307=CARTESIAN_POINT('Ctrl Pts',(6.40918306970307,2.57121039353712,15.6301415999972));
#9308=CARTESIAN_POINT('Ctrl Pts',(6.16913421937717,2.73160046180395,15.6109759102717));
#9309=CARTESIAN_POINT('Ctrl Pts',(6.08914780985128,2.7801484985049,15.6048554815705));
#9310=CARTESIAN_POINT('Ctrl Pts',(5.97148072336591,2.84473436462652,15.5962396788252));
#9311=CARTESIAN_POINT('Ctrl Pts',(5.93543569516697,2.86363962000486,15.5936500060045));
#9312=CARTESIAN_POINT('Ctrl Pts',(5.87046681988051,2.8961610955757,15.589069118269));
#9313=CARTESIAN_POINT('Ctrl Pts',(5.84168080312052,2.91003905448762,15.5870691243747));
#9314=CARTESIAN_POINT('Ctrl Pts',(5.79746827482951,2.93054951192893,15.5840413399687));
#9315=CARTESIAN_POINT('Ctrl Pts',(5.78218910390708,2.93749310073453,15.5830028820373));
#9316=CARTESIAN_POINT('Ctrl Pts',(5.76674005434707,2.94436879842505,15.5819606821606));
#9317=CARTESIAN_POINT('Ctrl Pts',(5.76662395001161,2.94442046316999,15.581952850152));
#9318=CARTESIAN_POINT('Ctrl Pts',(5.76638363535373,2.94452738267807,15.5819366402476));
#9319=CARTESIAN_POINT('Ctrl Pts',(5.76625942459416,2.94458263644781,15.5819282623862));
#9320=CARTESIAN_POINT('Ctrl Pts',(5.76600230474415,2.94469699385462,15.5819109210194));
#9321=CARTESIAN_POINT('Ctrl Pts',(5.76586939511761,2.9447560963666,15.5819019575512));
#9322=CARTESIAN_POINT('Ctrl Pts',(5.76559423873709,2.94487843113088,15.581883402115));
#9323=CARTESIAN_POINT('Ctrl Pts',(5.76545199140813,2.94494166207284,15.5818738101925));
#9324=CARTESIAN_POINT('Ctrl Pts',(5.76515747047517,2.94507255522234,15.581853951636));
#9325=CARTESIAN_POINT('Ctrl Pts',(5.76500519620537,2.94514021592632,15.5818436850538));
#9326=CARTESIAN_POINT('Ctrl Pts',(5.76468987762537,2.94528029355213,15.5818224273288));
#9327=CARTESIAN_POINT('Ctrl Pts',(5.76452683253783,2.94535270875038,15.5818114362448));
#9328=CARTESIAN_POINT('Ctrl Pts',(5.76418916926002,2.94550264568189,15.581788675722));
#9329=CARTESIAN_POINT('Ctrl Pts',(5.76401455018736,2.94558016542695,15.5817769063515));
#9330=CARTESIAN_POINT('Ctrl Pts',(5.7636528715537,2.94574068920268,15.5817525311862));
#9331=CARTESIAN_POINT('Ctrl Pts',(5.76346581097887,2.9458236909438,15.5817399254702));
#9332=CARTESIAN_POINT('Ctrl Pts',(5.76307831220833,2.94599558611335,15.5817138149134));
#9333=CARTESIAN_POINT('Ctrl Pts',(5.76287787282165,2.94608447691495,15.5817003101619));
#9334=CARTESIAN_POINT('Ctrl Pts',(5.76246260363558,2.94626858966093,15.5816723338166));
#9335=CARTESIAN_POINT('Ctrl Pts',(5.76224777249714,2.946363808563,15.5816578623279));
#9336=CARTESIAN_POINT('Ctrl Pts',(5.76180262511463,2.94656105153108,15.5816278793665));
#9337=CARTESIAN_POINT('Ctrl Pts',(5.76157230729521,2.9466630721026,15.5816123680128));
#9338=CARTESIAN_POINT('Ctrl Pts',(5.76109500319871,2.94687442969405,15.5815802263163));
#9339=CARTESIAN_POINT('Ctrl Pts',(5.76084801514135,2.94698376266537,15.5815635961131));
#9340=CARTESIAN_POINT('Ctrl Pts',(5.76033609148587,2.94721029639146,15.5815291313911));
#9341=CARTESIAN_POINT('Ctrl Pts',(5.76007115381155,2.94732749248152,15.581511297032));
#9342=CARTESIAN_POINT('Ctrl Pts',(5.7470510905882,2.95308486314133,15.5806349601208));
#9343=CARTESIAN_POINT('Ctrl Pts',(5.73425934784724,2.95864228580718,15.579779299626));
#9344=CARTESIAN_POINT('Ctrl Pts',(5.70561996261436,2.97086439389849,15.5778751900898));
#9345=CARTESIAN_POINT('Ctrl Pts',(5.68975418130527,2.97748569272211,15.5768282328901));
#9346=CARTESIAN_POINT('Ctrl Pts',(5.64943271995649,2.9939355390484,15.5741869292169));
#9347=CARTESIAN_POINT('Ctrl Pts',(5.62490777208991,3.00359174022535,15.5725983827072));
#9348=CARTESIAN_POINT('Ctrl Pts',(5.47281146318484,3.06133169274663,15.5628522427458));
#9349=CARTESIAN_POINT('Ctrl Pts',(5.34240645678249,3.10158425330213,15.5549595961868));
#9350=CARTESIAN_POINT('Ctrl Pts',(5.00100358647835,3.18366601698323,15.5350179954092));
#9351=CARTESIAN_POINT('Ctrl Pts',(4.78769233542449,3.21286967120153,15.5232619013929));
#9352=CARTESIAN_POINT('Ctrl Pts',(4.46963093309053,3.22438492671661,15.5050854832484));
#9353=CARTESIAN_POINT('Ctrl Pts',(4.36608115169072,3.22314395226207,15.4990592922793));
#9354=CARTESIAN_POINT('Ctrl Pts',(4.245588507109,3.21588924404218,15.4917392925464));
#9355=CARTESIAN_POINT('Ctrl Pts',(4.22840382921732,3.21471623265909,15.4906879652083));
#9356=CARTESIAN_POINT('Ctrl Pts',(4.20197411440329,3.21269918115946,15.4890586000215));
#9357=CARTESIAN_POINT('Ctrl Pts',(4.19272164290768,3.21195283278537,15.4884858445347));
#9358=CARTESIAN_POINT('Ctrl Pts',(4.17567192684417,3.21050335583172,15.4874258711806));
#9359=CARTESIAN_POINT('Ctrl Pts',(4.16787390269243,3.20981177924335,15.4869392995582));
#9360=CARTESIAN_POINT('Ctrl Pts',(4.15017427637304,3.20817704771718,15.4858308932224));
#9361=CARTESIAN_POINT('Ctrl Pts',(4.14027452628728,3.20721646817218,15.4852081098509));
#9362=CARTESIAN_POINT('Ctrl Pts',(4.11453934901997,3.20459905614654,15.4835820514084));
#9363=CARTESIAN_POINT('Ctrl Pts',(4.09871168692683,3.20287069276456,15.4825750089276));
#9364=CARTESIAN_POINT('Ctrl Pts',(3.98973828446636,3.19015310143718,15.4755963594086));
#9365=CARTESIAN_POINT('Ctrl Pts',(3.89710632796835,3.17522036171682,15.4694376110368));
#9366=CARTESIAN_POINT('Ctrl Pts',(3.53108585644918,3.09970301145523,15.4445203084541));
#9367=CARTESIAN_POINT('Ctrl Pts',(3.26538928753086,3.00763378006678,15.4252525225651));
#9368=CARTESIAN_POINT('Ctrl Pts',(2.96243440968215,2.85612045319719,15.4032067467837));
#9369=CARTESIAN_POINT('Ctrl Pts',(2.91065529717274,2.82843138130871,15.3994295612968));
#9370=CARTESIAN_POINT('Ctrl Pts',(2.82241784803954,2.77809866740508,15.3929769716587));
#9371=CARTESIAN_POINT('Ctrl Pts',(2.78560316788573,2.75611375322189,15.3902797679413));
#9372=CARTESIAN_POINT('Ctrl Pts',(2.73315350411069,2.7233546359667,15.3864280131561));
#9373=CARTESIAN_POINT('Ctrl Pts',(2.71715904636012,2.71316746221537,15.3852521669152));
#9374=CARTESIAN_POINT('Ctrl Pts',(2.68938066882154,2.69512828705432,15.3832075077371));
#9375=CARTESIAN_POINT('Ctrl Pts',(2.67755698112068,2.68733877481257,15.38233640583));
#9376=CARTESIAN_POINT('Ctrl Pts',(2.65323081725135,2.67108165899843,15.3805423428934));
#9377=CARTESIAN_POINT('Ctrl Pts',(2.64073572875639,2.66260358859132,15.3796198034592));
#9378=CARTESIAN_POINT('Ctrl Pts',(2.60878153733425,2.64059273145671,15.3772576082841));
#9379=CARTESIAN_POINT('Ctrl Pts',(2.58941108920564,2.62693238067609,15.3758228237256));
#9380=CARTESIAN_POINT('Ctrl Pts',(2.51299407515785,2.57176960231916,15.3701490248023));
#9381=CARTESIAN_POINT('Ctrl Pts',(2.45716381579259,2.52861098679474,15.3659739288738));
#9382=CARTESIAN_POINT('Ctrl Pts',(2.14974972054736,2.27441704651301,15.3427019931669));
#9383=CARTESIAN_POINT('Ctrl Pts',(1.93020425142487,2.02777595095433,15.3251892232104));
#9384=CARTESIAN_POINT('Ctrl Pts',(1.72640961500678,1.71320111798867,15.3034178980689));
#9385=CARTESIAN_POINT('Ctrl Pts',(1.70195892173451,1.67360572222976,15.3006823438617));
#9386=CARTESIAN_POINT('Ctrl Pts',(1.66276178985039,1.60694302366897,15.2960609581086));
#9387=CARTESIAN_POINT('Ctrl Pts',(1.64753049301144,1.58016776312746,15.2942006386201));
#9388=CARTESIAN_POINT('Ctrl Pts',(1.62704028672539,1.54291521021326,15.2916009297953));
#9389=CARTESIAN_POINT('Ctrl Pts',(1.62145071305986,1.53262046544368,15.2908813108477));
#9390=CARTESIAN_POINT('Ctrl Pts',(1.61209782512665,1.51516829658132,15.2896589815691));
#9391=CARTESIAN_POINT('Ctrl Pts',(1.60830502975869,1.50802663885232,15.2891581140091));
#9392=CARTESIAN_POINT('Ctrl Pts',(1.6010906341844,1.49431796358418,15.2881952516157));
#9393=CARTESIAN_POINT('Ctrl Pts',(1.59766473139471,1.48775331917547,15.2877335521962));
#9394=CARTESIAN_POINT('Ctrl Pts',(1.5895119862195,1.47199905822171,15.2866241703193));
#9395=CARTESIAN_POINT('Ctrl Pts',(1.58480669625066,1.46279846584081,15.285975175754));
#9396=CARTESIAN_POINT('Ctrl Pts',(1.56795010939538,1.42944279101816,15.2836187565137));
#9397=CARTESIAN_POINT('Ctrl Pts',(1.55605906122965,1.40515840653327,15.2818964526451));
#9398=CARTESIAN_POINT('Ctrl Pts',(1.47386999824014,1.2318194203206,15.2695703299018));
#9399=CARTESIAN_POINT('Ctrl Pts',(1.41479711571852,1.07772802551118,15.258456065562));
#9400=CARTESIAN_POINT('Ctrl Pts',(1.32800902907146,0.786296812171222,15.2378876730981));
#9401=CARTESIAN_POINT('Ctrl Pts',(1.29694487400604,0.650335241337894,15.2284618734336));
#9402=CARTESIAN_POINT('Ctrl Pts',(1.26035818069816,0.423324305142609,15.2132177361621));
#9403=CARTESIAN_POINT('Ctrl Pts',(1.2497186671456,0.333290381493073,15.2072947245123));
#9404=CARTESIAN_POINT('Ctrl Pts',(1.23842372552297,0.18387052768763,15.1976834727894));
#9405=CARTESIAN_POINT('Ctrl Pts',(1.23558820930995,0.124705389878211,15.1939335383011));
#9406=CARTESIAN_POINT('Ctrl Pts',(1.23394789713065,0.0440056078309579,15.1888916571596));
#9407=CARTESIAN_POINT('Ctrl Pts',(1.23372608710336,0.022514555349209,15.1875559641337));
#9408=CARTESIAN_POINT('Ctrl Pts',(1.23371462666001,-0.0136080604199647,
15.1853222826256));
#9409=CARTESIAN_POINT('Ctrl Pts',(1.23380961358421,-0.028238636685241,15.1844207208913));
#9410=CARTESIAN_POINT('Ctrl Pts',(1.23419408043649,-0.0571395324266167,
15.1826458122114));
#9411=CARTESIAN_POINT('Ctrl Pts',(1.23447873509014,-0.071409569521203,15.1817723352036));
#9412=CARTESIAN_POINT('Ctrl Pts',(1.23540090362008,-0.106084609192493,15.1796566613541));
#9413=CARTESIAN_POINT('Ctrl Pts',(1.23613752408481,-0.126486524131578,15.1784175837259));
#9414=CARTESIAN_POINT('Ctrl Pts',(1.23878143162324,-0.184437054822519,15.1749133950307));
#9415=CARTESIAN_POINT('Ctrl Pts',(1.24115200196418,-0.221961917583025,15.1726626744533));
#9416=CARTESIAN_POINT('Ctrl Pts',(1.26118947499137,-0.470060513455625,15.1578865352414));
#9417=CARTESIAN_POINT('Ctrl Pts',(1.29887326188963,-0.678506233941155,15.1460172901386));
#9418=CARTESIAN_POINT('Ctrl Pts',(1.41183853977395,-1.07561864602565,15.1229297176025));
#9419=CARTESIAN_POINT('Ctrl Pts',(1.48503205391908,-1.26383240288843,15.1117423904982));
#9420=CARTESIAN_POINT('Ctrl Pts',(1.58972850894977,-1.47273635848952,15.0977960627004));
#9421=CARTESIAN_POINT('Ctrl Pts',(1.60458301744071,-1.50129930081596,15.0958535504836));
#9422=CARTESIAN_POINT('Ctrl Pts',(1.62551873410921,-1.54012323530385,15.0931574200188));
#9423=CARTESIAN_POINT('Ctrl Pts',(1.63123324774054,-1.55058115650156,15.0924255436778));
#9424=CARTESIAN_POINT('Ctrl Pts',(1.64094190856478,-1.56811677064882,15.0911884506177));
#9425=CARTESIAN_POINT('Ctrl Pts',(1.64490513200767,-1.57521161241637,15.0906851816082));
#9426=CARTESIAN_POINT('Ctrl Pts',(1.65251033542968,-1.5887060750483,15.0897225699942));
#9427=CARTESIAN_POINT('Ctrl Pts',(1.65614748294632,-1.59510833012601,15.089263553099));
#9428=CARTESIAN_POINT('Ctrl Pts',(1.66584804882955,-1.61204822646685,15.088042982752));
#9429=CARTESIAN_POINT('Ctrl Pts',(1.67194914113431,-1.62256399669117,15.0872790611312));
#9430=CARTESIAN_POINT('Ctrl Pts',(1.69399197097058,-1.66006628005071,15.0845330333729));
#9431=CARTESIAN_POINT('Ctrl Pts',(1.71026715505651,-1.68685347632025,15.0825312300784));
#9432=CARTESIAN_POINT('Ctrl Pts',(1.91071337332961,-2.00617560505691,15.0582177944138));
#9433=CARTESIAN_POINT('Ctrl Pts',(2.1404070534296,-2.26749335729481,15.0340251349315));
#9434=CARTESIAN_POINT('Ctrl Pts',(2.45578973674155,-2.52732103489233,15.0073554035512));
#9435=CARTESIAN_POINT('Ctrl Pts',(2.5054709995015,-2.56586764738827,15.0033012270454));
#9436=CARTESIAN_POINT('Ctrl Pts',(2.59273778996224,-2.62957485938873,14.9964280145181));
#9437=CARTESIAN_POINT('Ctrl Pts',(2.62978213844828,-2.65544222578176,14.9935831812708));
#9438=CARTESIAN_POINT('Ctrl Pts',(2.68346117704979,-2.69127018339964,14.9895614587708));
#9439=CARTESIAN_POINT('Ctrl Pts',(2.69965945746288,-2.70187198090747,14.9883605837713));
#9440=CARTESIAN_POINT('Ctrl Pts',(2.72792374800866,-2.72000934353825,14.9862868210935));
#9441=CARTESIAN_POINT('Ctrl Pts',(2.73994580118056,-2.72761207613919,14.985411451434));
#9442=CARTESIAN_POINT('Ctrl Pts',(2.76471278104889,-2.7430460881605,14.9836215745742));
#9443=CARTESIAN_POINT('Ctrl Pts',(2.77746269929537,-2.75086873603203,14.9827074000755));
#9444=CARTESIAN_POINT('Ctrl Pts',(2.80999427006611,-2.77051788077464,14.9803929080917));
#9445=CARTESIAN_POINT('Ctrl Pts',(2.82984937697306,-2.78222159658008,14.9789970796022));
#9446=CARTESIAN_POINT('Ctrl Pts',(2.90658767378477,-2.82635315558743,14.9736644679125));
#9447=CARTESIAN_POINT('Ctrl Pts',(2.96433078833044,-2.85725895431166,14.9697820308718));
#9448=CARTESIAN_POINT('Ctrl Pts',(3.32247991218538,-3.03512963210773,14.9463899944093));
#9449=CARTESIAN_POINT('Ctrl Pts',(3.64325821590194,-3.13633417607138,14.9285747587303));
#9450=CARTESIAN_POINT('Ctrl Pts',(4.02008067259177,-3.19341050709871,14.9064421129961));
#9451=CARTESIAN_POINT('Ctrl Pts',(4.06647367522107,-3.19940754882225,14.9036928030104));
#9452=CARTESIAN_POINT('Ctrl Pts',(4.14372488350597,-3.20768839261889,14.8990503451401));
#9453=CARTESIAN_POINT('Ctrl Pts',(4.17451595613227,-3.21054139265349,14.8971830082216));
#9454=CARTESIAN_POINT('Ctrl Pts',(4.21703837289087,-3.21386498274025,14.8945750542911));
#9455=CARTESIAN_POINT('Ctrl Pts',(4.22873943842849,-3.21471528939506,14.8938543723607));
#9456=CARTESIAN_POINT('Ctrl Pts',(4.24851629089258,-3.21604394157425,14.8926307661192));
#9457=CARTESIAN_POINT('Ctrl Pts',(4.25658985448087,-3.2165558118103,14.8921296936226));
#9458=CARTESIAN_POINT('Ctrl Pts',(4.27205319839246,-3.21747775621718,14.8911668677404));
#9459=CARTESIAN_POINT('Ctrl Pts',(4.27944258868239,-3.21789278073207,14.8907054124554));
#9460=CARTESIAN_POINT('Ctrl Pts',(4.2971386335242,-3.21882554029774,14.8895971871766));
#9461=CARTESIAN_POINT('Ctrl Pts',(4.30744639851509,-3.21931922682238,14.8889491110005));
#9462=CARTESIAN_POINT('Ctrl Pts',(4.34466342420592,-3.22092259996151,14.8866004204136));
#9463=CARTESIAN_POINT('Ctrl Pts',(4.37158312577784,-3.22174442899836,14.8848850541916));
#9464=CARTESIAN_POINT('Ctrl Pts',(4.56786252687139,-3.22527502584141,14.8722726155126));
#9465=CARTESIAN_POINT('Ctrl Pts',(4.73717708900132,-3.21496496372012,14.8608360994689));
#9466=CARTESIAN_POINT('Ctrl Pts',(5.05310408032427,-3.17057545326413,14.8392539426337));
#9467=CARTESIAN_POINT('Ctrl Pts',(5.199708300608,-3.13944634936555,14.8291373703244));
#9468=CARTESIAN_POINT('Ctrl Pts',(5.46218627721138,-3.06428781011458,14.8111190377832));
#9469=CARTESIAN_POINT('Ctrl Pts',(5.57871160574097,-3.02355832609254,14.8031532030418));
#9470=CARTESIAN_POINT('Ctrl Pts',(5.71786186011325,-2.96576338706664,14.7936901044114));
#9471=CARTESIAN_POINT('Ctrl Pts',(5.74296188909585,-2.95496202025116,14.7919848855101));
#9472=CARTESIAN_POINT('Ctrl Pts',(5.782437464662,-2.93737603721723,14.7893051412287));
#9473=CARTESIAN_POINT('Ctrl Pts',(5.79690495793689,-2.93080224742148,14.7883234850033));
#9474=CARTESIAN_POINT('Ctrl Pts',(5.82399288132301,-2.91825140470405,14.7864861402352));
#9475=CARTESIAN_POINT('Ctrl Pts',(5.83662418452835,-2.91229883529384,14.7856296360118));
#9476=CARTESIAN_POINT('Ctrl Pts',(5.86492411355093,-2.89873687043178,14.7837110694565));
#9477=CARTESIAN_POINT('Ctrl Pts',(5.88057061663662,-2.89108212581976,14.7826506062509));
#9478=CARTESIAN_POINT('Ctrl Pts',(5.92039992286234,-2.87119461632867,14.7799513276929));
#9479=CARTESIAN_POINT('Ctrl Pts',(5.94449218191281,-2.85878284492059,14.7783187724842));
#9480=CARTESIAN_POINT('Ctrl Pts',(6.11130550442123,-2.77016428376176,14.7670103771462));
#9481=CARTESIAN_POINT('Ctrl Pts',(6.24827579829929,-2.68360428669593,14.757717259926));
#9482=CARTESIAN_POINT('Ctrl Pts',(6.55001980411922,-2.45946846696826,14.7365140861951));
#9483=CARTESIAN_POINT('Ctrl Pts',(6.70870252099457,-2.31503184665385,14.7247919159305));
#9484=CARTESIAN_POINT('Ctrl Pts',(6.88739626311304,-2.11648964026712,14.7093604353198));
#9485=CARTESIAN_POINT('Ctrl Pts',(6.92192467792707,-2.07616556722218,14.7062548041627));
#9486=CARTESIAN_POINT('Ctrl Pts',(6.97686161792159,-2.00870357477332,14.7010703204091));
#9487=CARTESIAN_POINT('Ctrl Pts',(6.99786589367853,-1.98206221511699,14.6990256433661));
#9488=CARTESIAN_POINT('Ctrl Pts',(7.02582199529364,-1.94542827489513,14.6962100995476));
#9489=CARTESIAN_POINT('Ctrl Pts',(7.03314433129875,-1.93571955997157,14.6954635551285));
#9490=CARTESIAN_POINT('Ctrl Pts',(7.04529794709878,-1.91941388284454,14.6942086935522));
#9491=CARTESIAN_POINT('Ctrl Pts',(7.05015946581625,-1.91283944355455,14.693702451636));
#9492=CARTESIAN_POINT('Ctrl Pts',(7.05932510815806,-1.90034517006326,14.6927396914844));
#9493=CARTESIAN_POINT('Ctrl Pts',(7.06363418534541,-1.89442903795944,14.6922835333995));
#9494=CARTESIAN_POINT('Ctrl Pts',(7.07378290543782,-1.88039518146651,14.6912008966535));
#9495=CARTESIAN_POINT('Ctrl Pts',(7.07960495222912,-1.87226490893535,14.6905732421793));
#9496=CARTESIAN_POINT('Ctrl Pts',(7.09982085610025,-1.84375475980464,14.6883710878591));
#9497=CARTESIAN_POINT('Ctrl Pts',(7.11401538606175,-1.82323552237407,14.6867840688754));
#9498=CARTESIAN_POINT('Ctrl Pts',(7.25253334520598,-1.61794305703171,14.6709019690701));
#9499=CARTESIAN_POINT('Ctrl Pts',(7.35761598225156,-1.42093211674223,14.6556723181389));
#9500=CARTESIAN_POINT('Ctrl Pts',(7.52210694239558,-1.01669585332977,14.6262221739974));
#9501=CARTESIAN_POINT('Ctrl Pts',(7.58278629138018,-0.811157564302041,14.6120634215929));
#9502=CARTESIAN_POINT('Ctrl Pts',(7.62872200634747,-0.56919517407018,14.5965321715331));
#9503=CARTESIAN_POINT('Ctrl Pts',(7.63429525706737,-0.537208234686814,14.5944999931617));
#9504=CARTESIAN_POINT('Ctrl Pts',(7.64204608195944,-0.488370007483515,14.5914281901282));
#9505=CARTESIAN_POINT('Ctrl Pts',(7.64457523520442,-0.471577417362987,14.5903775195629));
#9506=CARTESIAN_POINT('Ctrl Pts',(7.64874768915267,-0.442304685051345,14.5885554096294));
#9507=CARTESIAN_POINT('Ctrl Pts',(7.65045080476814,-0.429833574697313,14.5877820986514));
#9508=CARTESIAN_POINT('Ctrl Pts',(7.65411850280738,-0.401750517229236,14.5860472468449));
#9509=CARTESIAN_POINT('Ctrl Pts',(7.65604190868923,-0.38613344458636,14.585087021143));
#9510=CARTESIAN_POINT('Ctrl Pts',(7.66090994278541,-0.344070496015452,14.5825125617611));
#9511=CARTESIAN_POINT('Ctrl Pts',(7.66364159074693,-0.317600850537358,14.5809050343077));
#9512=CARTESIAN_POINT('Ctrl Pts',(7.67482275501954,-0.194320799569486,14.5734726957604));
#9513=CARTESIAN_POINT('Ctrl Pts',(7.67921910621768,-0.0971890396789468,
14.5677751526768));
#9514=CARTESIAN_POINT('Ctrl Pts',(7.67921910621823,-1.84544675223763E-11,
14.5621759541225));
#9515=CARTESIAN_POINT('Origin',(4.45646910621825,-5.13094777615093E-16,
-2.31077344927308));
#9516=CARTESIAN_POINT('',(7.67921910621823,-2.34781276219209E-11,13.3169799747702));
#9517=CARTESIAN_POINT('',(7.67921910621823,1.97331828652831E-11,13.5632093210196));
#9518=CARTESIAN_POINT('',(7.67921910621823,-3.51191647465084E-13,-2.31077344927308));
#9519=CARTESIAN_POINT('Ctrl Pts',(7.67921910621823,1.97331828652831E-11,
13.5632093210196));
#9520=CARTESIAN_POINT('Ctrl Pts',(7.67921910621822,-0.0872823144129474,
13.568890915301));
#9521=CARTESIAN_POINT('Ctrl Pts',(7.67567332283278,-0.174534833379368,13.5744749122219));
#9522=CARTESIAN_POINT('Ctrl Pts',(7.66650491624969,-0.287135839366412,13.5815600653288));
#9523=CARTESIAN_POINT('Ctrl Pts',(7.66411522062897,-0.312703306593041,13.583160841812));
#9524=CARTESIAN_POINT('Ctrl Pts',(7.65979000297505,-0.353686357435978,13.5857145189396));
#9525=CARTESIAN_POINT('Ctrl Pts',(7.6580481884606,-0.369120848326992,13.5866734535385));
#9526=CARTESIAN_POINT('Ctrl Pts',(7.65452124211246,-0.398468098647805,13.5884916497737));
#9527=CARTESIAN_POINT('Ctrl Pts',(7.65275673681869,-0.412382931066173,13.5893515379531));
#9528=CARTESIAN_POINT('Ctrl Pts',(7.64851855997497,-0.444142289377875,13.5913093328706));
#9529=CARTESIAN_POINT('Ctrl Pts',(7.64598598158508,-0.461978582462665,13.5924053585139));
#9530=CARTESIAN_POINT('Ctrl Pts',(7.63769445834384,-0.517051740537311,13.595779447273));
#9531=CARTESIAN_POINT('Ctrl Pts',(7.6314318304972,-0.554210358562995,13.5980416257949));
#9532=CARTESIAN_POINT('Ctrl Pts',(7.59762418271365,-0.735358737667528,13.6090114158656));
#9533=CARTESIAN_POINT('Ctrl Pts',(7.56092703528893,-0.877471202577492,13.6174257117409));
#9534=CARTESIAN_POINT('Ctrl Pts',(7.45762995869177,-1.18821533969688,13.6359094813931));
#9535=CARTESIAN_POINT('Ctrl Pts',(7.38624228015617,-1.35471305534666,13.6458690665646));
#9536=CARTESIAN_POINT('Ctrl Pts',(7.24888199481941,-1.61275477940762,13.6625025044014));
#9537=CARTESIAN_POINT('Ctrl Pts',(7.19142734031945,-1.70837519428772,13.6689657509572));
#9538=CARTESIAN_POINT('Ctrl Pts',(7.11990623727849,-1.814522909026,13.6767164889205));
#9539=CARTESIAN_POINT('Ctrl Pts',(7.11056557345264,-1.82815826858343,13.6777235505348));
#9540=CARTESIAN_POINT('Ctrl Pts',(7.09533277420137,-1.8500320755244,13.6793586503808));
#9541=CARTESIAN_POINT('Ctrl Pts',(7.08950582657601,-1.8583158400676,13.6799824564271));
#9542=CARTESIAN_POINT('Ctrl Pts',(7.07909719814258,-1.87296582292038,13.6810940907671));
#9543=CARTESIAN_POINT('Ctrl Pts',(7.07453120105153,-1.87934295650837,13.6815808517866));
#9544=CARTESIAN_POINT('Ctrl Pts',(7.06458744256367,-1.89312441388107,13.6826390744354));
#9545=CARTESIAN_POINT('Ctrl Pts',(7.05920149663022,-1.90052240235201,13.6832110776686));
#9546=CARTESIAN_POINT('Ctrl Pts',(7.04395270755118,-1.92128133477971,13.6848270253689));
#9547=CARTESIAN_POINT('Ctrl Pts',(7.03401815580536,-1.93458890313138,13.6858757181601));
#9548=CARTESIAN_POINT('Ctrl Pts',(6.97047713496943,-2.01834533800077,13.6925543542624));
#9549=CARTESIAN_POINT('Ctrl Pts',(6.91409443833061,-2.0866310235974,13.6983519820784));
#9550=CARTESIAN_POINT('Ctrl Pts',(6.66069352322214,-2.36899282757778,13.7235884407757));
#9551=CARTESIAN_POINT('Ctrl Pts',(6.43794545911826,-2.55822758520408,13.7436454060561));
#9552=CARTESIAN_POINT('Ctrl Pts',(6.1221650285876,-2.76018289956538,13.7680056350018));
#9553=CARTESIAN_POINT('Ctrl Pts',(6.04976318727673,-2.80260032591528,13.7733654656271));
#9554=CARTESIAN_POINT('Ctrl Pts',(5.95352273291203,-2.85404714757985,13.780206794908));
#9555=CARTESIAN_POINT('Ctrl Pts',(5.93112294350223,-2.86568504902897,13.7817799180098));
#9556=CARTESIAN_POINT('Ctrl Pts',(5.89480748850041,-2.88401431121457,13.7843001608354));
#9557=CARTESIAN_POINT('Ctrl Pts',(5.88097678090408,-2.8908707593447,13.7852530364967));
#9558=CARTESIAN_POINT('Ctrl Pts',(5.85446553563167,-2.9037770089866,13.7870665023599));
#9559=CARTESIAN_POINT('Ctrl Pts',(5.84179369279982,-2.90984376457854,13.7879276667447));
#9560=CARTESIAN_POINT('Ctrl Pts',(5.812617034622,-2.92357855136183,13.789897791958));
#9561=CARTESIAN_POINT('Ctrl Pts',(5.79608603267887,-2.93119007591118,13.7910047842005));
#9562=CARTESIAN_POINT('Ctrl Pts',(5.7442456253661,-2.95452927572253,13.7944481923671));
#9563=CARTESIAN_POINT('Ctrl Pts',(5.70871638456807,-2.96976237277451,13.7967677452789));
#9564=CARTESIAN_POINT('Ctrl Pts',(5.53002626094137,-3.04259820800698,13.8082469337431));
#9565=CARTESIAN_POINT('Ctrl Pts',(5.38312525025187,-3.09050887185996,13.8170794854008));
#9566=CARTESIAN_POINT('Ctrl Pts',(4.98413433007395,-3.1896117236503,13.8402389650523));
#9567=CARTESIAN_POINT('Ctrl Pts',(4.72845711729497,-3.22149686421932,13.8542000824417));
#9568=CARTESIAN_POINT('Ctrl Pts',(4.43528713460996,-3.2228866225644,13.8716218407371));
#9569=CARTESIAN_POINT('Ctrl Pts',(4.39882946673899,-3.22244073265954,13.8738144113679));
#9570=CARTESIAN_POINT('Ctrl Pts',(4.34947596861523,-3.22099936655052,13.8768272266492));
#9571=CARTESIAN_POINT('Ctrl Pts',(4.33656558512677,-3.2205446097503,13.8776194948264));
#9572=CARTESIAN_POINT('Ctrl Pts',(4.31615380471127,-3.21970271849754,13.8788791466167));
#9573=CARTESIAN_POINT('Ctrl Pts',(4.30865026646491,-3.21936695131815,13.8793437119217));
#9574=CARTESIAN_POINT('Ctrl Pts',(4.29315179479551,-3.2186191305319,13.8803065055505));
#9575=CARTESIAN_POINT('Ctrl Pts',(4.285157194394,-3.21820351671839,13.8808049409972));
#9576=CARTESIAN_POINT('Ctrl Pts',(4.26590199833611,-3.21713054983919,13.8820096480538));
#9577=CARTESIAN_POINT('Ctrl Pts',(4.25464319797041,-3.21644385792047,13.8827175255939));
#9578=CARTESIAN_POINT('Ctrl Pts',(4.21546791356717,-3.21384799981331,13.8851921332886));
#9579=CARTESIAN_POINT('Ctrl Pts',(4.1875737559046,-3.21163442938975,13.8869745266135));
#9580=CARTESIAN_POINT('Ctrl Pts',(4.11898393503,-3.20529162027661,13.8914018059873));
#9581=CARTESIAN_POINT('Ctrl Pts',(4.07833203372368,-3.20075032674342,13.894064420926));
#9582=CARTESIAN_POINT('Ctrl Pts',(3.90967964896791,-3.17865225502166,13.9052429966878));
#9583=CARTESIAN_POINT('Ctrl Pts',(3.78271202267294,-3.15418080149188,13.9139716859022));
#9584=CARTESIAN_POINT('Ctrl Pts',(3.41468177254106,-3.0600083179504,13.9396714385325));
#9585=CARTESIAN_POINT('Ctrl Pts',(3.17983557867515,-2.96971770234912,13.956509610083));
#9586=CARTESIAN_POINT('Ctrl Pts',(2.92223568691936,-2.8344064197869,13.9749596834051));
#9587=CARTESIAN_POINT('Ctrl Pts',(2.88701639955016,-2.81505779217045,13.9774843074672));
#9588=CARTESIAN_POINT('Ctrl Pts',(2.83631091692538,-2.78595391949007,13.9811236388135));
#9589=CARTESIAN_POINT('Ctrl Pts',(2.8205324800884,-2.77671805864701,13.982256793438));
#9590=CARTESIAN_POINT('Ctrl Pts',(2.79272218323632,-2.76012004511184,13.9842555100907));
#9591=CARTESIAN_POINT('Ctrl Pts',(2.78065857237513,-2.75281229869889,13.9851230161558));
#9592=CARTESIAN_POINT('Ctrl Pts',(2.75565150762454,-2.73743851693216,13.9869225177319));
#9593=CARTESIAN_POINT('Ctrl Pts',(2.74271653094874,-2.72935931327512,13.9878540024717));
#9594=CARTESIAN_POINT('Ctrl Pts',(2.70924498137342,-2.70812117474639,13.9902665023559));
#9595=CARTESIAN_POINT('Ctrl Pts',(2.6887993378901,-2.69482023141235,13.9917422327826));
#9596=CARTESIAN_POINT('Ctrl Pts',(2.59818717011898,-2.63439733689004,13.9982945228518));
#9597=CARTESIAN_POINT('Ctrl Pts',(2.52973610666055,-2.5847558562676,14.003275811716));
#9598=CARTESIAN_POINT('Ctrl Pts',(2.34182948526469,-2.43686604809397,14.0171407075722));
#9599=CARTESIAN_POINT('Ctrl Pts',(2.22737876835255,-2.3326332230422,14.0258092319487));
#9600=CARTESIAN_POINT('Ctrl Pts',(1.9755638832424,-2.06777304689273,14.0462465174096));
#9601=CARTESIAN_POINT('Ctrl Pts',(1.84564662558299,-1.90109383463384,14.0579403396425));
#9602=CARTESIAN_POINT('Ctrl Pts',(1.71926191110106,-1.70131419510654,14.0721308791342));
#9603=CARTESIAN_POINT('Ctrl Pts',(1.70583135091994,-1.67951334187961,14.0736818892604));
#9604=CARTESIAN_POINT('Ctrl Pts',(1.68746187484791,-1.64888409401837,14.0758677795365));
#9605=CARTESIAN_POINT('Ctrl Pts',(1.68230220318664,-1.64018833999965,14.0764891153684));
#9606=CARTESIAN_POINT('Ctrl Pts',(1.67346394745453,-1.62513194472003,14.0775664912129));
#9607=CARTESIAN_POINT('Ctrl Pts',(1.66976600188284,-1.61878267756716,14.078021293668));
#9608=CARTESIAN_POINT('Ctrl Pts',(1.66201448473906,-1.60536826899351,14.0789832951336));
#9609=CARTESIAN_POINT('Ctrl Pts',(1.65796594985724,-1.59830034405348,14.0794908214991));
#9610=CARTESIAN_POINT('Ctrl Pts',(1.64801652968044,-1.58077696921104,14.080750600314));
#9611=CARTESIAN_POINT('Ctrl Pts',(1.64214723363691,-1.57030382024321,14.081504823357));
#9612=CARTESIAN_POINT('Ctrl Pts',(1.62045746967877,-1.53108848997792,14.0843330285229));
#9613=CARTESIAN_POINT('Ctrl Pts',(1.60501827907145,-1.50213912565454,14.0864290521794));
#9614=CARTESIAN_POINT('Ctrl Pts',(1.49360584154234,-1.28532571022899,14.1021596815978));
#9615=CARTESIAN_POINT('Ctrl Pts',(1.41585033477799,-1.08869063139299,14.1165700249028));
#9616=CARTESIAN_POINT('Ctrl Pts',(1.30264064159823,-0.69271164662861,14.1443671150533));
#9617=CARTESIAN_POINT('Ctrl Pts',(1.26559002447791,-0.494770768667403,14.157706669747));
#9618=CARTESIAN_POINT('Ctrl Pts',(1.24339255104212,-0.252993440710904,14.1731184079337));
#9619=CARTESIAN_POINT('Ctrl Pts',(1.24037988709977,-0.211274771900807,14.1757482061316));
#9620=CARTESIAN_POINT('Ctrl Pts',(1.23720302558135,-0.150958562652312,14.1795094239339));
#9621=CARTESIAN_POINT('Ctrl Pts',(1.2363864109681,-0.132401074333798,14.1806610707089));
#9622=CARTESIAN_POINT('Ctrl Pts',(1.23523044362633,-0.0996958830725559,
14.1826811787533));
#9623=CARTESIAN_POINT('Ctrl Pts',(1.23482375146724,-0.0855512059513194,
14.1835517214522));
#9624=CARTESIAN_POINT('Ctrl Pts',(1.23417510248544,-0.0562823048112054,
14.1853467873184));
#9625=CARTESIAN_POINT('Ctrl Pts',(1.2339464350297,-0.0411581126778235,14.1862708739258));
#9626=CARTESIAN_POINT('Ctrl Pts',(1.23363186519905,-0.00221677478436835,
14.1886415319656));
#9627=CARTESIAN_POINT('Ctrl Pts',(1.23370348643724,0.0216009887060091,14.1900831643403));
#9628=CARTESIAN_POINT('Ctrl Pts',(1.23514912816945,0.124173905957879,14.1962581319088));
#9629=CARTESIAN_POINT('Ctrl Pts',(1.23914608551795,0.202868489030255,14.2009095787873));
#9630=CARTESIAN_POINT('Ctrl Pts',(1.25806380988224,0.418741700692692,14.2135087402557));
#9631=CARTESIAN_POINT('Ctrl Pts',(1.27891322663128,0.555233070420645,14.2212900489046));
#9632=CARTESIAN_POINT('Ctrl Pts',(1.35513367409847,0.9029902144834,14.2412310431853));
#9633=CARTESIAN_POINT('Ctrl Pts',(1.42331623848131,1.11069070407474,14.2532403999187));
#9634=CARTESIAN_POINT('Ctrl Pts',(1.5272913634106,1.34441942648955,14.2684247357883));
#9635=CARTESIAN_POINT('Ctrl Pts',(1.5432576493015,1.37867493237495,14.2706956182593));
#9636=CARTESIAN_POINT('Ctrl Pts',(1.56556566102557,1.42441796698323,14.2738001353051));
#9637=CARTESIAN_POINT('Ctrl Pts',(1.57138119976016,1.4361605176657,14.2746035790639));
#9638=CARTESIAN_POINT('Ctrl Pts',(1.58065897591155,1.4546101279565,14.2758767031226));
#9639=CARTESIAN_POINT('Ctrl Pts',(1.584073516023,1.4613411992434,14.2763434587789));
#9640=CARTESIAN_POINT('Ctrl Pts',(1.59114792633489,1.47516637024125,14.2773069599709));
#9641=CARTESIAN_POINT('Ctrl Pts',(1.59481051882663,1.4822588867892,14.2778038887315));
#9642=CARTESIAN_POINT('Ctrl Pts',(1.6036514997011,1.49922431882597,14.2789987788665));
#9643=CARTESIAN_POINT('Ctrl Pts',(1.6088548181716,1.50908406396157,14.2796982811521));
#9644=CARTESIAN_POINT('Ctrl Pts',(1.62691489610489,1.54288002658651,14.2821129069378));
#9645=CARTESIAN_POINT('Ctrl Pts',(1.64002274789877,1.56667980193364,14.2838427232106));
#9646=CARTESIAN_POINT('Ctrl Pts',(1.6728397651505,1.62452223360079,14.2881140279753));
#9647=CARTESIAN_POINT('Ctrl Pts',(1.69287397612027,1.65837464753388,14.2906717569573));
#9648=CARTESIAN_POINT('Ctrl Pts',(1.7769848521379,1.79474114538311,14.3011882588007));
#9649=CARTESIAN_POINT('Ctrl Pts',(1.84618332021367,1.89397367822122,14.309337550426));
#9650=CARTESIAN_POINT('Ctrl Pts',(2.08341938738767,2.19640280943998,14.3353319242764));
#9651=CARTESIAN_POINT('Ctrl Pts',(2.27089900362723,2.38304115681519,14.3530775343362));
#9652=CARTESIAN_POINT('Ctrl Pts',(2.50678977521358,2.56634032846529,14.3720047737299));
#9653=CARTESIAN_POINT('Ctrl Pts',(2.53488662616988,2.5874452852819,14.3742133498339));
#9654=CARTESIAN_POINT('Ctrl Pts',(2.5777100126057,2.61852970877647,14.3775123641553));
#9655=CARTESIAN_POINT('Ctrl Pts',(2.5921824736702,2.62885316052389,14.3786160207957));
#9656=CARTESIAN_POINT('Ctrl Pts',(2.61747801353977,2.64658294391563,14.3805258060782));
#9657=CARTESIAN_POINT('Ctrl Pts',(2.62826213955876,2.65404386043874,14.3813340100135));
#9658=CARTESIAN_POINT('Ctrl Pts',(2.65087756232357,2.66948692053903,14.3830165861445));
#9659=CARTESIAN_POINT('Ctrl Pts',(2.66271696903669,2.67745672663395,14.3838904788468));
#9660=CARTESIAN_POINT('Ctrl Pts',(2.6909622973422,2.69619888839839,14.3859591177908));
#9661=CARTESIAN_POINT('Ctrl Pts',(2.70741456777154,2.70690062356626,14.3871512024184));
#9662=CARTESIAN_POINT('Ctrl Pts',(2.76340019145648,2.74259413411238,14.3911655337118));
#9663=CARTESIAN_POINT('Ctrl Pts',(2.80338056406409,2.76687613409256,14.3939616750454));
#9664=CARTESIAN_POINT('Ctrl Pts',(3.04430364074229,2.90611328492733,14.4104269685823));
#9665=CARTESIAN_POINT('Ctrl Pts',(3.25662871095167,3.00001693761937,14.4233125400605));
#9666=CARTESIAN_POINT('Ctrl Pts',(3.64921270157713,3.12522841372324,14.4463650118354));
#9667=CARTESIAN_POINT('Ctrl Pts',(3.82551000751064,3.16553150731771,14.4564878544845));
#9668=CARTESIAN_POINT('Ctrl Pts',(4.0308060223305,3.19462816425958,14.4689188765829));
#9669=CARTESIAN_POINT('Ctrl Pts',(4.05742956440232,3.19806277399873,14.4705434350207));
#9670=CARTESIAN_POINT('Ctrl Pts',(4.09433116658667,3.20235537320779,14.472816209741));
#9671=CARTESIAN_POINT('Ctrl Pts',(4.10457592083184,3.20349730810074,14.4734494258226));
#9672=CARTESIAN_POINT('Ctrl Pts',(4.12218275386761,3.20537438325845,14.4745417997836));
#9673=CARTESIAN_POINT('Ctrl Pts',(4.12954228431856,3.20613336477755,14.4749996382791));
#9674=CARTESIAN_POINT('Ctrl Pts',(4.14495826731517,3.2076695700567,14.4759613758462));
#9675=CARTESIAN_POINT('Ctrl Pts',(4.15301508878348,3.20844179122328,14.4764655618908));
#9676=CARTESIAN_POINT('Ctrl Pts',(4.17277411163566,3.21026054256094,14.4777057335754));
#9677=CARTESIAN_POINT('Ctrl Pts',(4.18447922540539,3.21127343833726,14.4784435596951));
#9678=CARTESIAN_POINT('Ctrl Pts',(4.22711989960889,3.21472852366581,14.4811422412636));
#9679=CARTESIAN_POINT('Ctrl Pts',(4.25808367459332,3.21678777574895,14.4831226705108));
#9680=CARTESIAN_POINT('Ctrl Pts',(4.33600568986535,3.22084072156798,14.488150720113));
#9681=CARTESIAN_POINT('Ctrl Pts',(4.38298586218097,3.22225482416824,14.491222436927));
#9682=CARTESIAN_POINT('Ctrl Pts',(4.77014741194583,3.2254374548829,14.5167819394477));
#9683=CARTESIAN_POINT('Ctrl Pts',(5.10864669690037,3.17436463155494,14.5403858485047));
#9684=CARTESIAN_POINT('Ctrl Pts',(5.49079332467771,3.05286328757666,14.5661432515988));
#9685=CARTESIAN_POINT('Ctrl Pts',(5.54810227181103,3.03284333120434,14.5699910357038));
#9686=CARTESIAN_POINT('Ctrl Pts',(5.62572727920928,3.00324055275362,14.5751851623551));
#9687=CARTESIAN_POINT('Ctrl Pts',(5.6465564439084,2.99504768944647,14.5765771713108));
#9688=CARTESIAN_POINT('Ctrl Pts',(5.67965814263576,2.98162774304877,14.5787869829935));
#9689=CARTESIAN_POINT('Ctrl Pts',(5.69198621008855,2.97654042665313,14.5796094557429));
#9690=CARTESIAN_POINT('Ctrl Pts',(5.71730803757016,2.96590666364735,14.5812978638825));
#9691=CARTESIAN_POINT('Ctrl Pts',(5.73029763350956,2.96035099969067,14.5821634650598));
#9692=CARTESIAN_POINT('Ctrl Pts',(5.7594995317123,2.94763352243498,14.5841084590075));
#9693=CARTESIAN_POINT('Ctrl Pts',(5.77569021482703,2.94042298970787,14.5851861650754));
#9694=CARTESIAN_POINT('Ctrl Pts',(5.82715044061085,2.9169945383745,14.5886100426635));
#9695=CARTESIAN_POINT('Ctrl Pts',(5.86218761109995,2.90027242464741,14.5909389301721));
#9696=CARTESIAN_POINT('Ctrl Pts',(5.94348495925571,2.85965235148318,14.5963436891206));
#9697=CARTESIAN_POINT('Ctrl Pts',(5.98948563832835,2.83525809175234,14.5994025733774));
#9698=CARTESIAN_POINT('Ctrl Pts',(6.15408612860223,2.7427922610927,14.6103815486283));
#9699=CARTESIAN_POINT('Ctrl Pts',(6.26891874587849,2.66830344494869,14.6180989555965));
#9700=CARTESIAN_POINT('Ctrl Pts',(6.55074403205544,2.45887895294038,14.6377694321812));
#9701=CARTESIAN_POINT('Ctrl Pts',(6.70960348816129,2.31418194151873,14.6495754499166));
#9702=CARTESIAN_POINT('Ctrl Pts',(6.88103364429328,2.12352867794647,14.6647409153597));
#9703=CARTESIAN_POINT('Ctrl Pts',(6.90854439162075,2.09170114012658,14.6672622685669));
#9704=CARTESIAN_POINT('Ctrl Pts',(6.94415327203489,2.04883667509095,14.6706585851679));
#9705=CARTESIAN_POINT('Ctrl Pts',(6.95281663386567,2.03827212018418,14.6714957055672));
#9706=CARTESIAN_POINT('Ctrl Pts',(6.96676269838553,2.02104328456586,14.6728615701919));
#9707=CARTESIAN_POINT('Ctrl Pts',(6.97208676148357,2.014412491411,14.673387405667));
#9708=CARTESIAN_POINT('Ctrl Pts',(6.98239284779177,2.00147231888601,14.6744140713768));
#9709=CARTESIAN_POINT('Ctrl Pts',(6.9873775846459,1.99516527134056,14.6749147031086));
#9710=CARTESIAN_POINT('Ctrl Pts',(6.99941336172188,1.97981905774341,14.6761332759717));
#9711=CARTESIAN_POINT('Ctrl Pts',(7.00643983398527,1.97076083434401,14.6768529147233));
#9712=CARTESIAN_POINT('Ctrl Pts',(7.0311616626226,1.93853696858531,14.6794136829932));
#9713=CARTESIAN_POINT('Ctrl Pts',(7.04859028609062,1.91516970235062,14.6812719259126));
#9714=CARTESIAN_POINT('Ctrl Pts',(7.09105582808355,1.85659278422195,14.6859268063001));
#9715=CARTESIAN_POINT('Ctrl Pts',(7.11570576171344,1.82111065313819,14.688743466472));
#9716=CARTESIAN_POINT('Ctrl Pts',(7.26461568675241,1.59729145278992,14.7064420458323));
#9717=CARTESIAN_POINT('Ctrl Pts',(7.36952265379383,1.3968349644446,14.7219424101969));
#9718=CARTESIAN_POINT('Ctrl Pts',(7.48827060509728,1.09711361525992,14.7435037122974));
#9719=CARTESIAN_POINT('Ctrl Pts',(7.51984179616873,1.00559879559793,14.7498970662721));
#9720=CARTESIAN_POINT('Ctrl Pts',(7.56977246922604,0.836530558452999,14.7613300555828));
#9721=CARTESIAN_POINT('Ctrl Pts',(7.58946666073998,0.759453290113551,14.7664044723514));
#9722=CARTESIAN_POINT('Ctrl Pts',(7.6115247142054,0.657536273701604,14.7729387032276));
#9723=CARTESIAN_POINT('Ctrl Pts',(7.61648037024327,0.633291960173989,14.7744803292275));
#9724=CARTESIAN_POINT('Ctrl Pts',(7.62405286212141,0.593940782413684,14.7769624828522));
#9725=CARTESIAN_POINT('Ctrl Pts',(7.62684192522217,0.578868469647898,14.7779084559418));
#9726=CARTESIAN_POINT('Ctrl Pts',(7.63198637842811,0.549914396956638,14.7797167870231));
#9727=CARTESIAN_POINT('Ctrl Pts',(7.63435853079836,0.536036011064709,14.7805796581345));
#9728=CARTESIAN_POINT('Ctrl Pts',(7.63886555511494,0.508585439083418,14.782278835495));
#9729=CARTESIAN_POINT('Ctrl Pts',(7.64100473704754,0.495014274410429,14.7831152608139));
#9730=CARTESIAN_POINT('Ctrl Pts',(7.64573174625454,0.463726151964611,14.7850355122205));
#9731=CARTESIAN_POINT('Ctrl Pts',(7.64825885707549,0.446000377970389,14.7861174202155));
#9732=CARTESIAN_POINT('Ctrl Pts',(7.6572019822485,0.379297344009631,14.7901671597348));
#9733=CARTESIAN_POINT('Ctrl Pts',(7.66263964684926,0.330194287256672,14.7931046605912));
#9734=CARTESIAN_POINT('Ctrl Pts',(7.67512411768421,0.187548556376506,14.8015302425086));
#9735=CARTESIAN_POINT('Ctrl Pts',(7.67921910621824,0.0937987030144953,14.806932435509));
#9736=CARTESIAN_POINT('Ctrl Pts',(7.67921910621823,2.3786865083016E-11,
14.8122635502411));
#9737=CARTESIAN_POINT('Ctrl Pts',(7.67921910621823,-1.84544675223763E-11,
14.5621759541225));
#9738=CARTESIAN_POINT('Ctrl Pts',(7.67921910621823,0.000668280097381219,
14.5621374535563));
#9739=CARTESIAN_POINT('Ctrl Pts',(7.67921889835307,0.00133656291538531,
14.5620989575348));
#9740=CARTESIAN_POINT('Ctrl Pts',(7.67909503873809,0.200438155357122,14.5506312262009));
#9741=CARTESIAN_POINT('Ctrl Pts',(7.66064549735702,0.398434351142203,14.5396726513469));
#9742=CARTESIAN_POINT('Ctrl Pts',(7.59450626321197,0.751444354318352,14.5195032484083));
#9743=CARTESIAN_POINT('Ctrl Pts',(7.55313980900694,0.906952413113773,14.5103727338205));
#9744=CARTESIAN_POINT('Ctrl Pts',(7.49482381008865,1.07461718896952,14.499627873536));
#9745=CARTESIAN_POINT('Ctrl Pts',(7.48916459758958,1.09048587261971,14.4986016757321));
#9746=CARTESIAN_POINT('Ctrl Pts',(7.47990966549629,1.11580779055098,14.4969482174958));
#9747=CARTESIAN_POINT('Ctrl Pts',(7.4763933298234,1.12528997071433,14.4963254554595));
#9748=CARTESIAN_POINT('Ctrl Pts',(7.4700656187829,1.14211005158411,14.4952140904344));
#9749=CARTESIAN_POINT('Ctrl Pts',(7.46727196151491,1.1494544251454,14.4947265407459));
#9750=CARTESIAN_POINT('Ctrl Pts',(7.46120453016421,1.16523148696397,14.4936742033071));
#9751=CARTESIAN_POINT('Ctrl Pts',(7.45792216103014,1.17366048803549,14.4931089300761));
#9752=CARTESIAN_POINT('Ctrl Pts',(7.44869059052325,1.19707481208954,14.4915304087946));
#9753=CARTESIAN_POINT('Ctrl Pts',(7.44266444810608,1.21202923719652,14.4905127476183));
#9754=CARTESIAN_POINT('Ctrl Pts',(7.40643337908578,1.3000293753218,14.4844708098356));
#9755=CARTESIAN_POINT('Ctrl Pts',(7.37366389448707,1.37198321574115,14.4793127284117));
#9756=CARTESIAN_POINT('Ctrl Pts',(7.24302226894476,1.63295050469672,14.4599721949457));
#9757=CARTESIAN_POINT('Ctrl Pts',(7.12914480878979,1.81334320822728,14.4453784097787));
#9758=CARTESIAN_POINT('Ctrl Pts',(6.89801354792347,2.10988108581692,14.4202523384195));
#9759=CARTESIAN_POINT('Ctrl Pts',(6.78807410901351,2.23077781869281,14.4095932249652));
#9760=CARTESIAN_POINT('Ctrl Pts',(6.64970414225297,2.36147711178539,14.3976115866561));
#9761=CARTESIAN_POINT('Ctrl Pts',(6.62974004158838,2.37986293442126,14.3959138685314));
#9762=CARTESIAN_POINT('Ctrl Pts',(6.59657628207801,2.40963952479686,14.3931433638542));
#9763=CARTESIAN_POINT('Ctrl Pts',(6.58351253480578,2.42117897637548,14.3920643514368));
#9764=CARTESIAN_POINT('Ctrl Pts',(6.55981500428074,2.44177161036826,14.3901288409292));
#9765=CARTESIAN_POINT('Ctrl Pts',(6.5492148540294,2.45086266625679,14.3892707831063));
#9766=CARTESIAN_POINT('Ctrl Pts',(6.52643290943104,2.47014567776588,14.3874428564832));
#9767=CARTESIAN_POINT('Ctrl Pts',(6.5142341506277,2.48031708701237,14.3864738421072));
#9768=CARTESIAN_POINT('Ctrl Pts',(6.48087453751981,2.50771704520668,14.3838498863127));
#9769=CARTESIAN_POINT('Ctrl Pts',(6.45956897233869,2.52476793486275,14.3822021125532));
#9770=CARTESIAN_POINT('Ctrl Pts',(6.34128348057619,2.61699215112238,14.3732017676736));
#9771=CARTESIAN_POINT('Ctrl Pts',(6.2402822093321,2.68685482957355,14.3660604271901));
#9772=CARTESIAN_POINT('Ctrl Pts',(6.00739120865093,2.82900978486206,14.3504845664106));
#9773=CARTESIAN_POINT('Ctrl Pts',(5.87393719635609,2.89817905703745,14.342139651112));
#9774=CARTESIAN_POINT('Ctrl Pts',(5.58045190647431,3.02515431194848,14.3242352231939));
#9775=CARTESIAN_POINT('Ctrl Pts',(5.41969959233771,3.08010858363322,14.3146850043082));
#9776=CARTESIAN_POINT('Ctrl Pts',(5.2293016041149,3.12882930852328,14.3029033625162));
#9777=CARTESIAN_POINT('Ctrl Pts',(5.20312827659499,3.13517828639295,14.3012735630718));
#9778=CARTESIAN_POINT('Ctrl Pts',(5.16682087539358,3.14350511734529,14.298994752286));
#9779=CARTESIAN_POINT('Ctrl Pts',(5.15675145022703,3.14576361010987,14.2983608491235));
#9780=CARTESIAN_POINT('Ctrl Pts',(5.1394421296764,3.14955872910914,14.2972676368545));
#9781=CARTESIAN_POINT('Ctrl Pts',(5.13220739548798,3.1511188648941,14.2968096520904));
#9782=CARTESIAN_POINT('Ctrl Pts',(5.11705348761897,3.1543321455049,14.295848021324));
#9783=CARTESIAN_POINT('Ctrl Pts',(5.10913341072838,3.15598040387741,14.2953440909324));
#9784=CARTESIAN_POINT('Ctrl Pts',(5.08971250748114,3.15994588523639,14.2941052488143));
#9785=CARTESIAN_POINT('Ctrl Pts',(5.07820513617605,3.16223014689314,14.2933685048975));
#9786=CARTESIAN_POINT('Ctrl Pts',(5.03632261131575,3.17030655896598,14.2906778680443));
#9787=CARTESIAN_POINT('Ctrl Pts',(5.0058780464719,3.17572407766685,14.2887045480987));
#9788=CARTESIAN_POINT('Ctrl Pts',(4.92919639643872,3.18823374560923,14.2836983456709));
#9789=CARTESIAN_POINT('Ctrl Pts',(4.8828749841513,3.19475869056921,14.2806416142801));
#9790=CARTESIAN_POINT('Ctrl Pts',(4.50445092510337,3.2396881446224,14.2554882161959));
#9791=CARTESIAN_POINT('Ctrl Pts',(4.16833193024383,3.22721804051266,14.2322958511351));
#9792=CARTESIAN_POINT('Ctrl Pts',(3.7758054286254,3.15073045182821,14.2065419024282));
#9793=CARTESIAN_POINT('Ctrl Pts',(3.71192576680821,3.13624961335846,14.2023831248437));
#9794=CARTESIAN_POINT('Ctrl Pts',(3.62621624185979,3.11405345719717,14.1968440555202));
#9795=CARTESIAN_POINT('Ctrl Pts',(3.60396686911272,3.10803615376427,14.1954098886343));
#9796=CARTESIAN_POINT('Ctrl Pts',(3.56738673451449,3.09772075038639,14.1930576787443));
#9797=CARTESIAN_POINT('Ctrl Pts',(3.55301823141858,3.09356070570831,14.192135200289));
#9798=CARTESIAN_POINT('Ctrl Pts',(3.5250441141134,3.08524996810971,14.1903418859184));
#9799=CARTESIAN_POINT('Ctrl Pts',(3.51143600937368,3.08110894609963,14.1894707591095));
#9800=CARTESIAN_POINT('Ctrl Pts',(3.47937377395767,3.07111982952666,14.1874209863259));
#9801=CARTESIAN_POINT('Ctrl Pts',(3.46094390837154,3.0651952468612,14.1862448700069));
#9802=CARTESIAN_POINT('Ctrl Pts',(3.39968995235336,3.04489341262478,14.1823420712968));
#9803=CARTESIAN_POINT('Ctrl Pts',(3.35711372971005,3.02978153228021,14.1796395215578));
#9804=CARTESIAN_POINT('Ctrl Pts',(3.25608422394308,2.99151215891566,14.1732404660703));
#9805=CARTESIAN_POINT('Ctrl Pts',(3.19796254262301,2.96752940763584,14.1695706095977));
#9806=CARTESIAN_POINT('Ctrl Pts',(2.82507814161248,2.80073848069028,14.145996914924));
#9807=CARTESIAN_POINT('Ctrl Pts',(2.53439989466032,2.60981708533835,14.1277329016664));
#9808=CARTESIAN_POINT('Ctrl Pts',(2.25642222333436,2.35518600960463,14.1052314380284));
#9809=CARTESIAN_POINT('Ctrl Pts',(2.23353566643227,2.33359683354842,14.1033333515255));
#9810=CARTESIAN_POINT('Ctrl Pts',(2.20223543237642,2.30319264931507,14.1006673415672));
#9811=CARTESIAN_POINT('Ctrl Pts',(2.19354936152978,2.29465902788125,14.0999198183001));
#9812=CARTESIAN_POINT('Ctrl Pts',(2.17968624278577,2.28088395737702,14.0987139416052));
#9813=CARTESIAN_POINT('Ctrl Pts',(2.17447834595029,2.27567352705129,14.0982579956657));
#9814=CARTESIAN_POINT('Ctrl Pts',(2.16356562943253,2.26468037345803,14.0972962760922));
#9815=CARTESIAN_POINT('Ctrl Pts',(2.15786476281457,2.25889389202919,14.096790191477));
#9816=CARTESIAN_POINT('Ctrl Pts',(2.14386711522806,2.24457817417296,14.0955386179663));
#9817=CARTESIAN_POINT('Ctrl Pts',(2.13559563195884,2.23602447544034,14.0947912124938));
#9818=CARTESIAN_POINT('Ctrl Pts',(2.10520951288517,2.20425136708127,14.0920171389705));
#9819=CARTESIAN_POINT('Ctrl Pts',(2.08339522677425,2.18074894135581,14.0899694777593));
#9820=CARTESIAN_POINT('Ctrl Pts',(1.92835283495276,2.00862708802443,14.0750291528445));
#9821=CARTESIAN_POINT('Ctrl Pts',(1.80884515799611,1.84825070333104,14.0614328501973));
#9822=CARTESIAN_POINT('Ctrl Pts',(1.59383510024042,1.49565709925879,14.0335264710804));
#9823=CARTESIAN_POINT('Ctrl Pts',(1.5010814572475,1.30283377865261,14.0193147045042));
#9824=CARTESIAN_POINT('Ctrl Pts',(1.41521590396304,1.06691542992767,14.0033794686006));
#9825=CARTESIAN_POINT('Ctrl Pts',(1.40298226732136,1.03138154481074,14.0010144689211));
#9826=CARTESIAN_POINT('Ctrl Pts',(1.38506717777146,0.976229633878805,13.9973964776238));
#9827=CARTESIAN_POINT('Ctrl Pts',(1.37894630676164,0.956758879604003,13.9961291927427));
#9828=CARTESIAN_POINT('Ctrl Pts',(1.36886027581244,0.92357617507163,13.9939860482907));
#9829=CARTESIAN_POINT('Ctrl Pts',(1.36480054965817,0.909893833129339,13.993107120556));
#9830=CARTESIAN_POINT('Ctrl Pts',(1.35676299688425,0.88213019738672,13.9913330896865));
#9831=CARTESIAN_POINT('Ctrl Pts',(1.35278991035701,0.868047872911373,13.9904381585538));
#9832=CARTESIAN_POINT('Ctrl Pts',(1.34321670461973,0.833210158616637,13.9882360259451));
#9833=CARTESIAN_POINT('Ctrl Pts',(1.33772803572621,0.812424675982848,13.9869324522086));
#9834=CARTESIAN_POINT('Ctrl Pts',(1.317891595552,0.734139424707712,13.982059855971));
#9835=CARTESIAN_POINT('Ctrl Pts',(1.30492219573072,0.676300391067899,13.9785350100107));
#9836=CARTESIAN_POINT('Ctrl Pts',(1.27615686629611,0.529111721636741,13.9697263455005));
#9837=CARTESIAN_POINT('Ctrl Pts',(1.26252443902447,0.439390921102984,13.9645063327866));
#9838=CARTESIAN_POINT('Ctrl Pts',(1.23760916997616,0.210809062254648,13.9514419591284));
#9839=CARTESIAN_POINT('Ctrl Pts',(1.23150739452777,0.0715740310489558,13.9437050295382));
#9840=CARTESIAN_POINT('Ctrl Pts',(1.23788548569985,-0.23234013637818,13.92667648119));
#9841=CARTESIAN_POINT('Ctrl Pts',(1.25396853637502,-0.396534319980223,13.9173846255518));
#9842=CARTESIAN_POINT('Ctrl Pts',(1.28721481952918,-0.585385226616336,13.9058905525115));
#9843=CARTESIAN_POINT('Ctrl Pts',(1.29223732115812,-0.611952366562802,13.904254493684));
#9844=CARTESIAN_POINT('Ctrl Pts',(1.29964051032992,-0.648581195326102,13.9019684414169));
#9845=CARTESIAN_POINT('Ctrl Pts',(1.30173639977978,-0.6587001555527,13.9013336853142));
#9846=CARTESIAN_POINT('Ctrl Pts',(1.30541759048237,-0.676052319841705,13.9002393919425));
#9847=CARTESIAN_POINT('Ctrl Pts',(1.30697923714229,-0.683290535545815,13.8997811849379));
#9848=CARTESIAN_POINT('Ctrl Pts',(1.31029845498599,-0.698421926569698,13.8988195495288));
#9849=CARTESIAN_POINT('Ctrl Pts',(1.31206080017165,-0.70631392026081,13.8983158395494));
#9850=CARTESIAN_POINT('Ctrl Pts',(1.31644891143079,-0.725622472868669,13.8970783148354));
#9851=CARTESIAN_POINT('Ctrl Pts',(1.31910724697604,-0.737031445070224,13.8963426766312));
#9852=CARTESIAN_POINT('Ctrl Pts',(1.32898178079829,-0.778389101116496,13.8936605726701));
#9853=CARTESIAN_POINT('Ctrl Pts',(1.3365648444778,-0.808247362285659,13.8916948365096));
#9854=CARTESIAN_POINT('Ctrl Pts',(1.35667509513097,-0.882927138720909,13.8867120039979));
#9855=CARTESIAN_POINT('Ctrl Pts',(1.36974709336806,-0.927593672279187,13.8836713238479));
#9856=CARTESIAN_POINT('Ctrl Pts',(1.48281013137566,-1.28502378130988,13.8589309884121));
#9857=CARTESIAN_POINT('Ctrl Pts',(1.62910408500653,-1.58114236493716,13.8361569272549));
#9858=CARTESIAN_POINT('Ctrl Pts',(1.85811725982171,-1.90778690595023,13.8103996454192));
#9859=CARTESIAN_POINT('Ctrl Pts',(1.90045430153217,-1.96414682636604,13.805916464426));
#9860=CARTESIAN_POINT('Ctrl Pts',(1.95945165665872,-2.03754331424302,13.8000214080405));
#9861=CARTESIAN_POINT('Ctrl Pts',(1.97449872822753,-2.0558458093323,13.7985464028389));
#9862=CARTESIAN_POINT('Ctrl Pts',(1.99946250488216,-2.0855368752841,13.7961448658852));
#9863=CARTESIAN_POINT('Ctrl Pts',(2.00925962390741,-2.09702438212829,13.7952135234316));
#9864=CARTESIAN_POINT('Ctrl Pts',(2.02840087277306,-2.11915141176225,13.7934151387024));
#9865=CARTESIAN_POINT('Ctrl Pts',(2.03773509197325,-2.12979901180117,13.7925477180528));
#9866=CARTESIAN_POINT('Ctrl Pts',(2.05973658409488,-2.15456504856732,13.7905251193534));
#9867=CARTESIAN_POINT('Ctrl Pts',(2.07245901084021,-2.16863395252972,13.7893722800737));
#9868=CARTESIAN_POINT('Ctrl Pts',(2.11436088600907,-2.21415611636309,13.7856285533746));
#9869=CARTESIAN_POINT('Ctrl Pts',(2.14404505419226,-2.24513997052017,13.7830591256843));
#9870=CARTESIAN_POINT('Ctrl Pts',(2.21582687870698,-2.31713018133583,13.7770286625279));
#9871=CARTESIAN_POINT('Ctrl Pts',(2.2584452823529,-2.35759659762561,13.773590214167));
#9872=CARTESIAN_POINT('Ctrl Pts',(2.51085191031132,-2.5844605145735,13.7539501353106));
#9873=CARTESIAN_POINT('Ctrl Pts',(2.74314070948067,-2.74396680762048,13.7387821065838));
#9874=CARTESIAN_POINT('Ctrl Pts',(3.07613032813164,-2.91366764626532,13.7173533130667));
#9875=CARTESIAN_POINT('Ctrl Pts',(3.16091017783334,-2.95234110590285,13.711909767744));
#9876=CARTESIAN_POINT('Ctrl Pts',(3.26197101875949,-2.99324983167174,13.7053017956754));
#9877=CARTESIAN_POINT('Ctrl Pts',(3.27674891231762,-2.9991049458972,13.7043326047753));
#9878=CARTESIAN_POINT('Ctrl Pts',(3.30083567030626,-3.00844273627513,13.7027472291953));
#9879=CARTESIAN_POINT('Ctrl Pts',(3.31011859319263,-3.01199216977737,13.7021348720278));
#9880=CARTESIAN_POINT('Ctrl Pts',(3.32674254625061,-3.01826054956571,13.7010355757096));
#9881=CARTESIAN_POINT('Ctrl Pts',(3.3340772395925,-3.02099575320679,13.7005496115846));
#9882=CARTESIAN_POINT('Ctrl Pts',(3.35013702053118,-3.0269180960205,13.6994834551387));
#9883=CARTESIAN_POINT('Ctrl Pts',(3.35886582151306,-3.03009420120151,13.6989026480833));
#9884=CARTESIAN_POINT('Ctrl Pts',(3.38384726229506,-3.03906196641303,13.6972368580765));
#9885=CARTESIAN_POINT('Ctrl Pts',(3.40013256191121,-3.04476080018153,13.6961466617832));
#9886=CARTESIAN_POINT('Ctrl Pts',(3.51519340614459,-3.08399068982933,13.6884179401053));
#9887=CARTESIAN_POINT('Ctrl Pts',(3.61549084426952,-3.11283626087745,13.6815473107918));
#9888=CARTESIAN_POINT('Ctrl Pts',(3.92819197838124,-3.1865533499662,13.6600649581354));
#9889=CARTESIAN_POINT('Ctrl Pts',(4.14389397697756,-3.2148882277126,13.6452036680957));
#9890=CARTESIAN_POINT('Ctrl Pts',(4.4022998077223,-3.22256211297559,13.6280718044847));
#9891=CARTESIAN_POINT('Ctrl Pts',(4.44381554531811,-3.2229925501364,13.6253380233406));
#9892=CARTESIAN_POINT('Ctrl Pts',(4.5820523133432,-3.22175457106555,13.6163022463906));
#9893=CARTESIAN_POINT('Ctrl Pts',(4.67869446175065,-3.2165342668205,13.6100964425014));
#9894=CARTESIAN_POINT('Ctrl Pts',(4.80134393976071,-3.20435355041761,13.6023609886958));
#9895=CARTESIAN_POINT('Ctrl Pts',(4.82769114735343,-3.201408219916,13.6007074247587));
#9896=CARTESIAN_POINT('Ctrl Pts',(4.86959270277683,-3.19619983044423,13.5980900288976));
#9897=CARTESIAN_POINT('Ctrl Pts',(4.88517157619495,-3.19414756521506,13.5971196175894));
#9898=CARTESIAN_POINT('Ctrl Pts',(4.91320464959167,-3.19024586970708,13.5953781578395));
#9899=CARTESIAN_POINT('Ctrl Pts',(4.92566411906265,-3.1884372524484,13.5946058412056));
#9900=CARTESIAN_POINT('Ctrl Pts',(4.95493424703653,-3.18401311100888,13.5927953098236));
#9901=CARTESIAN_POINT('Ctrl Pts',(4.97173553092693,-3.18133737861027,13.5917590175383));
#9902=CARTESIAN_POINT('Ctrl Pts',(5.02068476036917,-3.17314388920715,13.5887479980086));
#9903=CARTESIAN_POINT('Ctrl Pts',(5.05277166652581,-3.16727087881588,13.5867845198453));
#9904=CARTESIAN_POINT('Ctrl Pts',(5.29897716113582,-3.11833251213573,13.5717860605839));
#9905=CARTESIAN_POINT('Ctrl Pts',(5.50831444020005,-3.05408824374727,13.5594805031201));
#9906=CARTESIAN_POINT('Ctrl Pts',(5.91001419956551,-2.88455552524536,13.5350919147166));
#9907=CARTESIAN_POINT('Ctrl Pts',(6.10135336698419,-2.77988908263454,13.5230537413206));
#9908=CARTESIAN_POINT('Ctrl Pts',(6.30137955911803,-2.64254696934178,13.5084815170903));
#9909=CARTESIAN_POINT('Ctrl Pts',(6.32192818433605,-2.62808131610801,13.5069588001555));
#9910=CARTESIAN_POINT('Ctrl Pts',(6.35043871295164,-2.60750787196009,13.5048066233857));
#9911=CARTESIAN_POINT('Ctrl Pts',(6.35854503259861,-2.60160053383523,13.504190169292));
#9912=CARTESIAN_POINT('Ctrl Pts',(6.37252461160565,-2.59131289971176,13.5031189575797));
#9913=CARTESIAN_POINT('Ctrl Pts',(6.37841080942031,-2.58695019876686,13.5026654043984));
#9914=CARTESIAN_POINT('Ctrl Pts',(6.39069585492202,-2.57777976310625,13.5017134087303));
#9915=CARTESIAN_POINT('Ctrl Pts',(6.39709173639391,-2.57296821308916,13.5012146920526));
#9916=CARTESIAN_POINT('Ctrl Pts',(6.41247952024194,-2.5613021420518,13.5000075039506));
#9917=CARTESIAN_POINT('Ctrl Pts',(6.42145334776341,-2.55442406897991,13.4992974168503));
#9918=CARTESIAN_POINT('Ctrl Pts',(6.44095531016407,-2.53931303540811,13.4977412734762));
#9919=CARTESIAN_POINT('Ctrl Pts',(6.45146875418697,-2.5310615512356,13.4968940165852));
#9920=CARTESIAN_POINT('Ctrl Pts',(6.48101781920159,-2.50757146273953,13.4944897567835));
#9921=CARTESIAN_POINT('Ctrl Pts',(6.49993185008024,-2.49218219043527,13.4929236241527));
#9922=CARTESIAN_POINT('Ctrl Pts',(6.56305320578506,-2.43962227858665,13.487609685616));
#9923=CARTESIAN_POINT('Ctrl Pts',(6.60643361362268,-2.40147981221747,13.4838109813724));
#9924=CARTESIAN_POINT('Ctrl Pts',(6.84336442457945,-2.18159023073843,13.4623293720801));
#9925=CARTESIAN_POINT('Ctrl Pts',(7.01491172105647,-1.97762541223175,13.4440443299091));
#9926=CARTESIAN_POINT('Ctrl Pts',(7.21824865472653,-1.66442997305387,13.4195268783202));
#9927=CARTESIAN_POINT('Ctrl Pts',(7.27241290310834,-1.57105641319643,13.4125838106318));
#9928=CARTESIAN_POINT('Ctrl Pts',(7.33417509311794,-1.45108826908946,13.4041091031588));
#9929=CARTESIAN_POINT('Ctrl Pts',(7.3462507122496,-1.42688866167521,13.4024212026745));
#9930=CARTESIAN_POINT('Ctrl Pts',(7.36497677984122,-1.38814846469177,13.3997525998214));
#9931=CARTESIAN_POINT('Ctrl Pts',(7.37182590555821,-1.37370586182128,13.3987650311547));
#9932=CARTESIAN_POINT('Ctrl Pts',(7.38445212800718,-1.34656142494925,13.3969223483472));
#9933=CARTESIAN_POINT('Ctrl Pts',(7.39025470693223,-1.33387192255277,13.3960663710962));
#9934=CARTESIAN_POINT('Ctrl Pts',(7.40306065038044,-1.30537910464537,13.3941563237535));
#9935=CARTESIAN_POINT('Ctrl Pts',(7.41001968722926,-1.28955624867551,13.3931037898284));
#9936=CARTESIAN_POINT('Ctrl Pts',(7.43027196280166,-1.24248432210975,13.3899961361588));
#9937=CARTESIAN_POINT('Ctrl Pts',(7.44319922745701,-1.21107969815745,13.3879534210041));
#9938=CARTESIAN_POINT('Ctrl Pts',(7.52870715791737,-0.99365098824755,13.3740077225398));
#9939=CARTESIAN_POINT('Ctrl Pts',(7.58436220790903,-0.801428459235842,13.3626990609833));
#9940=CARTESIAN_POINT('Ctrl Pts',(7.66002300390259,-0.40574215963851,13.3401367438679));
#9941=CARTESIAN_POINT('Ctrl Pts',(7.67921910621675,-0.203083804950041,13.3289292504702));
#9942=CARTESIAN_POINT('Ctrl Pts',(7.67921910621823,-2.34794475528766E-11,
13.3169799747702));
#9943=CARTESIAN_POINT('Origin',(4.45646910621825,-5.13094777615093E-16,
-2.31077344927308));
#9944=CARTESIAN_POINT('',(7.67921910621823,-1.80065651569973E-10,12.0641237905203));
#9945=CARTESIAN_POINT('',(7.67921910621823,3.33464896044866E-11,12.3083142504469));
#9946=CARTESIAN_POINT('',(7.67921910621823,-3.51191647465084E-13,-2.31077344927308));
#9947=CARTESIAN_POINT('Ctrl Pts',(7.67921910621823,3.33546384956307E-11,
12.3083142504469));
#9948=CARTESIAN_POINT('Ctrl Pts',(7.67921910622113,-0.280383095796685,12.3267276928725));
#9949=CARTESIAN_POINT('Ctrl Pts',(7.64263159215061,-0.559592506371846,12.3461293237484));
#9950=CARTESIAN_POINT('Ctrl Pts',(7.53881732225561,-0.948797846265927,12.3727036979257));
#9951=CARTESIAN_POINT('Ctrl Pts',(7.50057450373251,-1.06513681324748,12.3806045998136));
#9952=CARTESIAN_POINT('Ctrl Pts',(7.44582673239986,-1.20440944008838,12.3900026642943));
#9953=CARTESIAN_POINT('Ctrl Pts',(7.43552883995388,-1.22966023471888,12.3917043587878));
#9954=CARTESIAN_POINT('Ctrl Pts',(7.41872874207879,-1.26940441635969,12.3943799193372));
#9955=CARTESIAN_POINT('Ctrl Pts',(7.41243793317796,-1.28398521447319,12.3953608775295));
#9956=CARTESIAN_POINT('Ctrl Pts',(7.4004121269501,-1.31130168704837,12.3971977069326));
#9957=CARTESIAN_POINT('Ctrl Pts',(7.39470163099574,-1.32404768185387,12.3980543874791));
#9958=CARTESIAN_POINT('Ctrl Pts',(7.38167499036028,-1.35262419376029,12.3999743765636));
#9959=CARTESIAN_POINT('Ctrl Pts',(7.3743128118175,-1.36843333869575,12.4010360767259));
#9960=CARTESIAN_POINT('Ctrl Pts',(7.35515518848157,-1.40871376966487,12.4037404772194));
#9961=CARTESIAN_POINT('Ctrl Pts',(7.34317785921788,-1.43309739084182,12.4053768769742));
#9962=CARTESIAN_POINT('Ctrl Pts',(7.25672026003652,-1.60362588695045,12.4168224247787));
#9963=CARTESIAN_POINT('Ctrl Pts',(7.17148211227494,-1.74405754107698,12.4262373645221));
#9964=CARTESIAN_POINT('Ctrl Pts',(7.01756403963998,-1.9588113864248,12.4411339624225));
#9965=CARTESIAN_POINT('Ctrl Pts',(6.95545297765951,-2.03745656534628,12.4467152953346));
#9966=CARTESIAN_POINT('Ctrl Pts',(6.80388689882243,-2.21199189525644,12.4596539543624));
#9967=CARTESIAN_POINT('Ctrl Pts',(6.71204870215988,-2.30556590073623,12.467015678508));
#9968=CARTESIAN_POINT('Ctrl Pts',(6.58415928554667,-2.42089905136426,12.4770672170594));
#9969=CARTESIAN_POINT('Ctrl Pts',(6.55301305340035,-2.44792174795321,12.4795012765369));
#9970=CARTESIAN_POINT('Ctrl Pts',(6.50653588881959,-2.48670795793105,12.4831279841435));
#9971=CARTESIAN_POINT('Ctrl Pts',(6.49160286495506,-2.49894394229083,12.4842924397806));
#9972=CARTESIAN_POINT('Ctrl Pts',(6.46471989572811,-2.52057082669988,12.4863891634543));
#9973=CARTESIAN_POINT('Ctrl Pts',(6.45281162415638,-2.53001285693807,12.4873180908032));
#9974=CARTESIAN_POINT('Ctrl Pts',(6.4338005774955,-2.5448688702918,12.4888021183337));
#9975=CARTESIAN_POINT('Ctrl Pts',(6.4267411422943,-2.55033829395978,12.4893534110466));
#9976=CARTESIAN_POINT('Ctrl Pts',(6.41365960180178,-2.56038672068573,12.4903755895942));
#9977=CARTESIAN_POINT('Ctrl Pts',(6.40764402390254,-2.56497392424168,12.4908458898465));
#9978=CARTESIAN_POINT('Ctrl Pts',(6.39361876202776,-2.57559105601253,12.4919429370439));
#9979=CARTESIAN_POINT('Ctrl Pts',(6.3855970887134,-2.58160479113828,12.4925707823596));
#9980=CARTESIAN_POINT('Ctrl Pts',(6.36455276852032,-2.59722856976623,12.4942186348895));
#9981=CARTESIAN_POINT('Ctrl Pts',(6.35148574021324,-2.60677798014992,12.4952425715615));
#9982=CARTESIAN_POINT('Ctrl Pts',(6.25654681305502,-2.67506847618704,12.5026840260521));
#9983=CARTESIAN_POINT('Ctrl Pts',(6.17203916718867,-2.73003413698777,12.5093171424033));
#9984=CARTESIAN_POINT('Ctrl Pts',(5.9053557404573,-2.8862149346065,12.5299684545301));
#9985=CARTESIAN_POINT('Ctrl Pts',(5.71582050451688,-2.97381082121707,12.5442290818051));
#9986=CARTESIAN_POINT('Ctrl Pts',(5.42789978566637,-3.07437503110044,12.5645038317668));
#9987=CARTESIAN_POINT('Ctrl Pts',(5.33525869693962,-3.10212685741149,12.5708380402753));
#9988=CARTESIAN_POINT('Ctrl Pts',(5.20114628508984,-3.13581007976809,12.5797207759354));
#9989=CARTESIAN_POINT('Ctrl Pts',(5.16059571678796,-3.14516373637219,12.582370196098));
#9990=CARTESIAN_POINT('Ctrl Pts',(5.08778282902986,-3.16048033496879,12.5870635923237));
#9991=CARTESIAN_POINT('Ctrl Pts',(5.05558975562851,-3.16674083869105,12.5891166147838));
#9992=CARTESIAN_POINT('Ctrl Pts',(5.00652182547518,-3.17550787457755,12.592213300854));
#9993=CARTESIAN_POINT('Ctrl Pts',(4.98971411624229,-3.1783734885362,12.593268284443));
#9994=CARTESIAN_POINT('Ctrl Pts',(4.95912468727175,-3.18333932259374,12.5951781101941));
#9995=CARTESIAN_POINT('Ctrl Pts',(4.94535066443466,-3.18548374782396,12.5960343319193));
#9996=CARTESIAN_POINT('Ctrl Pts',(4.91557345614374,-3.18992195878262,12.5978774412759));
#9997=CARTESIAN_POINT('Ctrl Pts',(4.89956599667714,-3.192184842359,12.5988633320907));
#9998=CARTESIAN_POINT('Ctrl Pts',(4.8559488113597,-3.19801634126479,12.601536735067));
#9999=CARTESIAN_POINT('Ctrl Pts',(4.82830839654391,-3.20134786762485,12.603216773561));
#10000=CARTESIAN_POINT('Ctrl Pts',(4.68162062536532,-3.21710279522244,12.6120630033188));
#10001=CARTESIAN_POINT('Ctrl Pts',(4.56198647919039,-3.22324591996066,12.6190299901467));
#10002=CARTESIAN_POINT('Ctrl Pts',(4.21408862251111,-3.22171386894985,12.6388991770143));
#10003=CARTESIAN_POINT('Ctrl Pts',(3.98666505872358,-3.19647719283489,12.651364339304));
#10004=CARTESIAN_POINT('Ctrl Pts',(3.69213172208375,-3.13165995818053,12.6685534509104));
#10005=CARTESIAN_POINT('Ctrl Pts',(3.62100730242283,-3.113439889655,12.6727926536621));
#10006=CARTESIAN_POINT('Ctrl Pts',(3.52305722303507,-3.08474987867242,12.6788307043833));
#10007=CARTESIAN_POINT('Ctrl Pts',(3.49565248640691,-3.07632424576494,12.6805422377958));
#10008=CARTESIAN_POINT('Ctrl Pts',(3.44806417995651,-3.06099525360632,12.6835590326797));
#10009=CARTESIAN_POINT('Ctrl Pts',(3.42782960132389,-3.05425492575899,12.68485602953));
#10010=CARTESIAN_POINT('Ctrl Pts',(3.39810118291132,-3.04402319012996,12.68678469638));
#10011=CARTESIAN_POINT('Ctrl Pts',(3.38855402880637,-3.04068696582291,12.6874076204511));
#10012=CARTESIAN_POINT('Ctrl Pts',(3.37163195638336,-3.03468407264001,12.6885182973413));
#10013=CARTESIAN_POINT('Ctrl Pts',(3.36425086854456,-3.03203535300356,12.6890049900022));
#10014=CARTESIAN_POINT('Ctrl Pts',(3.34826797920018,-3.02623392208214,12.6900637887849));
#10015=CARTESIAN_POINT('Ctrl Pts',(3.33967006666442,-3.02307151576813,12.6906364419256));
#10016=CARTESIAN_POINT('Ctrl Pts',(3.31590097740323,-3.01421374644525,12.692227855125));
#10017=CARTESIAN_POINT('Ctrl Pts',(3.3007593369409,-3.00844063751657,12.6932510318437));
#10018=CARTESIAN_POINT('Ctrl Pts',(3.21902205422988,-2.97656824496834,12.6988228599169));
#10019=CARTESIAN_POINT('Ctrl Pts',(3.15327069599096,-2.94837344077278,12.703479833281));
#10020=CARTESIAN_POINT('Ctrl Pts',(3.06343515286575,-2.906258994978,12.7100368782526));
#10021=CARTESIAN_POINT('Ctrl Pts',(3.03850610157407,-2.89417791309808,12.7118778132383));
#10022=CARTESIAN_POINT('Ctrl Pts',(2.76593378100132,-2.7577173343064,12.7322214904861));
#10023=CARTESIAN_POINT('Ctrl Pts',(2.53511957275793,-2.602185422782,12.7512800949521));
#10024=CARTESIAN_POINT('Ctrl Pts',(2.28317822030604,-2.3804078249608,12.7731215823635));
#10025=CARTESIAN_POINT('Ctrl Pts',(2.24035733189057,-2.34059479120643,12.7768823059954));
#10026=CARTESIAN_POINT('Ctrl Pts',(2.16814624449462,-2.26969654170508,12.7833098209696));
#10027=CARTESIAN_POINT('Ctrl Pts',(2.13824899115032,-2.2391515559859,12.7859981838682));
#10028=CARTESIAN_POINT('Ctrl Pts',(2.09599081180354,-2.19422389211145,12.7898398023908));
#10029=CARTESIAN_POINT('Ctrl Pts',(2.0831363424598,-2.18031371232119,12.7910141961165));
#10030=CARTESIAN_POINT('Ctrl Pts',(2.06088939508232,-2.15580978024384,12.7930572502876));
#10031=CARTESIAN_POINT('Ctrl Pts',(2.05144281222413,-2.14526606656641,12.7939281880721));
#10032=CARTESIAN_POINT('Ctrl Pts',(2.03205694964629,-2.12333972603486,12.7957227642804));
#10033=CARTESIAN_POINT('Ctrl Pts',(2.02212762386339,-2.11194873436338,12.7966459751391));
#10034=CARTESIAN_POINT('Ctrl Pts',(1.99680008638921,-2.08247685910075,12.799011665166));
#10035=CARTESIAN_POINT('Ctrl Pts',(1.98152078101579,-2.06429464697946,12.8004492457636));
#10036=CARTESIAN_POINT('Ctrl Pts',(1.92141222366032,-1.9911392796657,12.8061490001547));
#10037=CARTESIAN_POINT('Ctrl Pts',(1.87820039708457,-1.93485932107359,12.8103464884415));
#10038=CARTESIAN_POINT('Ctrl Pts',(1.80439232553842,-1.83186158480249,12.8177375603417));
#10039=CARTESIAN_POINT('Ctrl Pts',(1.77308719436076,-1.78569035762233,12.8209527577885));
#10040=CARTESIAN_POINT('Ctrl Pts',(1.61945999993934,-1.54593845630854,12.8372226771492));
#10041=CARTESIAN_POINT('Ctrl Pts',(1.51682907237625,-1.34054343587287,12.8497296651616));
#10042=CARTESIAN_POINT('Ctrl Pts',(1.3987369121024,-1.02385495744705,12.8689894033766));
#10043=CARTESIAN_POINT('Ctrl Pts',(1.36585505957918,-0.91983957267185,12.8753217721624));
#10044=CARTESIAN_POINT('Ctrl Pts',(1.33390847275518,-0.79751865796829,12.8829863052737));
#10045=CARTESIAN_POINT('Ctrl Pts',(1.32964405612803,-0.780631792002036,
12.8840491732649));
#10046=CARTESIAN_POINT('Ctrl Pts',(1.32330726809734,-0.754653163071605,
12.8856927250864));
#10047=CARTESIAN_POINT('Ctrl Pts',(1.32113705499851,-0.745585289473953,
12.8862679820854));
#10048=CARTESIAN_POINT('Ctrl Pts',(1.31721758402831,-0.728888674859578,
12.8873303038784));
#10049=CARTESIAN_POINT('Ctrl Pts',(1.31545673762614,-0.721262862141284,
12.8878167013743));
#10050=CARTESIAN_POINT('Ctrl Pts',(1.31153222360232,-0.703979765194318,
12.888921784122));
#10051=CARTESIAN_POINT('Ctrl Pts',(1.3093852645857,-0.694318941891138,12.8895413929244));
#10052=CARTESIAN_POINT('Ctrl Pts',(1.30393587446378,-0.669253315526627,
12.8911536405293));
#10053=CARTESIAN_POINT('Ctrl Pts',(1.30070189317633,-0.653834116257114,
12.8921499447888));
#10054=CARTESIAN_POINT('Ctrl Pts',(1.2798059829733,-0.550437114123183,12.8988583280191));
#10055=CARTESIAN_POINT('Ctrl Pts',(1.26571366128599,-0.461785948136937,
12.9047418643186));
#10056=CARTESIAN_POINT('Ctrl Pts',(1.22252704560661,-0.090826657060951,
12.929606447947));
#10057=CARTESIAN_POINT('Ctrl Pts',(1.22707809586845,0.194176743933125,12.9491546877146));
#10058=CARTESIAN_POINT('Ctrl Pts',(1.28203216841671,0.563034906910546,12.9734317401019));
#10059=CARTESIAN_POINT('Ctrl Pts',(1.2988140034172,0.650595809980168,12.9791308336188));
#10060=CARTESIAN_POINT('Ctrl Pts',(1.32488349736597,0.761514967831724,12.9862711637016));
#10061=CARTESIAN_POINT('Ctrl Pts',(1.33084067171668,0.785608309902471,12.9878174324361));
#10062=CARTESIAN_POINT('Ctrl Pts',(1.34093042815405,0.824482710904736,12.9903052006832));
#10063=CARTESIAN_POINT('Ctrl Pts',(1.34489122514292,0.839306915314272,12.9912521910129));
#10064=CARTESIAN_POINT('Ctrl Pts',(1.35268787498126,0.867673742781844,12.9930612604975));
#10065=CARTESIAN_POINT('Ctrl Pts',(1.35650686044375,0.881220596665855,12.9939238618749));
#10066=CARTESIAN_POINT('Ctrl Pts',(1.36543472480635,0.912113468790976,12.9958881256814));
#10067=CARTESIAN_POINT('Ctrl Pts',(1.37060111974435,0.929442476837498,12.996987891866));
#10068=CARTESIAN_POINT('Ctrl Pts',(1.38739370247584,0.984083857658635,13.0004498078648));
#10069=CARTESIAN_POINT('Ctrl Pts',(1.39955314018012,1.02122957660542,13.0027945547021));
#10070=CARTESIAN_POINT('Ctrl Pts',(1.49870176107478,1.30646112754162,13.0207531970528));
#10071=CARTESIAN_POINT('Ctrl Pts',(1.61507331208986,1.54327973948428,13.0352860904291));
#10072=CARTESIAN_POINT('Ctrl Pts',(1.85236789918476,1.90628884204277,13.0595939793505));
#10073=CARTESIAN_POINT('Ctrl Pts',(1.95700802932465,2.04155797881894,13.0692447930298));
#10074=CARTESIAN_POINT('Ctrl Pts',(2.08559318563472,2.18299845060467,13.0807909941339));
#10075=CARTESIAN_POINT('Ctrl Pts',(2.09947772797619,2.19798236119644,13.0820342101143));
#10076=CARTESIAN_POINT('Ctrl Pts',(2.12032764428936,2.22005842546125,13.0838977238906));
#10077=CARTESIAN_POINT('Ctrl Pts',(2.12718520532033,2.2272523084491,13.0845101030516));
#10078=CARTESIAN_POINT('Ctrl Pts',(2.13898481636893,2.23951652377176,13.0855631408545));
#10079=CARTESIAN_POINT('Ctrl Pts',(2.14391046066186,2.24460246003662,13.0860025331292));
#10080=CARTESIAN_POINT('Ctrl Pts',(2.15512677522783,2.25610766908877,13.0870027149876));
#10081=CARTESIAN_POINT('Ctrl Pts',(2.16142744088259,2.26251675986647,13.0875642751017));
#10082=CARTESIAN_POINT('Ctrl Pts',(2.17862900576883,2.27986855168398,13.0890964190707));
#10083=CARTESIAN_POINT('Ctrl Pts',(2.18958173758774,2.29075921300148,13.0900709167299));
#10084=CARTESIAN_POINT('Ctrl Pts',(2.24450311933146,2.3445897548294,13.0949502089249));
#10085=CARTESIAN_POINT('Ctrl Pts',(2.28961262461102,2.386341659838,13.0989348041721));
#10086=CARTESIAN_POINT('Ctrl Pts',(2.36456371250586,2.45183603102268,13.1054805861793));
#10087=CARTESIAN_POINT('Ctrl Pts',(2.39368405170251,2.4763856195491,13.1080065352424));
#10088=CARTESIAN_POINT('Ctrl Pts',(2.56236217141639,2.61354805183486,13.1225114644826));
#10089=CARTESIAN_POINT('Ctrl Pts',(2.71069190499138,2.71487345370927,13.1347604085088));
#10090=CARTESIAN_POINT('Ctrl Pts',(3.00744471482028,2.88316365151822,13.1576296300736));
#10091=CARTESIAN_POINT('Ctrl Pts',(3.15403622994852,2.95228490901848,13.1682621382635));
#10092=CARTESIAN_POINT('Ctrl Pts',(3.34218049738266,3.02424277043986,13.1810294593323));
#10093=CARTESIAN_POINT('Ctrl Pts',(3.3793991329058,3.0376971433638,13.1835151711712));
#10094=CARTESIAN_POINT('Ctrl Pts',(3.4342448814686,3.05638882207109,13.1871215543392));
#10095=CARTESIAN_POINT('Ctrl Pts',(3.45168288746346,3.06216584696773,13.1882599280882));
#10096=CARTESIAN_POINT('Ctrl Pts',(3.48256472845279,3.07210446405868,13.1902616581366));
#10097=CARTESIAN_POINT('Ctrl Pts',(3.49598808410393,3.07632764692806,13.191127018138));
#10098=CARTESIAN_POINT('Ctrl Pts',(3.5241144939772,3.08497458178052,13.1929305465105));
#10099=CARTESIAN_POINT('Ctrl Pts',(3.53882239549219,3.0893814624092,13.1938681448824));
#10100=CARTESIAN_POINT('Ctrl Pts',(3.57742767059103,3.10064861478459,13.1963150959281));
#10101=CARTESIAN_POINT('Ctrl Pts',(3.60137420508863,3.10733783821667,13.1978188728869));
#10102=CARTESIAN_POINT('Ctrl Pts',(3.70326173620357,3.13453204926887,13.2041604505742));
#10103=CARTESIAN_POINT('Ctrl Pts',(3.78188345793262,3.15238771197374,13.2089130075183));
#10104=CARTESIAN_POINT('Ctrl Pts',(4.0915723936306,3.21060177606796,13.2272053979618));
#10105=CARTESIAN_POINT('Ctrl Pts',(4.32608151635074,3.22863984625599,13.2400819056559));
#10106=CARTESIAN_POINT('Ctrl Pts',(4.70633942201599,3.2163613540936,13.2615140518314));
#10107=CARTESIAN_POINT('Ctrl Pts',(4.8516956392506,3.20174963588584,13.2698575940307));
#10108=CARTESIAN_POINT('Ctrl Pts',(5.01358619258606,3.17428308527813,13.2798014026489));
#10109=CARTESIAN_POINT('Ctrl Pts',(5.03160419382584,3.17106798236126,13.2809173807437));
#10110=CARTESIAN_POINT('Ctrl Pts',(5.05894059214937,3.16594947926375,13.2826259376557));
#10111=CARTESIAN_POINT('Ctrl Pts',(5.06827990273194,3.16415795125306,13.2832124008005));
#10112=CARTESIAN_POINT('Ctrl Pts',(5.08528306823281,3.16081820025487,13.2842853484006));
#10113=CARTESIAN_POINT('Ctrl Pts',(5.09294935231818,3.15928339767642,13.2847710708786));
#10114=CARTESIAN_POINT('Ctrl Pts',(5.11009774708293,3.15578531032237,13.2858619591544));
#10115=CARTESIAN_POINT('Ctrl Pts',(5.1195765482943,3.15380719758422,13.2864679414813));
#10116=CARTESIAN_POINT('Ctrl Pts',(5.14719490018595,3.14791356559026,13.2882420361841));
#10117=CARTESIAN_POINT('Ctrl Pts',(5.16530937330319,3.14388412269432,13.2894162853379));
#10118=CARTESIAN_POINT('Ctrl Pts',(5.32122019252144,3.10778688446259,13.2996090789624));
#10119=CARTESIAN_POINT('Ctrl Pts',(5.45678715339439,3.06683690000413,13.309046941385));
#10120=CARTESIAN_POINT('Ctrl Pts',(5.62939744916173,3.00203255164949,13.3214786776704));
#10121=CARTESIAN_POINT('Ctrl Pts',(5.66928023713543,2.98614290450023,13.3243817022453));
#10122=CARTESIAN_POINT('Ctrl Pts',(5.85031651510964,2.90979122506909,13.3376737535657));
#10123=CARTESIAN_POINT('Ctrl Pts',(5.98736445408275,2.84008127699621,13.3480463773411));
#10124=CARTESIAN_POINT('Ctrl Pts',(6.22004580104891,2.69997171070097,13.3659368928106));
#10125=CARTESIAN_POINT('Ctrl Pts',(6.31775185058082,2.63356833100348,13.3735498445784));
#10126=CARTESIAN_POINT('Ctrl Pts',(6.43307136596196,2.54556286702816,13.382658052534));
#10127=CARTESIAN_POINT('Ctrl Pts',(6.45433247337631,2.52891060354138,13.3843430088537));
#10128=CARTESIAN_POINT('Ctrl Pts',(6.48771493705192,2.50208078932814,13.3869983730876));
#10129=CARTESIAN_POINT('Ctrl Pts',(6.49997458904939,2.49207810020211,13.3879756928641));
#10130=CARTESIAN_POINT('Ctrl Pts',(6.52292226370886,2.47307181113204,13.3898093081554));
#10131=CARTESIAN_POINT('Ctrl Pts',(6.53362631379439,2.46408822485294,13.3906663834845));
#10132=CARTESIAN_POINT('Ctrl Pts',(6.55762212135739,2.44368179230383,13.392591958317));
#10133=CARTESIAN_POINT('Ctrl Pts',(6.57087988256129,2.43221951781021,13.39365880857));
#10134=CARTESIAN_POINT('Ctrl Pts',(6.60466178773215,2.40252768377527,13.3963854087311));
#10135=CARTESIAN_POINT('Ctrl Pts',(6.62504797110731,2.38414279039983,13.3980386770825));
#10136=CARTESIAN_POINT('Ctrl Pts',(6.80378346179067,2.21876400114542,13.4126123459492));
#10137=CARTESIAN_POINT('Ctrl Pts',(6.94721913518784,2.05644818125776,13.4248123958923));
#10138=CARTESIAN_POINT('Ctrl Pts',(7.17167490327287,1.74417835955314,13.4463312502281));
#10139=CARTESIAN_POINT('Ctrl Pts',(7.25911965845381,1.59988827985571,13.4556754827386));
#10140=CARTESIAN_POINT('Ctrl Pts',(7.35617056744006,1.40715669141018,13.4682007101432));
#10141=CARTESIAN_POINT('Ctrl Pts',(7.37652603064583,1.36441402459769,13.4709819276123));
#10142=CARTESIAN_POINT('Ctrl Pts',(7.40872192624013,1.29278542145264,13.4756732593142));
#10143=CARTESIAN_POINT('Ctrl Pts',(7.4210977422972,1.26414704251688,13.4775568634157));
#10144=CARTESIAN_POINT('Ctrl Pts',(7.43756830341546,1.22446059674141,13.4801839681871));
#10145=CARTESIAN_POINT('Ctrl Pts',(7.4420215607347,1.21356199176158,13.4809071498913));
#10146=CARTESIAN_POINT('Ctrl Pts',(7.44943709289846,1.19512584303349,13.4821338013944));
#10147=CARTESIAN_POINT('Ctrl Pts',(7.45243090820416,1.1876009553603,13.4826353983371));
#10148=CARTESIAN_POINT('Ctrl Pts',(7.45810355712397,1.17318491683476,13.4835982609504));
#10149=CARTESIAN_POINT('Ctrl Pts',(7.46078708789358,1.16629571221425,13.4840592223917));
#10150=CARTESIAN_POINT('Ctrl Pts',(7.46714823561781,1.14979763364853,13.4851649827836));
#10151=CARTESIAN_POINT('Ctrl Pts',(7.47080356363207,1.14018033251333,13.4858110749508));
#10152=CARTESIAN_POINT('Ctrl Pts',(7.48378092911438,1.10553781239608,13.4881433469418));
#10153=CARTESIAN_POINT('Ctrl Pts',(7.49283758792597,1.08041522740317,13.4898440107271));
#10154=CARTESIAN_POINT('Ctrl Pts',(7.56284092930072,0.878395494069324,13.5035776530195));
#10155=CARTESIAN_POINT('Ctrl Pts',(7.60858387781865,0.696623788770225,13.5162674048535));
#10156=CARTESIAN_POINT('Ctrl Pts',(7.66541976647591,0.343368413608132,13.540470057364));
#10157=CARTESIAN_POINT('Ctrl Pts',(7.67910509069768,0.17290148099393,13.5519513694079));
#10158=CARTESIAN_POINT('Ctrl Pts',(7.67921886993575,0.0014255959816308,
13.5631165164725));
#10159=CARTESIAN_POINT('Ctrl Pts',(7.67921910621823,0.000712797000042185,
13.563162921892));
#10160=CARTESIAN_POINT('Ctrl Pts',(7.67921910621823,1.97331828652831E-11,
13.5632093210196));
#10161=CARTESIAN_POINT('',(7.67921877062999,0.00147072563195245,13.3168934255997));
#10162=CARTESIAN_POINT('Ctrl Pts',(7.67921910621823,-2.34781276219209E-11,
13.3169799747702));
#10163=CARTESIAN_POINT('Ctrl Pts',(7.67921910621823,0.000490239403011727,
13.3169511295057));
#10164=CARTESIAN_POINT('Ctrl Pts',(7.67921899435662,0.000980481300954709,
13.316922279787));
#10165=CARTESIAN_POINT('Ctrl Pts',(7.67921877062999,0.0014707256322326,
13.3168934255997));
#10166=CARTESIAN_POINT('Ctrl Pts',(7.6792187687556,0.00147482719786989,
13.3168931841947));
#10167=CARTESIAN_POINT('Ctrl Pts',(7.67920381324451,0.0341551767246361,
13.3149697234694));
#10168=CARTESIAN_POINT('Ctrl Pts',(7.67869176533755,0.066832409103204,13.3130272302896));
#10169=CARTESIAN_POINT('Ctrl Pts',(7.67701596931515,0.121087280003743,13.3097618798408));
#10170=CARTESIAN_POINT('Ctrl Pts',(7.67613197904975,0.142671496439738,13.3084522487079));
#10171=CARTESIAN_POINT('Ctrl Pts',(7.67457495974107,0.173183093420942,13.306583935171));
#10172=CARTESIAN_POINT('Ctrl Pts',(7.67408159372043,0.182119587732629,13.3060346618699));
#10173=CARTESIAN_POINT('Ctrl Pts',(7.67311364949827,0.19841843143695,13.305028911093));
#10174=CARTESIAN_POINT('Ctrl Pts',(7.67265100068669,0.205781463906846,13.3045730869004));
#10175=CARTESIAN_POINT('Ctrl Pts',(7.67166754783189,0.220618859610453,13.3036514575909));
#10176=CARTESIAN_POINT('Ctrl Pts',(7.67114596244545,0.228092976882592,13.3031856038319));
#10177=CARTESIAN_POINT('Ctrl Pts',(7.66985949858511,0.245645916032934,13.3020878355876));
#10178=CARTESIAN_POINT('Ctrl Pts',(7.66907326560881,0.255722971971126,13.3014547504164));
#10179=CARTESIAN_POINT('Ctrl Pts',(7.6664827713951,0.287025448232298,13.2994796438253));
#10180=CARTESIAN_POINT('Ctrl Pts',(7.66451549984509,0.308236303210312,13.2981290732907));
#10181=CARTESIAN_POINT('Ctrl Pts',(7.65607497150492,0.390376983252589,13.2928554920203));
#10182=CARTESIAN_POINT('Ctrl Pts',(7.64807519898021,0.451133451762505,13.2888622700012));
#10183=CARTESIAN_POINT('Ctrl Pts',(7.61248406997233,0.672482481119379,13.2740595272985));
#10184=CARTESIAN_POINT('Ctrl Pts',(7.57445842254818,0.831145153881467,13.2629676725312));
#10185=CARTESIAN_POINT('Ctrl Pts',(7.45784536113904,1.19391894370988,13.2372407243241));
#10186=CARTESIAN_POINT('Ctrl Pts',(7.37016663932756,1.39430994304863,13.2227739788541));
#10187=CARTESIAN_POINT('Ctrl Pts',(7.24686129349354,1.61272823893366,13.2069549707656));
#10188=CARTESIAN_POINT('Ctrl Pts',(7.23039973895362,1.64088083106302,13.2049136678247));
#10189=CARTESIAN_POINT('Ctrl Pts',(7.20470477867923,1.68333229679738,13.2018310000153));
#10190=CARTESIAN_POINT('Ctrl Pts',(7.19578111571957,1.6978152623848,13.2007784693871));
#10191=CARTESIAN_POINT('Ctrl Pts',(7.17933882447423,1.72403372313035,13.1988713202093));
#10192=CARTESIAN_POINT('Ctrl Pts',(7.17185799443414,1.73579231952181,13.1980153399034));
#10193=CARTESIAN_POINT('Ctrl Pts',(7.15551989687925,1.76110892453041,13.1961707906214));
#10194=CARTESIAN_POINT('Ctrl Pts',(7.14663620508639,1.77464948926502,13.1951832330464));
#10195=CARTESIAN_POINT('Ctrl Pts',(7.12213343558818,1.8113899065014,13.192500470571));
#10196=CARTESIAN_POINT('Ctrl Pts',(7.10631360892998,1.8344546590993,13.1908128297048));
#10197=CARTESIAN_POINT('Ctrl Pts',(7.02009683401578,1.95671277920615,13.181843496809));
#10198=CARTESIAN_POINT('Ctrl Pts',(6.94442300520664,2.05207265756611,13.1747679709686));
#10199=CARTESIAN_POINT('Ctrl Pts',(6.6961399381897,2.33095796738833,13.1534577150527));
#10200=CARTESIAN_POINT('Ctrl Pts',(6.50730971249028,2.49870532792051,13.1397892186547));
#10201=CARTESIAN_POINT('Ctrl Pts',(6.25442653781677,2.67519687004011,13.1220223134124));
#10202=CARTESIAN_POINT('Ctrl Pts',(6.20710910792218,2.70639762280815,13.1187148839667));
#10203=CARTESIAN_POINT('Ctrl Pts',(6.13856035875061,2.7490481796493,13.1139107569189));
#10204=CARTESIAN_POINT('Ctrl Pts',(6.11798303048373,2.76153368330714,13.1124670407894));
#10205=CARTESIAN_POINT('Ctrl Pts',(6.08586864287728,2.78053055028302,13.110208339515));
#10206=CARTESIAN_POINT('Ctrl Pts',(6.07442760828103,2.78720348439878,13.1094025820518));
#10207=CARTESIAN_POINT('Ctrl Pts',(6.05302258814588,2.79951166725186,13.107892471534));
#10208=CARTESIAN_POINT('Ctrl Pts',(6.04306903576269,2.80516474562825,13.1071892087795));
#10209=CARTESIAN_POINT('Ctrl Pts',(6.02615221544345,2.81465374401116,13.1059918275921));
#10210=CARTESIAN_POINT('Ctrl Pts',(6.0192043684039,2.81851720954874,13.1054994495111));
#10211=CARTESIAN_POINT('Ctrl Pts',(6.00578195545449,2.82591607735439,13.1045469326737));
#10212=CARTESIAN_POINT('Ctrl Pts',(5.99930943693048,2.82945501685345,13.1040870398865));
#10213=CARTESIAN_POINT('Ctrl Pts',(5.98207452954156,2.83880172167028,13.1028610427401));
#10214=CARTESIAN_POINT('Ctrl Pts',(5.97129125984596,2.84457043404316,13.1020925320432));
#10215=CARTESIAN_POINT('Ctrl Pts',(5.93235403518063,2.86511644726083,13.0993130402351));
#10216=CARTESIAN_POINT('Ctrl Pts',(5.90401558841697,2.87953773805855,13.097281748021));
#10217=CARTESIAN_POINT('Ctrl Pts',(5.56561613348809,3.04549001940456,13.0729670581777));
#10218=CARTESIAN_POINT('Ctrl Pts',(5.23335666464999,3.1466996842052,13.0488180794679));
#10219=CARTESIAN_POINT('Ctrl Pts',(4.82905732106831,3.20175649558625,13.0221877117035));
#10220=CARTESIAN_POINT('Ctrl Pts',(4.76655263534069,3.20841326552862,13.0181350829883));
#10221=CARTESIAN_POINT('Ctrl Pts',(4.65886056695671,3.21670559904264,13.0112642092798));
#10222=CARTESIAN_POINT('Ctrl Pts',(4.61376173223752,3.2192260834208,13.0084201903498));
#10223=CARTESIAN_POINT('Ctrl Pts',(4.54927820309124,3.22147151244244,13.0043994024005));
#10224=CARTESIAN_POINT('Ctrl Pts',(4.52992749134325,3.22197084496574,13.0031986628876));
#10225=CARTESIAN_POINT('Ctrl Pts',(4.49635149315902,3.22253460324911,13.0011250584373));
#10226=CARTESIAN_POINT('Ctrl Pts',(4.48212827316133,3.22267924115812,13.0002497125702));
#10227=CARTESIAN_POINT('Ctrl Pts',(4.45294571398415,3.222782790176,12.9984598167093));
#10228=CARTESIAN_POINT('Ctrl Pts',(4.43798666812938,3.22273171987286,12.9975455998804));
#10229=CARTESIAN_POINT('Ctrl Pts',(4.39997950722119,3.22233731826011,12.9952308652837));
#10230=CARTESIAN_POINT('Ctrl Pts',(4.37693348163165,3.22185086466744,12.9938348384292));
#10231=CARTESIAN_POINT('Ctrl Pts',(4.28842649284819,3.21903240249337,12.988500519426));
#10232=CARTESIAN_POINT('Ctrl Pts',(4.22303456711213,3.21495211817029,12.9846166192997));
#10233=CARTESIAN_POINT('Ctrl Pts',(3.82487465482195,3.17789417989429,12.9612252041445));
#10234=CARTESIAN_POINT('Ctrl Pts',(3.49884225918399,3.09529230279362,12.9434114911611));
#10235=CARTESIAN_POINT('Ctrl Pts',(3.14834390018076,2.94569412298596,12.9212806630537));
#10236=CARTESIAN_POINT('Ctrl Pts',(3.10573094069481,2.9263990494975,12.9185314203321));
#10237=CARTESIAN_POINT('Ctrl Pts',(3.03567049819908,2.89281956792869,12.9138890654744));
#10238=CARTESIAN_POINT('Ctrl Pts',(3.00798081011377,2.87905457277214,12.9120217628384));
#10239=CARTESIAN_POINT('Ctrl Pts',(2.97006541102245,2.85952080884865,12.9094138491821));
#10240=CARTESIAN_POINT('Ctrl Pts',(2.95966578189501,2.85409092352391,12.9086931724371));
#10241=CARTESIAN_POINT('Ctrl Pts',(2.94214561115178,2.84482114719977,12.9074695724265));
#10242=CARTESIAN_POINT('Ctrl Pts',(2.93500933157743,2.841010939726,12.9069685009313));
#10243=CARTESIAN_POINT('Ctrl Pts',(2.92137187678723,2.83366350071366,12.906005674878));
#10244=CARTESIAN_POINT('Ctrl Pts',(2.91486843024113,2.83013068466764,12.9055442184075));
#10245=CARTESIAN_POINT('Ctrl Pts',(2.89932614673029,2.82161830578856,12.9044359875086));
#10246=CARTESIAN_POINT('Ctrl Pts',(2.89029901177816,2.81661770361597,12.903787906869));
#10247=CARTESIAN_POINT('Ctrl Pts',(2.85779971090961,2.79841010176745,12.9014391791299));
#10248=CARTESIAN_POINT('Ctrl Pts',(2.83447004431859,2.7849527583687,12.8997237796098));
#10249=CARTESIAN_POINT('Ctrl Pts',(2.66584667633639,2.68484764025082,12.8871249561621));
#10250=CARTESIAN_POINT('Ctrl Pts',(2.52741954039008,2.58717848896796,12.8757034219781));
#10251=CARTESIAN_POINT('Ctrl Pts',(2.27798024077954,2.37999320192958,12.8537674463824));
#10252=CARTESIAN_POINT('Ctrl Pts',(2.16595314362284,2.27238306191774,12.8432842875182));
#10253=CARTESIAN_POINT('Ctrl Pts',(1.98270926928234,2.06898544425127,12.8252476824585));
#10254=CARTESIAN_POINT('Ctrl Pts',(1.90823076345392,1.97653118871277,12.8175957438341));
#10255=CARTESIAN_POINT('Ctrl Pts',(1.82323786911562,1.85820933382615,12.8084483277612));
#10256=CARTESIAN_POINT('Ctrl Pts',(1.80773973075249,1.83605050135093,12.8067611715887));
#10257=CARTESIAN_POINT('Ctrl Pts',(1.78361391579044,1.80061468314072,12.8041032200917));
#10258=CARTESIAN_POINT('Ctrl Pts',(1.77480230591938,1.78746504653802,12.8031254888156));
#10259=CARTESIAN_POINT('Ctrl Pts',(1.7583960480067,1.7625874538957,12.8012916207077));
#10260=CARTESIAN_POINT('Ctrl Pts',(1.75078012239798,1.75087403676891,12.8004346999934));
#10261=CARTESIAN_POINT('Ctrl Pts',(1.73379112888625,1.72436910719446,12.7985101535118));
#10262=CARTESIAN_POINT('Ctrl Pts',(1.7244619111404,1.70954990888216,12.7974441706748));
#10263=CARTESIAN_POINT('Ctrl Pts',(1.70084292389648,1.67134465608744,12.7947211088799));
#10264=CARTESIAN_POINT('Ctrl Pts',(1.68672965839136,1.64785074475509,12.7930704834745));
#10265=CARTESIAN_POINT('Ctrl Pts',(1.56633419568821,1.44151451785189,12.7787725176692));
#10266=CARTESIAN_POINT('Ctrl Pts',(1.47798439372229,1.24879489861585,12.7668123694457));
#10267=CARTESIAN_POINT('Ctrl Pts',(1.35364031562009,0.887504212192018,12.7454246640629));
#10268=CARTESIAN_POINT('Ctrl Pts',(1.31102808707795,0.72208242657127,12.7359741007249));
#10269=CARTESIAN_POINT('Ctrl Pts',(1.2733007208603,0.505912383712873,12.7232538653564));
#10270=CARTESIAN_POINT('Ctrl Pts',(1.26599196824303,0.457562516161085,12.7203845244984));
#10271=CARTESIAN_POINT('Ctrl Pts',(1.25573093626501,0.377377089863857,12.7155586696377));
#10272=CARTESIAN_POINT('Ctrl Pts',(1.25214725977861,0.345629323396932,12.7136306506186));
#10273=CARTESIAN_POINT('Ctrl Pts',(1.24787919925338,0.30200920164946,12.7109514988501));
#10274=CARTESIAN_POINT('Ctrl Pts',(1.24678753001809,0.290177390756196,12.7102217536085));
#10275=CARTESIAN_POINT('Ctrl Pts',(1.24506006218668,0.270250704656202,12.7089872333189));
#10276=CARTESIAN_POINT('Ctrl Pts',(1.24438936907204,0.262158828956796,12.7084843876311));
#10277=CARTESIAN_POINT('Ctrl Pts',(1.24316823701675,0.246717261086248,12.7075217583553));
#10278=CARTESIAN_POINT('Ctrl Pts',(1.24261241919079,0.239368075555769,12.7070622953139));
#10279=CARTESIAN_POINT('Ctrl Pts',(1.24120391249241,0.2198544909123,12.7058389567956));
#10280=CARTESIAN_POINT('Ctrl Pts',(1.24039505798525,0.207687188476975,12.7050726936982));
#10281=CARTESIAN_POINT('Ctrl Pts',(1.23773990807846,0.164002115223861,12.7023097672006));
#10282=CARTESIAN_POINT('Ctrl Pts',(1.23628780042375,0.132463312770913,12.7002930985489));
#10283=CARTESIAN_POINT('Ctrl Pts',(1.22448456204126,-0.244311594846807,
12.6759790780607));
#10284=CARTESIAN_POINT('Ctrl Pts',(1.26922898318824,-0.589041015268961,
12.6518085214495));
#10285=CARTESIAN_POINT('Ctrl Pts',(1.38581085210585,-0.980370320995771,
12.625158704807));
#10286=CARTESIAN_POINT('Ctrl Pts',(1.40551539561215,-1.04007229488903,12.6211053095696));
#10287=CARTESIAN_POINT('Ctrl Pts',(1.44236004250517,-1.14162355173332,12.6142332775771));
#10288=CARTESIAN_POINT('Ctrl Pts',(1.45865702174169,-1.18375707821254,12.6113888553529));
#10289=CARTESIAN_POINT('Ctrl Pts',(1.4831962438025,-1.24343908603298,12.6073676045592));
#10290=CARTESIAN_POINT('Ctrl Pts',(1.49071872181435,-1.26127592487877,12.6061667979425));
#10291=CARTESIAN_POINT('Ctrl Pts',(1.50404672723625,-1.29209983173182,12.6040931151261));
#10292=CARTESIAN_POINT('Ctrl Pts',(1.50977830782964,-1.30511808970727,12.603217757476));
#10293=CARTESIAN_POINT('Ctrl Pts',(1.52171391878816,-1.3317482142607,12.6014278710306));
#10294=CARTESIAN_POINT('Ctrl Pts',(1.52792691538541,-1.34535570192071,12.6005136751708));
#10295=CARTESIAN_POINT('Ctrl Pts',(1.54395320699319,-1.37981880262653,12.5981990607555));
#10296=CARTESIAN_POINT('Ctrl Pts',(1.55389600868042,-1.40061352522789,12.5968031321633));
#10297=CARTESIAN_POINT('Ctrl Pts',(1.59294297434135,-1.48007580164221,12.59146965895));
#10298=CARTESIAN_POINT('Ctrl Pts',(1.62361084589942,-1.53796009082808,12.5875864836286));
#10299=CARTESIAN_POINT('Ctrl Pts',(1.82150488730791,-1.88544335459233,12.5641947607128));
#10300=CARTESIAN_POINT('Ctrl Pts',(2.0311709514052,-2.14844655108265,12.5463802934115));
#10301=CARTESIAN_POINT('Ctrl Pts',(2.31196539467383,-2.40611913816037,12.5242485648804));
#10302=CARTESIAN_POINT('Ctrl Pts',(2.34711166352935,-2.43698917163063,12.5214992888348));
#10303=CARTESIAN_POINT('Ctrl Pts',(2.40658716930032,-2.48697764356547,12.5168568829425));
#10304=CARTESIAN_POINT('Ctrl Pts',(2.43054301448473,-2.50653088262194,12.5149895633222));
#10305=CARTESIAN_POINT('Ctrl Pts',(2.46397008586001,-2.53302247447593,12.5123816297132));
#10306=CARTESIAN_POINT('Ctrl Pts',(2.47320425305622,-2.54025898574482,12.5116609503992));
#10307=CARTESIAN_POINT('Ctrl Pts',(2.4888721994674,-2.55239993338525,12.5104373473017));
#10308=CARTESIAN_POINT('Ctrl Pts',(2.49528542216456,-2.55733094515154,12.5099362753104));
#10309=CARTESIAN_POINT('Ctrl Pts',(2.50760133950425,-2.56672685862988,12.5089734493419));
#10310=CARTESIAN_POINT('Ctrl Pts',(2.51350094753726,-2.57119565002111,12.5085119934587));
#10311=CARTESIAN_POINT('Ctrl Pts',(2.52766341740478,-2.58184675647691,12.5074037653441));
#10312=CARTESIAN_POINT('Ctrl Pts',(2.53594062357905,-2.58800973717229,12.5067556869159));
#10313=CARTESIAN_POINT('Ctrl Pts',(2.56592626462596,-2.6101131553157,12.5044069775835));
#10314=CARTESIAN_POINT('Ctrl Pts',(2.58780403541401,-2.62582056938119,12.5026915945608));
#10315=CARTESIAN_POINT('Ctrl Pts',(2.74860490422625,-2.73824224349261,12.4900861121656));
#10316=CARTESIAN_POINT('Ctrl Pts',(2.89474768326844,-2.8241434324512,12.4786572505607));
#10317=CARTESIAN_POINT('Ctrl Pts',(3.18637835362486,-2.96597844620731,12.4567191528118));
#10318=CARTESIAN_POINT('Ctrl Pts',(3.33053632435742,-3.02364693790833,12.4462411388403));
#10319=CARTESIAN_POINT('Ctrl Pts',(3.59129349320956,-3.10671099593496,12.4282113290634));
#10320=CARTESIAN_POINT('Ctrl Pts',(3.70620321469813,-3.13644525442325,12.4205612013085));
#10321=CARTESIAN_POINT('Ctrl Pts',(3.84901240458805,-3.16509793537076,12.4114156115129));
#10322=CARTESIAN_POINT('Ctrl Pts',(3.87558803885065,-3.17008293929334,12.409728562755));
#10323=CARTESIAN_POINT('Ctrl Pts',(3.91781629810821,-3.17745515259895,12.4070707408858));
#10324=CARTESIAN_POINT('Ctrl Pts',(3.93342872877015,-3.18006240069309,12.4060930329751));
#10325=CARTESIAN_POINT('Ctrl Pts',(3.96285706663703,-3.18475429442643,12.4042591853959));
#10326=CARTESIAN_POINT('Ctrl Pts',(3.97666850011975,-3.18686431301914,12.4034022620349));
#10327=CARTESIAN_POINT('Ctrl Pts',(4.00782061276383,-3.19141641518297,12.4014776791398));
#10328=CARTESIAN_POINT('Ctrl Pts',(4.02516844051225,-3.19380712635601,12.4004116628017));
#10329=CARTESIAN_POINT('Ctrl Pts',(4.06971536768892,-3.19957657568628,12.397688456489));
#10330=CARTESIAN_POINT('Ctrl Pts',(4.09693997644385,-3.20275000468555,12.3960377212503));
#10331=CARTESIAN_POINT('Ctrl Pts',(4.33403374495199,-3.22732542235886,12.3817714188112));
#10332=CARTESIAN_POINT('Ctrl Pts',(4.54550260105667,-3.22842202195993,12.3698392355282));
#10333=CARTESIAN_POINT('Ctrl Pts',(4.91798138865993,-3.19370093934476,12.3488981862817));
#10334=CARTESIAN_POINT('Ctrl Pts',(5.07898401990814,-3.16625772812626,12.3398564251453));
#10335=CARTESIAN_POINT('Ctrl Pts',(5.31514417693471,-3.10728943927905,12.325802516139));
#10336=CARTESIAN_POINT('Ctrl Pts',(5.39232009816608,-3.084923204585,12.3210766100853));
#10337=CARTESIAN_POINT('Ctrl Pts',(5.48394688357945,-3.05461441152921,12.3152161762111));
#10338=CARTESIAN_POINT('Ctrl Pts',(5.49928201198969,-3.04941322299876,12.3142267885455));
#10339=CARTESIAN_POINT('Ctrl Pts',(5.52313552910312,-3.04112189900822,12.3126734865469));
#10340=CARTESIAN_POINT('Ctrl Pts',(5.53168142742914,-3.03811094628702,12.3121141075238));
#10341=CARTESIAN_POINT('Ctrl Pts',(5.54761242537416,-3.03242238627542,12.3110657385685));
#10342=CARTESIAN_POINT('Ctrl Pts',(5.55500053250379,-3.02975378082513,12.3105772774782));
#10343=CARTESIAN_POINT('Ctrl Pts',(5.57185613235565,-3.02359573250288,12.3094577242184));
#10344=CARTESIAN_POINT('Ctrl Pts',(5.5813170353997,-3.02008882343736,12.3088256171271));
#10345=CARTESIAN_POINT('Ctrl Pts',(5.60645625573877,-3.01063586056169,12.3071364030628));
#10346=CARTESIAN_POINT('Ctrl Pts',(5.62210466530556,-3.00461186255643,12.3060749417688));
#10347=CARTESIAN_POINT('Ctrl Pts',(5.7565902080672,-2.95163172675197,12.2968706456738));
#10348=CARTESIAN_POINT('Ctrl Pts',(5.87257240794169,-2.89777310594636,12.2883833695715));
#10349=CARTESIAN_POINT('Ctrl Pts',(6.1708839703949,-2.73705376730441,12.2655890021648));
#10350=CARTESIAN_POINT('Ctrl Pts',(6.34646159466809,-2.6188974861744,12.2511835575357));
#10351=CARTESIAN_POINT('Ctrl Pts',(6.59984640436162,-2.40953727643423,12.2295372133662));
#10352=CARTESIAN_POINT('Ctrl Pts',(6.68631071990159,-2.3297527877283,12.221956470714));
#10353=CARTESIAN_POINT('Ctrl Pts',(6.78702288341076,-2.22606472267618,12.2128809011621));
#10354=CARTESIAN_POINT('Ctrl Pts',(6.80557219741457,-2.20648131556224,12.2111979965357));
#10355=CARTESIAN_POINT('Ctrl Pts',(6.83460386556999,-2.17505004780455,12.2085451760659));
#10356=CARTESIAN_POINT('Ctrl Pts',(6.84524829377783,-2.1633542593425,12.207568369822));
#10357=CARTESIAN_POINT('Ctrl Pts',(6.86513526886889,-2.1411772774605,12.2057353128842));
#10358=CARTESIAN_POINT('Ctrl Pts',(6.87439653775097,-2.13071343971381,12.2048782858412));
#10359=CARTESIAN_POINT('Ctrl Pts',(6.8951242350167,-2.10698508113077,12.2029522902023));
#10360=CARTESIAN_POINT('Ctrl Pts',(6.90655112002233,-2.0936864889109,12.2018849751087));
#10361=CARTESIAN_POINT('Ctrl Pts',(6.93560703155391,-2.05930760673307,12.1991561646069));
#10362=CARTESIAN_POINT('Ctrl Pts',(6.95307621695464,-2.03809363790473,12.1975011699074));
#10363=CARTESIAN_POINT('Ctrl Pts',(7.09807638440555,-1.85734815055128,12.1836334219675));
#10364=CARTESIAN_POINT('Ctrl Pts',(7.21045377309074,-1.68624278667474,12.1720567753647));
#10365=CARTESIAN_POINT('Ctrl Pts',(7.38905693971152,-1.34823458912725,12.1506434341339));
#10366=CARTESIAN_POINT('Ctrl Pts',(7.45903448048918,-1.18422980717912,12.140798669982));
#10367=CARTESIAN_POINT('Ctrl Pts',(7.53044644192222,-0.969097934124585,
12.1276565582434));
#10368=CARTESIAN_POINT('Ctrl Pts',(7.54473358000822,-0.922555974668644,
12.1247993016484));
#10369=CARTESIAN_POINT('Ctrl Pts',(7.56661394311815,-0.845062629067053,
12.1199918723882));
#10370=CARTESIAN_POINT('Ctrl Pts',(7.5748123556431,-0.814289234928381,12.1180699183353));
#10371=CARTESIAN_POINT('Ctrl Pts',(7.58543782081593,-0.771889357120676,
12.115397874579));
#10372=CARTESIAN_POINT('Ctrl Pts',(7.58825893293793,-0.760362326530088,
12.1146690249373));
#10373=CARTESIAN_POINT('Ctrl Pts',(7.59290221207841,-0.740925647767541,
12.1134355851471));
#10374=CARTESIAN_POINT('Ctrl Pts',(7.5947583121602,-0.733024079335304,12.1129329166605));
#10375=CARTESIAN_POINT('Ctrl Pts',(7.59824348841837,-0.717931513197416,
12.111970276808));
#10376=CARTESIAN_POINT('Ctrl Pts',(7.59987776802665,-0.710741801622296,
12.1115106238061));
#10377=CARTESIAN_POINT('Ctrl Pts',(7.60371683245668,-0.693580284382329,
12.1104109929231));
#10378=CARTESIAN_POINT('Ctrl Pts',(7.60589890169122,-0.683603553226435,
12.1097697527912));
#10379=CARTESIAN_POINT('Ctrl Pts',(7.61351266386181,-0.647982021254438,
12.1074735972572));
#10380=CARTESIAN_POINT('Ctrl Pts',(7.6186786751694,-0.622282303269627,12.1058047643183));
#10381=CARTESIAN_POINT('Ctrl Pts',(7.66039724929173,-0.400790100694894,
12.0913335325743));
#10382=CARTESIAN_POINT('Ctrl Pts',(7.67903638184453,-0.202077454925135,
12.0777860519143));
#10383=CARTESIAN_POINT('Ctrl Pts',(7.67921866061281,-0.00195693911181231,
12.0642560913868));
#10384=CARTESIAN_POINT('Ctrl Pts',(7.67921910621818,-0.000978464247689706,
12.0641899395814));
#10385=CARTESIAN_POINT('Ctrl Pts',(7.67921910621823,-1.80065651569973E-10,
12.0641237905203));
#10386=CARTESIAN_POINT('Origin',(4.45646910621825,-5.13094777615093E-16,
-2.31077344927308));
#10387=CARTESIAN_POINT('',(7.67921909946346,0.000172060260772193,10.8112112210413));
#10388=CARTESIAN_POINT('',(7.67921910621823,4.13684814843145E-12,11.0603093566956));
#10389=CARTESIAN_POINT('',(7.67921910621823,-3.51191647465084E-13,-2.31077344927308));
#10390=CARTESIAN_POINT('',(7.67921883037524,0.00133339637767557,12.3082266921078));
#10391=CARTESIAN_POINT('Ctrl Pts',(7.67921910621823,4.13684814843145E-12,
11.0603093566956));
#10392=CARTESIAN_POINT('Ctrl Pts',(7.67921910621823,-0.000978691749929005,
11.0603640893182));
#10393=CARTESIAN_POINT('Ctrl Pts',(7.6792186604013,-0.00195739598008107,
11.0604188236236));
#10394=CARTESIAN_POINT('Ctrl Pts',(7.67904758692959,-0.189731801402226,
11.0709203693113));
#10395=CARTESIAN_POINT('Ctrl Pts',(7.66263724333298,-0.376135903192157,
11.0813693796804));
#10396=CARTESIAN_POINT('Ctrl Pts',(7.62554174357558,-0.586353128666877,
11.0941687338931));
#10397=CARTESIAN_POINT('Ctrl Pts',(7.62057205216903,-0.612604125605327,
11.0957857537902));
#10398=CARTESIAN_POINT('Ctrl Pts',(7.61323707430009,-0.648875527346521,
11.0980497544362));
#10399=CARTESIAN_POINT('Ctrl Pts',(7.61114912889885,-0.658951744915312,
11.0986818887872));
#10400=CARTESIAN_POINT('Ctrl Pts',(7.60747807361002,-0.676250486208489,
11.0997728929118));
#10401=CARTESIAN_POINT('Ctrl Pts',(7.60591828335012,-0.68347795191097,11.1002304507979));
#10402=CARTESIAN_POINT('Ctrl Pts',(7.60259803063439,-0.698610002476913,
11.1011921894131));
#10403=CARTESIAN_POINT('Ctrl Pts',(7.60083263348986,-0.706513374217232,
11.1016966607099));
#10404=CARTESIAN_POINT('Ctrl Pts',(7.59642807764261,-0.725888271816524,
11.102938529704));
#10405=CARTESIAN_POINT('Ctrl Pts',(7.59375583437939,-0.737352087267582,
11.1036777791226));
#10406=CARTESIAN_POINT('Ctrl Pts',(7.58377558417166,-0.779130369775862,
11.1063875035056));
#10407=CARTESIAN_POINT('Ctrl Pts',(7.57609076160968,-0.809351900783152,
11.1083777567132));
#10408=CARTESIAN_POINT('Ctrl Pts',(7.55564617089128,-0.885131161045326,
11.1134361643206));
#10409=CARTESIAN_POINT('Ctrl Pts',(7.54231972362599,-0.930527356070157,
11.1165287636591));
#10410=CARTESIAN_POINT('Ctrl Pts',(7.47706380636555,-1.13597345241519,11.1307621369488));
#10411=CARTESIAN_POINT('Ctrl Pts',(7.4136496190919,-1.29209444827668,11.1422265556533));
#10412=CARTESIAN_POINT('Ctrl Pts',(7.24954036859994,-1.61994659645458,11.1669649109007));
#10413=CARTESIAN_POINT('Ctrl Pts',(7.14453799737394,-1.78879369389825,11.1801285828953));
#10414=CARTESIAN_POINT('Ctrl Pts',(6.99939537129697,-1.98025042203995,11.1953789822275));
#10415=CARTESIAN_POINT('Ctrl Pts',(6.97348954364359,-2.01307578225376,11.1980080857866));
#10416=CARTESIAN_POINT('Ctrl Pts',(6.93516356939034,-2.05974179764837,11.2017685004541));
#10417=CARTESIAN_POINT('Ctrl Pts',(6.92325183129595,-2.07399265310841,11.2029200267265));
#10418=CARTESIAN_POINT('Ctrl Pts',(6.90204912210327,-2.09891785632107,11.2049399947677));
#10419=CARTESIAN_POINT('Ctrl Pts',(6.89280988842858,-2.10963536772769,11.2058105170673));
#10420=CARTESIAN_POINT('Ctrl Pts',(6.87354844187395,-2.13168333783996,11.2076056087064));
#10421=CARTESIAN_POINT('Ctrl Pts',(6.86351642726592,-2.14300480031042,11.208529741018));
#10422=CARTESIAN_POINT('Ctrl Pts',(6.83748225095625,-2.17197177008911,11.2109006582316));
#10423=CARTESIAN_POINT('Ctrl Pts',(6.82136331771991,-2.18951144789662,11.2123425019607));
#10424=CARTESIAN_POINT('Ctrl Pts',(6.75109062967667,-2.26429658693185,11.218519729137));
#10425=CARTESIAN_POINT('Ctrl Pts',(6.69503938127266,-2.31972661717589,11.2231731475022));
#10426=CARTESIAN_POINT('Ctrl Pts',(6.53537825877686,-2.46643548092471,11.2357796146883));
#10427=CARTESIAN_POINT('Ctrl Pts',(6.42784844943309,-2.55320089576116,11.2435659992456));
#10428=CARTESIAN_POINT('Ctrl Pts',(6.13667874027008,-2.75875007111114,11.2635291721455));
#10429=CARTESIAN_POINT('Ctrl Pts',(5.94595913438762,-2.86621754563971,11.275555351935));
#10430=CARTESIAN_POINT('Ctrl Pts',(5.71154865503173,-2.96855104290203,11.290741840794));
#10431=CARTESIAN_POINT('Ctrl Pts',(5.67697098965047,-2.98293393263337,11.2929925309254));
#10432=CARTESIAN_POINT('Ctrl Pts',(5.63001147617826,-3.00151400845297,11.2960734256265));
#10433=CARTESIAN_POINT('Ctrl Pts',(5.61784181895103,-3.00624374355983,11.2968740184334));
#10434=CARTESIAN_POINT('Ctrl Pts',(5.59860120598885,-3.01358733997101,11.2981437043337));
#10435=CARTESIAN_POINT('Ctrl Pts',(5.59154908833675,-3.01625062294471,11.2986099000534));
#10436=CARTESIAN_POINT('Ctrl Pts',(5.57700487189572,-3.02168512123565,11.2995732058822));
#10437=CARTESIAN_POINT('Ctrl Pts',(5.56951179144285,-3.02445323148031,11.3000705052422));
#10438=CARTESIAN_POINT('Ctrl Pts',(5.55150579438006,-3.03102907209611,11.3012678365657));
#10439=CARTESIAN_POINT('Ctrl Pts',(5.54098325279889,-3.0348099844112,11.3019694256215));
#10440=CARTESIAN_POINT('Ctrl Pts',(5.50463489484315,-3.04765733281829,11.3043988921674));
#10441=CARTESIAN_POINT('Ctrl Pts',(5.47871418307278,-3.05644918587328,11.3061416995402));
#10442=CARTESIAN_POINT('Ctrl Pts',(5.41491064716071,-3.07718785343146,11.3104514079697));
#10443=CARTESIAN_POINT('Ctrl Pts',(5.37691354786026,-3.08876626081083,11.3130349096823));
#10444=CARTESIAN_POINT('Ctrl Pts',(5.22051589591655,-3.13328145452372,11.3237115703974));
#10445=CARTESIAN_POINT('Ctrl Pts',(5.10049698743856,-3.16013365532247,11.3320005480398));
#10446=CARTESIAN_POINT('Ctrl Pts',(4.72235662512426,-3.22229685985559,11.3579195217586));
#10447=CARTESIAN_POINT('Ctrl Pts',(4.46124441515921,-3.23325226299835,11.3754404989111));
#10448=CARTESIAN_POINT('Ctrl Pts',(4.16241650436121,-3.2095479040965,11.3944371762699));
#10449=CARTESIAN_POINT('Ctrl Pts',(4.12326515513776,-3.20571989235086,11.3969076814506));
#10450=CARTESIAN_POINT('Ctrl Pts',(4.06618514457591,-3.19908184221559,11.4004840681602));
#10451=CARTESIAN_POINT('Ctrl Pts',(4.04819573555253,-3.19683579187826,11.4016075110291));
#10452=CARTESIAN_POINT('Ctrl Pts',(4.0162684177267,-3.19257563687982,11.4035950748661));
#10453=CARTESIAN_POINT('Ctrl Pts',(4.00232308227447,-3.19062176421459,11.4044610681076));
#10454=CARTESIAN_POINT('Ctrl Pts',(3.97323172784513,-3.18635119673012,11.4062633159448));
#10455=CARTESIAN_POINT('Ctrl Pts',(3.95808849479013,-3.18401775931291,11.4071990187233));
#10456=CARTESIAN_POINT('Ctrl Pts',(3.91856225998225,-3.17763821995725,11.4096352968336));
#10457=CARTESIAN_POINT('Ctrl Pts',(3.89420786100196,-3.17341941385261,11.4111303872281));
#10458=CARTESIAN_POINT('Ctrl Pts',(3.78338083700313,-3.15290540173152,11.4179091869772));
#10459=CARTESIAN_POINT('Ctrl Pts',(3.69754517663288,-3.13335232264249,11.4230890407422));
#10460=CARTESIAN_POINT('Ctrl Pts',(3.34676165286698,-3.03818126721864,11.4441297859574));
#10461=CARTESIAN_POINT('Ctrl Pts',(3.0912781516922,-2.93227525318054,11.4590455379355));
#10462=CARTESIAN_POINT('Ctrl Pts',(2.83184276159427,-2.7833913837344,11.4761535701754));
#10463=CARTESIAN_POINT('Ctrl Pts',(2.81143444126037,-2.77137858590893,11.4775144258895));
#10464=CARTESIAN_POINT('Ctrl Pts',(2.72529584922079,-2.71938876111501,11.4833303972237));
#10465=CARTESIAN_POINT('Ctrl Pts',(2.6608810191872,-2.67729294076745,11.487859785427));
#10466=CARTESIAN_POINT('Ctrl Pts',(2.58451951153603,-2.62339401083963,11.4935312901317));
#10467=CARTESIAN_POINT('Ctrl Pts',(2.57107353285406,-2.61374729582814,11.4945417496268));
#10468=CARTESIAN_POINT('Ctrl Pts',(2.55023763166598,-2.59855430705072,11.4961270654055));
#10469=CARTESIAN_POINT('Ctrl Pts',(2.54279604115322,-2.59307892597518,11.4966971886456));
#10470=CARTESIAN_POINT('Ctrl Pts',(2.52908845097391,-2.58290199957926,11.4977548527623));
#10471=CARTESIAN_POINT('Ctrl Pts',(2.52281595714934,-2.57820953851906,11.4982417705361));
#10472=CARTESIAN_POINT('Ctrl Pts',(2.50857047234511,-2.56747124502946,11.4993542976546));
#10473=CARTESIAN_POINT('Ctrl Pts',(2.50060852705559,-2.56141114826782,11.4999808849298));
#10474=CARTESIAN_POINT('Ctrl Pts',(2.47620531938287,-2.54265694787415,11.5019157958421));
#10475=CARTESIAN_POINT('Ctrl Pts',(2.45985882884333,-2.52984117445728,11.5032321891396));
#10476=CARTESIAN_POINT('Ctrl Pts',(2.42199608070531,-2.49956096045932,11.5063267764986));
#10477=CARTESIAN_POINT('Ctrl Pts',(2.40057918344838,-2.48197542362974,11.5081121610438));
#10478=CARTESIAN_POINT('Ctrl Pts',(2.32605653766171,-2.41915808436957,11.5144410230817));
#10479=CARTESIAN_POINT('Ctrl Pts',(2.2741974848701,-2.37248243873286,11.5190568512391));
#10480=CARTESIAN_POINT('Ctrl Pts',(2.07052539828312,-2.17683678891236,11.5379351860183));
#10481=CARTESIAN_POINT('Ctrl Pts',(1.93210077453762,-2.01467599240331,11.5524984109024));
#10482=CARTESIAN_POINT('Ctrl Pts',(1.73140636231103,-1.72609953531858,11.5758291490185));
#10483=CARTESIAN_POINT('Ctrl Pts',(1.65958750919274,-1.60712439048832,11.5848402089506));
#10484=CARTESIAN_POINT('Ctrl Pts',(1.58355731945138,-1.46054309564896,11.5952268862625));
#10485=CARTESIAN_POINT('Ctrl Pts',(1.57174199827352,-1.43706570734369,11.5968700235363));
#10486=CARTESIAN_POINT('Ctrl Pts',(1.55268457107457,-1.39801564115407,11.5995700282398));
#10487=CARTESIAN_POINT('Ctrl Pts',(1.54527755670816,-1.38252527635991,11.6006325923202));
#10488=CARTESIAN_POINT('Ctrl Pts',(1.53207895050924,-1.35434644216353,11.6025504687986));
#10489=CARTESIAN_POINT('Ctrl Pts',(1.52624530070121,-1.34167825035857,11.6034072175087));
#10490=CARTESIAN_POINT('Ctrl Pts',(1.51386611533915,-1.31433006817151,11.6052452383843));
#10491=CARTESIAN_POINT('Ctrl Pts',(1.50734777256357,-1.29963812811037,11.6062255604608));
#10492=CARTESIAN_POINT('Ctrl Pts',(1.48971303192609,-1.25907459335024,11.6089131165678));
#10493=CARTESIAN_POINT('Ctrl Pts',(1.47882520381993,-1.23310474115358,11.6106125716609));
#10494=CARTESIAN_POINT('Ctrl Pts',(1.41624538143159,-1.07817416417145,11.6206317981295));
#10495=CARTESIAN_POINT('Ctrl Pts',(1.37259289356336,-0.946115242427954,
11.6286760763592));
#10496=CARTESIAN_POINT('Ctrl Pts',(1.28980684874658,-0.627994041516914,
11.6473414407405));
#10497=CARTESIAN_POINT('Ctrl Pts',(1.25833077457372,-0.440494492926915,
11.6577824273708));
#10498=CARTESIAN_POINT('Ctrl Pts',(1.23373667137521,-0.126075299624717,
11.6756424952873));
#10499=CARTESIAN_POINT('Ctrl Pts',(1.23127269959557,-0.000380615296982113,
11.6828823604304));
#10500=CARTESIAN_POINT('Ctrl Pts',(1.23679864356387,0.141844133949329,11.6914988498626));
#10501=CARTESIAN_POINT('Ctrl Pts',(1.23757863459981,0.15856150566911,11.6925183421518));
#10502=CARTESIAN_POINT('Ctrl Pts',(1.2390370478985,0.185337916165719,11.6941630826639));
#10503=CARTESIAN_POINT('Ctrl Pts',(1.23963254275298,0.195401409026146,11.6947839077818));
#10504=CARTESIAN_POINT('Ctrl Pts',(1.24077603574011,0.213301064458868,11.6958931752251));
#10505=CARTESIAN_POINT('Ctrl Pts',(1.24130547906815,0.221138229832411,11.6963805798441));
#10506=CARTESIAN_POINT('Ctrl Pts',(1.24250789712175,0.238019218530842,11.6974342263589));
#10507=CARTESIAN_POINT('Ctrl Pts',(1.24319038174068,0.247062008491229,11.6980009656996));
#10508=CARTESIAN_POINT('Ctrl Pts',(1.24520044188864,0.27227635048743,11.6995874803384));
#10509=CARTESIAN_POINT('Ctrl Pts',(1.24661197599933,0.28844067589552,11.7006117389568));
#10510=CARTESIAN_POINT('Ctrl Pts',(1.25579314380662,0.385147208826615,11.7067798460935));
#10511=CARTESIAN_POINT('Ctrl Pts',(1.26647125483765,0.465377637834308,11.7120638974129));
#10512=CARTESIAN_POINT('Ctrl Pts',(1.30762353524697,0.70516721361332,11.7281997086415));
#10513=CARTESIAN_POINT('Ctrl Pts',(1.34714905757414,0.862911292366838,11.739264962974));
#10514=CARTESIAN_POINT('Ctrl Pts',(1.46497644901045,1.21721302943449,11.764441969432));
#10515=CARTESIAN_POINT('Ctrl Pts',(1.55107007936994,1.41043310090803,11.7783901046834));
#10516=CARTESIAN_POINT('Ctrl Pts',(1.6690102569144,1.61769647661509,11.7934051510063));
#10517=CARTESIAN_POINT('Ctrl Pts',(1.68286876840089,1.64134395165133,11.7951199783696));
#10518=CARTESIAN_POINT('Ctrl Pts',(1.70607413426041,1.67980705473906,11.7979126286919));
#10519=CARTESIAN_POINT('Ctrl Pts',(1.71524286721299,1.69472799259804,11.798996846783));
#10520=CARTESIAN_POINT('Ctrl Pts',(1.73194509131987,1.7214185124042,11.8009381139648));
#10521=CARTESIAN_POINT('Ctrl Pts',(1.73943431278229,1.73321514637385,11.8017967610808));
#10522=CARTESIAN_POINT('Ctrl Pts',(1.75557159269913,1.75827210365081,11.8036221638665));
#10523=CARTESIAN_POINT('Ctrl Pts',(1.76424113675216,1.77151820296095,11.8045880925586));
#10524=CARTESIAN_POINT('Ctrl Pts',(1.78798410413118,1.80721794278911,11.8071943451218));
#10525=CARTESIAN_POINT('Ctrl Pts',(1.80324332580989,1.82954691793712,11.8088276690067));
#10526=CARTESIAN_POINT('Ctrl Pts',(1.8869591174586,1.94879854200651,11.8175726274125));
#10527=CARTESIAN_POINT('Ctrl Pts',(1.96045186665671,2.04208221883733,11.8244876130443));
#10528=CARTESIAN_POINT('Ctrl Pts',(2.14157176600435,2.24754556426695,11.8401459484117));
#10529=CARTESIAN_POINT('Ctrl Pts',(2.25249498917068,2.35641910651263,11.8487713625466));
#10530=CARTESIAN_POINT('Ctrl Pts',(2.49970191536184,2.56627252074296,11.8669283903286));
#10531=CARTESIAN_POINT('Ctrl Pts',(2.63696350998806,2.66534761487728,11.876446943503));
#10532=CARTESIAN_POINT('Ctrl Pts',(2.80434943085274,2.76719055605803,11.8881926546349));
#10533=CARTESIAN_POINT('Ctrl Pts',(2.82753273765578,2.78090078839968,11.8898225452397));
#10534=CARTESIAN_POINT('Ctrl Pts',(2.85983290088742,2.79946010972262,11.8921015057698));
#10535=CARTESIAN_POINT('Ctrl Pts',(2.86880602333693,2.8045587900115,11.8927354660463));
#10536=CARTESIAN_POINT('Ctrl Pts',(2.88425633767143,2.81324001119805,11.89382878287));
#10537=CARTESIAN_POINT('Ctrl Pts',(2.89072173162477,2.81684353604128,11.894286814871));
#10538=CARTESIAN_POINT('Ctrl Pts',(2.90428023565949,2.82433934489387,11.8952485542498));
#10539=CARTESIAN_POINT('Ctrl Pts',(2.91137563640776,2.82822721673375,11.8957525461371));
#10540=CARTESIAN_POINT('Ctrl Pts',(2.92879687160709,2.83768792987388,11.8969915598155));
#10541=CARTESIAN_POINT('Ctrl Pts',(2.93913858890091,2.84323114342978,11.8977284144185));
#10542=CARTESIAN_POINT('Ctrl Pts',(2.97684959418558,2.86318009722167,11.9004195797089));
#10543=CARTESIAN_POINT('Ctrl Pts',(3.00439465755385,2.87724760854169,11.9023933256723));
#10544=CARTESIAN_POINT('Ctrl Pts',(3.07410665991517,2.91159418514974,11.9074007530025));
#10545=CARTESIAN_POINT('Ctrl Pts',(3.11651989023072,2.93135502564482,11.9104582955685));
#10546=CARTESIAN_POINT('Ctrl Pts',(3.4656478501972,3.08485794785006,11.9356318364543));
#10547=CARTESIAN_POINT('Ctrl Pts',(3.79107840754225,3.17102644228206,11.9588445125763));
#10548=CARTESIAN_POINT('Ctrl Pts',(4.18889971442039,3.21228580812286,11.984598124893));
#10549=CARTESIAN_POINT('Ctrl Pts',(4.25398196640656,3.21704420846337,11.9887410366056));
#10550=CARTESIAN_POINT('Ctrl Pts',(4.34216371387288,3.22080449791538,11.994262728989));
#10551=CARTESIAN_POINT('Ctrl Pts',(4.3651699440188,3.22153873849655,11.9956949485987));
#10552=CARTESIAN_POINT('Ctrl Pts',(4.40313192585424,3.22234329203948,11.9980448761718));
#10553=CARTESIAN_POINT('Ctrl Pts',(4.41808351676838,3.2225560825376,11.9989670014789));
#10554=CARTESIAN_POINT('Ctrl Pts',(4.44726502520892,3.2227682690688,12.0007602760201));
#10555=CARTESIAN_POINT('Ctrl Pts',(4.46149450482491,3.22277749570648,12.001631711573));
#10556=CARTESIAN_POINT('Ctrl Pts',(4.49510514568959,3.22257668185406,12.0036832185075));
#10557=CARTESIAN_POINT('Ctrl Pts',(4.51448540914642,3.22228604378204,12.0048607490557));
#10558=CARTESIAN_POINT('Ctrl Pts',(4.57915408971273,3.22073260235598,12.0087729133907));
#10559=CARTESIAN_POINT('Ctrl Pts',(4.6244195651695,3.21868964796209,12.0114832539261));
#10560=CARTESIAN_POINT('Ctrl Pts',(4.73259156779437,3.21151921904056,12.0179039516255));
#10561=CARTESIAN_POINT('Ctrl Pts',(4.79542079024282,3.20549711656875,12.0215874103393));
#10562=CARTESIAN_POINT('Ctrl Pts',(5.19165243688261,3.15573739974705,12.0446297194061));
#10563=CARTESIAN_POINT('Ctrl Pts',(5.51659325538989,3.06190208872768,12.0624557908975));
#10564=CARTESIAN_POINT('Ctrl Pts',(5.85575968986766,2.90337153703621,12.0846699154591));
#10565=CARTESIAN_POINT('Ctrl Pts',(5.89011608816558,2.88656135560115,12.0869674869881));
#10566=CARTESIAN_POINT('Ctrl Pts',(5.93588472811248,2.86314867231562,12.0901032031835));
#10567=CARTESIAN_POINT('Ctrl Pts',(5.94756891320646,2.85708107233618,12.0909103830337));
#10568=CARTESIAN_POINT('Ctrl Pts',(5.96590310900927,2.84741702361747,12.0921880139532));
#10569=CARTESIAN_POINT('Ctrl Pts',(5.97257835379497,2.84386839741559,12.0926555044932));
#10570=CARTESIAN_POINT('Ctrl Pts',(5.98612980002014,2.83660304253335,12.0936094161364));
#10571=CARTESIAN_POINT('Ctrl Pts',(5.99300498945145,2.83288477234763,12.0940959461785));
#10572=CARTESIAN_POINT('Ctrl Pts',(6.00928205416367,2.82400505459335,12.0952538266617));
#10573=CARTESIAN_POINT('Ctrl Pts',(6.01867177874385,2.81882163357949,12.0959265503405));
#10574=CARTESIAN_POINT('Ctrl Pts',(6.03870017181669,2.80763452802438,12.0973714406658));
#10575=CARTESIAN_POINT('Ctrl Pts',(6.04933090070736,2.80161704749301,12.0981444229905));
#10576=CARTESIAN_POINT('Ctrl Pts',(6.07849629427805,2.7848884405216,12.1002812902777));
#10577=CARTESIAN_POINT('Ctrl Pts',(6.09695850697849,2.77405304528776,12.1016520884313));
#10578=CARTESIAN_POINT('Ctrl Pts',(6.15630956149059,2.73842048441058,12.1061144379651));
#10579=CARTESIAN_POINT('Ctrl Pts',(6.1967532842698,2.71289786619919,12.1092414831599));
#10580=CARTESIAN_POINT('Ctrl Pts',(6.37984055542981,2.59157898589117,12.1237488907221));
#10581=CARTESIAN_POINT('Ctrl Pts',(6.51524493031847,2.48537287449146,12.1354633572611));
#10582=CARTESIAN_POINT('Ctrl Pts',(6.79735182520336,2.22515669248053,12.1613456969005));
#10583=CARTESIAN_POINT('Ctrl Pts',(6.93863271240567,2.06638515019245,12.1753626016913));
#10584=CARTESIAN_POINT('Ctrl Pts',(7.07942216527227,1.87269474230708,12.1904394314919));
#10585=CARTESIAN_POINT('Ctrl Pts',(7.09524969724317,1.85032575909946,12.1921538182579));
#10586=CARTESIAN_POINT('Ctrl Pts',(7.12072119413416,1.81333531969423,12.19494590011));
#10587=CARTESIAN_POINT('Ctrl Pts',(7.1305344164181,1.79883265085385,12.1960299859318));
#10588=CARTESIAN_POINT('Ctrl Pts',(7.14796495644493,1.77261470307994,12.1979711086328));
#10589=CARTESIAN_POINT('Ctrl Pts',(7.1556251440065,1.76092858764597,12.1988297425504));
#10590=CARTESIAN_POINT('Ctrl Pts',(7.1718021871384,1.73589587020527,12.2006552145705));
#10591=CARTESIAN_POINT('Ctrl Pts',(7.18029720731496,1.72253554453937,12.2016212249853));
#10592=CARTESIAN_POINT('Ctrl Pts',(7.20303866731209,1.68618056162621,12.2042279379456));
#10593=CARTESIAN_POINT('Ctrl Pts',(7.21709481641753,1.66306794696448,12.2058616361951));
#10594=CARTESIAN_POINT('Ctrl Pts',(7.29128521373943,1.53754318610722,12.2146130112867));
#10595=CARTESIAN_POINT('Ctrl Pts',(7.34601833158008,1.43203743172263,12.221533680445));
#10596=CARTESIAN_POINT('Ctrl Pts',(7.50209949664125,1.08558063208721,12.2432565024709));
#10597=CARTESIAN_POINT('Ctrl Pts',(7.58003042799952,0.835282469259103,12.2574077007351));
#10598=CARTESIAN_POINT('Ctrl Pts',(7.63798520752686,0.517579001566154,12.2760516264132));
#10599=CARTESIAN_POINT('Ctrl Pts',(7.64731980758917,0.456512386987226,12.2796696021478));
#10600=CARTESIAN_POINT('Ctrl Pts',(7.65832034987787,0.367487389848901,12.2850418986793));
#10601=CARTESIAN_POINT('Ctrl Pts',(7.66138615378078,0.339713065685527,12.2867317287733));
#10602=CARTESIAN_POINT('Ctrl Pts',(7.66521301089827,0.300357594063791,12.2891500471769));
#10603=CARTESIAN_POINT('Ctrl Pts',(7.66627334392751,0.288805948951008,12.2898627781235));
#10604=CARTESIAN_POINT('Ctrl Pts',(7.6679582024821,0.2692937171048,12.2910719534643));
#10605=CARTESIAN_POINT('Ctrl Pts',(7.66861556138497,0.261335934111689,12.2915665805529));
#10606=CARTESIAN_POINT('Ctrl Pts',(7.66981775725156,0.246092238856737,12.29251704469));
#10607=CARTESIAN_POINT('Ctrl Pts',(7.67036740132274,0.238806803366017,12.29297259082));
#10608=CARTESIAN_POINT('Ctrl Pts',(7.67149353305973,0.223171569119474,12.2939529109828));
#10609=CARTESIAN_POINT('Ctrl Pts',(7.67206227469203,0.214821287746002,12.2944781046257));
#10610=CARTESIAN_POINT('Ctrl Pts',(7.67335950428873,0.194614582118339,12.2957528141746));
#10611=CARTESIAN_POINT('Ctrl Pts',(7.67405497275093,0.182756259358044,12.296504043653));
#10612=CARTESIAN_POINT('Ctrl Pts',(7.67768381420142,0.114419421775526,12.3008503987718));
#10613=CARTESIAN_POINT('Ctrl Pts',(7.67919543476754,0.0578793639106088,
12.304513948662));
#10614=CARTESIAN_POINT('Ctrl Pts',(7.67921883037524,0.00133339637767557,
12.3082266921078));
#10615=CARTESIAN_POINT('Ctrl Pts',(7.6792188285542,0.00133779050316054,
12.3082264035946));
#10616=CARTESIAN_POINT('Ctrl Pts',(7.67921901366479,0.000891857374298317,
12.308255683033));
#10617=CARTESIAN_POINT('Ctrl Pts',(7.67921910621823,0.000445927208297339,
12.3082849653206));
#10618=CARTESIAN_POINT('Ctrl Pts',(7.67921910621823,3.33464896044866E-11,
12.3083142504469));
#10619=CARTESIAN_POINT('Ctrl Pts',(7.67921910621823,-1.80070125477272E-10,
12.0641237905203));
#10620=CARTESIAN_POINT('Ctrl Pts',(7.67921910623054,0.220223674247331,12.0492355694953));
#10621=CARTESIAN_POINT('Ctrl Pts',(7.6566461785926,0.439904518120074,12.0345467987471));
#10622=CARTESIAN_POINT('Ctrl Pts',(7.60348141468906,0.695784317002951,12.0179601641892));
#10623=CARTESIAN_POINT('Ctrl Pts',(7.59436437097806,0.735809650992355,12.0153791528641));
#10624=CARTESIAN_POINT('Ctrl Pts',(7.5803823102935,0.792195940043441,12.0117608083892));
#10625=CARTESIAN_POINT('Ctrl Pts',(7.57614852599569,0.808707889004498,12.0107033809678));
#10626=CARTESIAN_POINT('Ctrl Pts',(7.56814013939585,0.838941864390323,12.0087709310081));
#10627=CARTESIAN_POINT('Ctrl Pts',(7.56440529012875,0.852673887028682,12.0078946503945));
#10628=CARTESIAN_POINT('Ctrl Pts',(7.55663175939393,0.880525260543539,12.0061200941527));
#10629=CARTESIAN_POINT('Ctrl Pts',(7.552587279485,0.894642654354233,12.0052220302843));
#10630=CARTESIAN_POINT('Ctrl Pts',(7.54231194754444,0.929604655910437,12.0030012414111));
#10631=CARTESIAN_POINT('Ctrl Pts',(7.53596619612086,0.950414944436179,12.0016822836236));
#10632=CARTESIAN_POINT('Ctrl Pts',(7.5109721779184,1.02950094478521,11.9966793787643));
#10633=CARTESIAN_POINT('Ctrl Pts',(7.49087576490687,1.08730776049391,11.9930428097661));
#10634=CARTESIAN_POINT('Ctrl Pts',(7.43545603159794,1.23318820622243,11.9838868717474));
#10635=CARTESIAN_POINT('Ctrl Pts',(7.39786705934426,1.32033946090253,11.9784383134237));
#10636=CARTESIAN_POINT('Ctrl Pts',(7.26736789938451,1.58956253537082,11.9614708766129));
#10637=CARTESIAN_POINT('Ctrl Pts',(7.16097357143027,1.76451448333438,11.9502648967615));
#10638=CARTESIAN_POINT('Ctrl Pts',(7.00963137616278,1.9671925982126,11.9358484172731));
#10639=CARTESIAN_POINT('Ctrl Pts',(6.97964616158735,2.00550778828141,11.9330511638447));
#10640=CARTESIAN_POINT('Ctrl Pts',(6.9089977411522,2.09168921400619,11.92655564984));
#10641=CARTESIAN_POINT('Ctrl Pts',(6.8677812061394,2.13907299375599,11.9228334040076));
#10642=CARTESIAN_POINT('Ctrl Pts',(6.81466414182491,2.1966510065224,11.9180735088394));
#10643=CARTESIAN_POINT('Ctrl Pts',(6.80403562790972,2.20800608567754,11.9171228345294));
#10644=CARTESIAN_POINT('Ctrl Pts',(6.78711986355854,2.22581801149646,11.9156116990101));
#10645=CARTESIAN_POINT('Ctrl Pts',(6.7808868500872,2.23232634718757,11.9150552874418));
#10646=CARTESIAN_POINT('Ctrl Pts',(6.76971150626549,2.2438977745161,11.9140582081819));
#10647=CARTESIAN_POINT('Ctrl Pts',(6.76477970281994,2.24897083353874,11.9136183538537));
#10648=CARTESIAN_POINT('Ctrl Pts',(6.75290665460124,2.26110375058687,11.912559858883));
#10649=CARTESIAN_POINT('Ctrl Pts',(6.74594959421759,2.26814785088999,11.911939994256));
#10650=CARTESIAN_POINT('Ctrl Pts',(6.72467346626776,2.28949253943776,11.9100457466175));
#10651=CARTESIAN_POINT('Ctrl Pts',(6.71025236808401,2.30369009788425,11.9087637634295));
#10652=CARTESIAN_POINT('Ctrl Pts',(6.57792824521665,2.43153135117997,11.8970262685726));
#10653=CARTESIAN_POINT('Ctrl Pts',(6.4516689512312,2.53615840650527,11.8860213886354));
#10654=CARTESIAN_POINT('Ctrl Pts',(6.15469770637899,2.74630112738081,11.8614278720506));
#10655=CARTESIAN_POINT('Ctrl Pts',(5.98094434977684,2.84642618032661,11.8478781345625));
#10656=CARTESIAN_POINT('Ctrl Pts',(5.7156013817188,2.96801649833694,11.8288419701231));
#10657=CARTESIAN_POINT('Ctrl Pts',(5.63058958983003,3.0026621195026,11.8229643458874));
#10658=CARTESIAN_POINT('Ctrl Pts',(5.51970978380955,3.04241912504131,11.8155747419029));
#10659=CARTESIAN_POINT('Ctrl Pts',(5.49510576315501,3.05090623087821,11.8139519136509));
#10660=CARTESIAN_POINT('Ctrl Pts',(5.45558650835282,3.06400482378726,11.8113716504733));
#10661=CARTESIAN_POINT('Ctrl Pts',(5.44073629958786,3.06880746368696,11.8104079557328));
#10662=CARTESIAN_POINT('Ctrl Pts',(5.41249211727007,3.0777156779338,11.8085860262564));
#10663=CARTESIAN_POINT('Ctrl Pts',(5.39910516402675,3.08184215432441,11.8077271237873));
#10664=CARTESIAN_POINT('Ctrl Pts',(5.36857705916762,3.09103479594336,11.80577878941));
#10665=CARTESIAN_POINT('Ctrl Pts',(5.35141971937201,3.09604593757507,11.8046911722217));
#10666=CARTESIAN_POINT('Ctrl Pts',(5.29867032934833,3.11097730641304,11.8013692753442));
#10667=CARTESIAN_POINT('Ctrl Pts',(5.26294788974635,3.1204286310937,11.799150165121));
#10668=CARTESIAN_POINT('Ctrl Pts',(5.09016954695058,3.16297636604587,11.7885520867415));
#10669=CARTESIAN_POINT('Ctrl Pts',(4.95119657956384,3.18767108367891,11.7804431528228));
#10670=CARTESIAN_POINT('Ctrl Pts',(4.58726014989438,3.22795634216087,11.7597424254733));
#10671=CARTESIAN_POINT('Ctrl Pts',(4.36151944620187,3.22920725055079,11.7474447921891));
#10672=CARTESIAN_POINT('Ctrl Pts',(4.06116664416522,3.19933418790658,11.7299949288011));
#10673=CARTESIAN_POINT('Ctrl Pts',(3.98512666545837,3.18901827998858,11.7254776524982));
#10674=CARTESIAN_POINT('Ctrl Pts',(3.89323889988093,3.1731943998788,11.7198198290195));
#10675=CARTESIAN_POINT('Ctrl Pts',(3.87696610934467,3.17026295672794,11.7188101978106));
#10676=CARTESIAN_POINT('Ctrl Pts',(3.85164090077474,3.16549928043924,11.7172259452684));
#10677=CARTESIAN_POINT('Ctrl Pts',(3.84257231951007,3.16375308500252,11.716656047468));
#10678=CARTESIAN_POINT('Ctrl Pts',(3.82582614007766,3.16045382328994,11.715598646352));
#10679=CARTESIAN_POINT('Ctrl Pts',(3.81814658605979,3.15891172334973,11.7151117645995));
#10680=CARTESIAN_POINT('Ctrl Pts',(3.80066751894192,3.15533548256719,11.7139991226772));
#10681=CARTESIAN_POINT('Ctrl Pts',(3.79087185604669,3.1532836890576,11.7133723830575));
#10682=CARTESIAN_POINT('Ctrl Pts',(3.76076054193737,3.14683003359098,11.7114363318822));
#10683=CARTESIAN_POINT('Ctrl Pts',(3.74047825306778,3.14227731311064,11.7101189364605));
#10684=CARTESIAN_POINT('Ctrl Pts',(3.69323668938031,3.13119199119303,11.7070215542541));
#10685=CARTESIAN_POINT('Ctrl Pts',(3.66631520671211,3.12450695535757,11.7052343593985));
#10686=CARTESIAN_POINT('Ctrl Pts',(3.57190394239094,3.09976496004786,11.6988966574035));
#10687=CARTESIAN_POINT('Ctrl Pts',(3.50492129018556,3.07986264111225,11.6942735954374));
#10688=CARTESIAN_POINT('Ctrl Pts',(3.23623886210338,2.99042841080317,11.6753436950448));
#10689=CARTESIAN_POINT('Ctrl Pts',(3.04100674687627,2.90311892647591,11.6607353114752));
#10690=CARTESIAN_POINT('Ctrl Pts',(2.73602052805816,2.72859507165688,11.6374175157297));
#10691=CARTESIAN_POINT('Ctrl Pts',(2.62072147831916,2.6523977438883,11.6284579607456));
#10692=CARTESIAN_POINT('Ctrl Pts',(2.48971916744451,2.55317484496912,11.6181211032822));
#10693=CARTESIAN_POINT('Ctrl Pts',(2.46898057113399,2.53706454374651,11.6164793686601));
#10694=CARTESIAN_POINT('Ctrl Pts',(2.43501735358665,2.51000894529688,11.6137812414612));
#10695=CARTESIAN_POINT('Ctrl Pts',(2.42167944198256,2.49920850155493,11.6127191650596));
#10696=CARTESIAN_POINT('Ctrl Pts',(2.39766152151381,2.4794401271263,11.6108018957496));
#10697=CARTESIAN_POINT('Ctrl Pts',(2.38695230920184,2.47050850057202,11.6099452696033));
#10698=CARTESIAN_POINT('Ctrl Pts',(2.36402317226441,2.45113157301568,11.6081072144645));
#10699=CARTESIAN_POINT('Ctrl Pts',(2.35182270974581,2.44066374890149,11.6071267375644));
#10700=CARTESIAN_POINT('Ctrl Pts',(2.31845542800445,2.41159883067978,11.6044379903333));
#10701=CARTESIAN_POINT('Ctrl Pts',(2.29745306211572,2.39281449468743,11.6027375117796));
#10702=CARTESIAN_POINT('Ctrl Pts',(2.17407128205378,2.27951565041241,11.5926933473035));
#10703=CARTESIAN_POINT('Ctrl Pts',(2.07765619194766,2.1787123070302,11.5846268638287));
#10704=CARTESIAN_POINT('Ctrl Pts',(1.86552823064782,1.92599740819466,11.5658940719076));
#10705=CARTESIAN_POINT('Ctrl Pts',(1.75619065494535,1.76944470664022,11.5554096703205));
#10706=CARTESIAN_POINT('Ctrl Pts',(1.59940400760066,1.49625307534337,11.5375651204653));
#10707=CARTESIAN_POINT('Ctrl Pts',(1.54378671469099,1.38487125356914,11.5303919072017));
#10708=CARTESIAN_POINT('Ctrl Pts',(1.48816131788502,1.2552074855191,11.5218502635722));
#10709=CARTESIAN_POINT('Ctrl Pts',(1.48169114895505,1.23979556217569,11.5208320030074));
#10710=CARTESIAN_POINT('Ctrl Pts',(1.47151393111779,1.21501508765922,11.5191889054141));
#10711=CARTESIAN_POINT('Ctrl Pts',(1.46773032463518,1.20567804562248,11.5185684780571));
#10712=CARTESIAN_POINT('Ctrl Pts',(1.46107519190689,1.18903092595743,11.5174596974215));
#10713=CARTESIAN_POINT('Ctrl Pts',(1.45818652740502,1.18172789624985,11.516972379024));
#10714=CARTESIAN_POINT('Ctrl Pts',(1.45201887750108,1.16596683977823,11.5159186562171));
#10715=CARTESIAN_POINT('Ctrl Pts',(1.4487489533227,1.15750564811413,11.5153517525427));
#10716=CARTESIAN_POINT('Ctrl Pts',(1.43972446679359,1.13385761871625,11.5137641485953));
#10717=CARTESIAN_POINT('Ctrl Pts',(1.43404900964207,1.11864116371261,11.5127389547059));
#10718=CARTESIAN_POINT('Ctrl Pts',(1.40068398725088,1.02707854151743,11.5065509939708));
#10719=CARTESIAN_POINT('Ctrl Pts',(1.37577564988708,0.94975706260412,11.5012469955488));
#10720=CARTESIAN_POINT('Ctrl Pts',(1.30995361568709,0.715444949027674,11.4851035086846));
#10721=CARTESIAN_POINT('Ctrl Pts',(1.27794155792669,0.556220906086365,11.4740526136909));
#10722=CARTESIAN_POINT('Ctrl Pts',(1.2321857967585,0.185975661357574,11.4488974658969));
#10723=CARTESIAN_POINT('Ctrl Pts',(1.22692197046327,-0.0253815361453739,
11.4349569508367));
#10724=CARTESIAN_POINT('Ctrl Pts',(1.24435981001886,-0.26310166646629,11.4199489368552));
#10725=CARTESIAN_POINT('Ctrl Pts',(1.24671333211472,-0.290407580425181,
11.41823423667));
#10726=CARTESIAN_POINT('Ctrl Pts',(1.25114104351235,-0.33510624733189,11.4154418129523));
#10727=CARTESIAN_POINT('Ctrl Pts',(1.25300916797354,-0.35251755986187,11.4143576950389));
#10728=CARTESIAN_POINT('Ctrl Pts',(1.2566227920913,-0.383792034940419,11.4124166210896));
#10729=CARTESIAN_POINT('Ctrl Pts',(1.25831669986068,-0.397660603501415,
11.4115580672226));
#10730=CARTESIAN_POINT('Ctrl Pts',(1.26212193619423,-0.427216880753332,
11.4097328787171));
#10731=CARTESIAN_POINT('Ctrl Pts',(1.264258768027,-0.442900978287249,11.4087670707483));
#10732=CARTESIAN_POINT('Ctrl Pts',(1.27035851962529,-0.485332880446873,
11.406161187575));
#10733=CARTESIAN_POINT('Ctrl Pts',(1.27454270339344,-0.512047956223543,
11.4045281100179));
#10734=CARTESIAN_POINT('Ctrl Pts',(1.29889139434481,-0.655661396283384,
11.3957855121279));
#10735=CARTESIAN_POINT('Ctrl Pts',(1.32516328904076,-0.771438434329466,
11.3888725168799));
#10736=CARTESIAN_POINT('Ctrl Pts',(1.40038725642705,-1.03467216221648,11.3732211608344));
#10737=CARTESIAN_POINT('Ctrl Pts',(1.45372761201006,-1.18056276128543,11.364600531952));
#10738=CARTESIAN_POINT('Ctrl Pts',(1.58676839199512,-1.47633202276641,11.3464411885921));
#10739=CARTESIAN_POINT('Ctrl Pts',(1.66820167335284,-1.62489666084929,11.336915467499));
#10740=CARTESIAN_POINT('Ctrl Pts',(1.77566523256052,-1.78889170212943,11.3251616676655));
#10741=CARTESIAN_POINT('Ctrl Pts',(1.79070808459254,-1.81123190095604,11.3235318469473));
#10742=CARTESIAN_POINT('Ctrl Pts',(1.81189935885067,-1.84186723491647,11.3212530115149));
#10743=CARTESIAN_POINT('Ctrl Pts',(1.81781076837829,-1.85032597916519,11.3206191054174));
#10744=CARTESIAN_POINT('Ctrl Pts',(1.82803128458814,-1.86480212271782,11.3195258894289));
#10745=CARTESIAN_POINT('Ctrl Pts',(1.83232072458879,-1.87083339922545,11.3190679039009));
#10746=CARTESIAN_POINT('Ctrl Pts',(1.84134220619562,-1.88342621456326,11.3181062731231));
#10747=CARTESIAN_POINT('Ctrl Pts',(1.84607821012626,-1.88998475481941,11.3176023434937));
#10748=CARTESIAN_POINT('Ctrl Pts',(1.85774280189033,-1.90601070213575,11.3163635059266));
#10749=CARTESIAN_POINT('Ctrl Pts',(1.86469845193362,-1.91545818723699,11.3156267658286));
#10750=CARTESIAN_POINT('Ctrl Pts',(1.89017440807326,-1.94966798776422,11.3129361584839));
#10751=CARTESIAN_POINT('Ctrl Pts',(1.90899861926493,-1.97420052027516,11.3109628647708));
#10752=CARTESIAN_POINT('Ctrl Pts',(1.95717746703219,-2.03515275411314,11.3059567432344));
#10753=CARTESIAN_POINT('Ctrl Pts',(1.98697688944659,-2.07121055852537,11.3029000674229));
#10754=CARTESIAN_POINT('Ctrl Pts',(2.23606312980758,-2.35958992983217,11.2777481393411));
#10755=CARTESIAN_POINT('Ctrl Pts',(2.49262234709484,-2.57706247502939,11.2545572636626));
#10756=CARTESIAN_POINT('Ctrl Pts',(2.83401623413867,-2.78532841998298,11.2288033108617));
#10757=CARTESIAN_POINT('Ctrl Pts',(2.89096202238079,-2.81772892592821,11.224643388743));
#10758=CARTESIAN_POINT('Ctrl Pts',(2.96923153900141,-2.85915604308597,11.2191030593982));
#10759=CARTESIAN_POINT('Ctrl Pts',(2.98971930407134,-2.86972018188014,11.2176687455785));
#10760=CARTESIAN_POINT('Ctrl Pts',(3.02368719361504,-2.88677628452276,11.2153163583304));
#10761=CARTESIAN_POINT('Ctrl Pts',(3.03710205444235,-2.89339567123651,11.2143938481195));
#10762=CARTESIAN_POINT('Ctrl Pts',(3.06336153212007,-2.90612648750706,11.2126005169973));
#10763=CARTESIAN_POINT('Ctrl Pts',(3.07620146085871,-2.91224674638006,11.2117294048702));
#10764=CARTESIAN_POINT('Ctrl Pts',(3.10660948320878,-2.92649470117636,11.2096797364911));
#10765=CARTESIAN_POINT('Ctrl Pts',(3.12421123765801,-2.93454957954183,11.2085037091601));
#10766=CARTESIAN_POINT('Ctrl Pts',(3.18311983945182,-2.96086793377446,11.2046015279199));
#10767=CARTESIAN_POINT('Ctrl Pts',(3.22473900220289,-2.97842215443572,11.2018994959622));
#10768=CARTESIAN_POINT('Ctrl Pts',(3.32511899383177,-3.01829649873181,11.1955018847928));
#10769=CARTESIAN_POINT('Ctrl Pts',(3.38419138395671,-3.03978420454166,11.1918329381576));
#10770=CARTESIAN_POINT('Ctrl Pts',(3.77159633858511,-3.16800347026377,11.1682829642504));
#10771=CARTESIAN_POINT('Ctrl Pts',(4.11456495857461,-3.22309192692174,11.1500374569534));
#10772=CARTESIAN_POINT('Ctrl Pts',(4.49145464435115,-3.22271677207613,11.1275475132918));
#10773=CARTESIAN_POINT('Ctrl Pts',(4.52322871360484,-3.2222151330177,11.125630791769));
#10774=CARTESIAN_POINT('Ctrl Pts',(4.56720963865016,-3.22087000448166,11.1229426981498));
#10775=CARTESIAN_POINT('Ctrl Pts',(4.57942803175382,-3.22042670197447,11.1221921701828));
#10776=CARTESIAN_POINT('Ctrl Pts',(4.59901322797788,-3.21960450152842,11.1209827009971));
#10777=CARTESIAN_POINT('Ctrl Pts',(4.60638190657565,-3.21926981202584,11.1205261941671));
#10778=CARTESIAN_POINT('Ctrl Pts',(4.62185321793741,-3.21851386335856,11.1195645237478));
#10779=CARTESIAN_POINT('Ctrl Pts',(4.62995547006626,-3.21808729988793,11.1190590566389));
#10780=CARTESIAN_POINT('Ctrl Pts',(4.64988859051627,-3.21696237536811,11.1178111072399));
#10781=CARTESIAN_POINT('Ctrl Pts',(4.66171731068068,-3.2162293428344,11.1170667324173));
#10782=CARTESIAN_POINT('Ctrl Pts',(4.70520670843476,-3.21329339198362,11.1143165930574));
#10783=CARTESIAN_POINT('Ctrl Pts',(4.73683724621753,-3.21068814229316,11.1122902910883));
#10784=CARTESIAN_POINT('Ctrl Pts',(4.81665020025041,-3.20292601077256,11.1071199351535));
#10785=CARTESIAN_POINT('Ctrl Pts',(4.86476334008476,-3.19714885221963,11.103950127269));
#10786=CARTESIAN_POINT('Ctrl Pts',(5.08730863716374,-3.16532174860641,11.0890945311827));
#10787=CARTESIAN_POINT('Ctrl Pts',(5.25954232120868,-3.126066361025,11.0770612481191));
#10788=CARTESIAN_POINT('Ctrl Pts',(5.62438551802157,-3.01075414149152,11.0512764874949));
#10789=CARTESIAN_POINT('Ctrl Pts',(5.81468190077913,-2.92983866604257,11.0376553469737));
#10790=CARTESIAN_POINT('Ctrl Pts',(6.02221814101125,-2.81699142197774,11.0227804948697));
#10791=CARTESIAN_POINT('Ctrl Pts',(6.04827422450781,-2.80235031241455,11.0209116022635));
#10792=CARTESIAN_POINT('Ctrl Pts',(6.08861467606917,-2.77893848804436,11.0180152102385));
#10793=CARTESIAN_POINT('Ctrl Pts',(6.10304015938343,-2.77041550410005,11.0169788774665));
#10794=CARTESIAN_POINT('Ctrl Pts',(6.12909592291001,-2.75474561532282,11.0151056958175));
#10795=CARTESIAN_POINT('Ctrl Pts',(6.14074843466152,-2.74763662552363,11.0142674948921));
#10796=CARTESIAN_POINT('Ctrl Pts',(6.16592703566354,-2.73205524634707,11.012455086251));
#10797=CARTESIAN_POINT('Ctrl Pts',(6.17943610946637,-2.72355594795934,11.0114818940404));
#10798=CARTESIAN_POINT('Ctrl Pts',(6.20720905344388,-2.70579312608946,11.0094792104312));
#10799=CARTESIAN_POINT('Ctrl Pts',(6.22146387079355,-2.6965163270345,11.0084502453134));
#10800=CARTESIAN_POINT('Ctrl Pts',(6.29281827183956,-2.64927181028644,11.0032932267952));
#10801=CARTESIAN_POINT('Ctrl Pts',(6.34877175810351,-2.60959978934597,10.9992290454581));
#10802=CARTESIAN_POINT('Ctrl Pts',(6.49246358577995,-2.50066584478156,10.9886913692953));
#10803=CARTESIAN_POINT('Ctrl Pts',(6.57794065420054,-2.42857251610717,10.9823210782168));
#10804=CARTESIAN_POINT('Ctrl Pts',(6.85242546700345,-2.17149198577975,10.9611273833903));
#10805=CARTESIAN_POINT('Ctrl Pts',(7.0223557567631,-1.96778337828671,10.9467807596889));
#10806=CARTESIAN_POINT('Ctrl Pts',(7.18290855974081,-1.71862718751688,10.9290996327766));
#10807=CARTESIAN_POINT('Ctrl Pts',(7.19991957875737,-1.69133995103716,10.9271606304123));
#10808=CARTESIAN_POINT('Ctrl Pts',(7.22286060953618,-1.65328355438285,10.9244462478727));
#10809=CARTESIAN_POINT('Ctrl Pts',(7.22914216457237,-1.64272717181336,10.9236922499977));
#10810=CARTESIAN_POINT('Ctrl Pts',(7.23910431644646,-1.62576548768821,10.9224786281062));
#10811=CARTESIAN_POINT('Ctrl Pts',(7.24282357833584,-1.61938287235636,10.9220214696629));
#10812=CARTESIAN_POINT('Ctrl Pts',(7.2505763285439,-1.60597261801255,10.921059832261));
#10813=CARTESIAN_POINT('Ctrl Pts',(7.25460528627269,-1.59894250445306,10.920555058309));
#10814=CARTESIAN_POINT('Ctrl Pts',(7.26443525670486,-1.58163929210865,10.9193112006158));
#10815=CARTESIAN_POINT('Ctrl Pts',(7.27020641674,-1.57134944867043,10.9185702514656));
#10816=CARTESIAN_POINT('Ctrl Pts',(7.29111549839727,-1.53358450546202,10.9158469576761));
#10817=CARTESIAN_POINT('Ctrl Pts',(7.30590799905327,-1.50592145516734,10.9138445805711));
#10818=CARTESIAN_POINT('Ctrl Pts',(7.34216750077239,-1.43566606181642,10.9087485431914));
#10819=CARTESIAN_POINT('Ctrl Pts',(7.36309669245342,-1.39280575584128,10.9056300007568));
#10820=CARTESIAN_POINT('Ctrl Pts',(7.45464594297158,-1.19426709515922,10.8911902089749));
#10821=CARTESIAN_POINT('Ctrl Pts',(7.51375933613255,-1.0335915424067,10.8795374249385));
#10822=CARTESIAN_POINT('Ctrl Pts',(7.60187594792293,-0.718905664837764,
10.8574962158966));
#10823=CARTESIAN_POINT('Ctrl Pts',(7.63296332552938,-0.565954231945592,
10.8471144209096));
#10824=CARTESIAN_POINT('Ctrl Pts',(7.66177825343877,-0.342041428854369,
10.8325427447077));
#10825=CARTESIAN_POINT('Ctrl Pts',(7.66844056163603,-0.272469536252241,
10.8280987125428));
#10826=CARTESIAN_POINT('Ctrl Pts',(7.67429102637126,-0.17965099168277,10.8222771897009));
#10827=CARTESIAN_POINT('Ctrl Pts',(7.67549736894351,-0.156555029264165,
10.8208373831447));
#10828=CARTESIAN_POINT('Ctrl Pts',(7.67708334470026,-0.118286674984217,
10.8184657677264));
#10829=CARTESIAN_POINT('Ctrl Pts',(7.67760459210728,-0.103121310616642,
10.8175295663393));
#10830=CARTESIAN_POINT('Ctrl Pts',(7.67838502949849,-0.0745352632944399,
10.8157715506668));
#10831=CARTESIAN_POINT('Ctrl Pts',(7.67866751960757,-0.0611155914426918,
10.8149490269002));
#10832=CARTESIAN_POINT('Ctrl Pts',(7.67900178879491,-0.0385312124607307,
10.8135693095553));
#10833=CARTESIAN_POINT('Ctrl Pts',(7.67909832803428,-0.0293674311609509,
10.8130107342684));
#10834=CARTESIAN_POINT('Ctrl Pts',(7.67919852553884,-0.0133846288352081,
10.8120386483023));
#10835=CARTESIAN_POINT('Ctrl Pts',(7.67921963167649,-0.00656581911898159,
10.8116246026049));
#10836=CARTESIAN_POINT('Ctrl Pts',(7.67921909628439,0.000253038698648237,
10.8112112210413));
#10837=CARTESIAN_POINT('Origin',(4.45646910621825,-5.13094777615093E-16,
-2.31077344927308));
#10838=CARTESIAN_POINT('',(7.67921910621823,-1.20018596680688E-11,9.56539764702567));
#10839=CARTESIAN_POINT('',(7.67921908851299,0.000264017416110453,9.81380927132941));
#10840=CARTESIAN_POINT('',(7.67921910621823,-3.51191647465084E-13,-2.31077344927308));
#10841=CARTESIAN_POINT('Ctrl Pts',(7.67921907731647,0.000431608942485311,
9.81380931041028));
#10842=CARTESIAN_POINT('Ctrl Pts',(7.67921999593717,-0.00642757427997835,
9.81423341595552));
#10843=CARTESIAN_POINT('Ctrl Pts',(7.67919901631219,-0.0132867957832829,
9.8146568350422));
#10844=CARTESIAN_POINT('Ctrl Pts',(7.67908726875781,-0.0311627145954824,
9.81575854209838));
#10845=CARTESIAN_POINT('Ctrl Pts',(7.67896190832854,-0.0421791588647937,
9.8164357403265));
#10846=CARTESIAN_POINT('Ctrl Pts',(7.6785598212312,-0.0665358320184445,
9.81792919613046));
#10847=CARTESIAN_POINT('Ctrl Pts',(7.67825673277487,-0.0798754686210316,
9.81874461760427));
#10848=CARTESIAN_POINT('Ctrl Pts',(7.67724587273198,-0.114810363339683,
9.82087374072973));
#10849=CARTESIAN_POINT('Ctrl Pts',(7.676403751909,-0.136401288975939,9.82218323111384));
#10850=CARTESIAN_POINT('Ctrl Pts',(7.67247659054794,-0.216416741788965,
9.8270140149127));
#10851=CARTESIAN_POINT('Ctrl Pts',(7.66801786859589,-0.274764496649009,
9.83049256274217));
#10852=CARTESIAN_POINT('Ctrl Pts',(7.65687582983732,-0.382031733374004,
9.83682556887203));
#10853=CARTESIAN_POINT('Ctrl Pts',(7.65065256122217,-0.430980066625157,
9.83969154504362));
#10854=CARTESIAN_POINT('Ctrl Pts',(7.60275977378607,-0.749105943252482,
9.85821572193964));
#10855=CARTESIAN_POINT('Ctrl Pts',(7.52823663255914,-1.01219235733315,9.87295000215523));
#10856=CARTESIAN_POINT('Ctrl Pts',(7.38643664285754,-1.34514943407498,9.89374760571939));
#10857=CARTESIAN_POINT('Ctrl Pts',(7.34793301146621,-1.42603302969453,9.89899372328385));
#10858=CARTESIAN_POINT('Ctrl Pts',(7.29833761037256,-1.51992708460718,9.90543784929495));
#10859=CARTESIAN_POINT('Ctrl Pts',(7.29044516328324,-1.53459265547766,9.90645494356437));
#10860=CARTESIAN_POINT('Ctrl Pts',(7.27803574020009,-1.55722934100019,9.90804233239676));
#10861=CARTESIAN_POINT('Ctrl Pts',(7.27359771370477,-1.56524371728423,9.90860776396864));
#10862=CARTESIAN_POINT('Ctrl Pts',(7.26529732416374,-1.58008325894628,9.90966130530712));
#10863=CARTESIAN_POINT('Ctrl Pts',(7.26144416700374,-1.5869133457858,9.91014883292004));
#10864=CARTESIAN_POINT('Ctrl Pts',(7.2525648634924,-1.60251937807423,9.91126876450845));
#10865=CARTESIAN_POINT('Ctrl Pts',(7.247522327569,-1.61128574437785,9.91190219956568));
#10866=CARTESIAN_POINT('Ctrl Pts',(7.23415518826596,-1.6342732739089,9.91357435620706));
#10867=CARTESIAN_POINT('Ctrl Pts',(7.22576274584919,-1.64845437162698,9.91461719224971));
#10868=CARTESIAN_POINT('Ctrl Pts',(7.16048343881514,-1.75685440318819,9.9226718941789));
#10869=CARTESIAN_POINT('Ctrl Pts',(7.09891775007986,-1.84815881476174,9.92994028631981));
#10870=CARTESIAN_POINT('Ctrl Pts',(6.88754774358668,-2.12942226747186,9.95351278466168));
#10871=CARTESIAN_POINT('Ctrl Pts',(6.72097057431804,-2.30578354131053,9.97007775942203));
#10872=CARTESIAN_POINT('Ctrl Pts',(6.45483559886048,-2.53061292137835,9.99292498399827));
#10873=CARTESIAN_POINT('Ctrl Pts',(6.37007609874208,-2.59530014581036,9.99977477048405));
#10874=CARTESIAN_POINT('Ctrl Pts',(6.2606443924544,-2.67053498375984,10.0081073214428));
#10875=CARTESIAN_POINT('Ctrl Pts',(6.23884891337553,-2.68513088160387,10.0097431269656));
#10876=CARTESIAN_POINT('Ctrl Pts',(6.20578566355649,-2.7066925358365,10.0121896787153));
#10877=CARTESIAN_POINT('Ctrl Pts',(6.19464958698807,-2.71385731496079,10.0130078399992));
#10878=CARTESIAN_POINT('Ctrl Pts',(6.17194538963449,-2.72826776365378,10.0146641699982));
#10879=CARTESIAN_POINT('Ctrl Pts',(6.16037475621262,-2.73550898630452,10.0155021622287));
#10880=CARTESIAN_POINT('Ctrl Pts',(6.13509826111924,-2.75110511622994,10.0173197094045));
#10881=CARTESIAN_POINT('Ctrl Pts',(6.12137523194765,-2.75943160945997,10.018298206435));
#10882=CARTESIAN_POINT('Ctrl Pts',(6.08333762719452,-2.78212399350229,10.020988083634));
#10883=CARTESIAN_POINT('Ctrl Pts',(6.05889519153959,-2.79627355914039,10.0226916144835));
#10884=CARTESIAN_POINT('Ctrl Pts',(5.92225013319539,-2.87299630020352,10.0320832132331));
#10885=CARTESIAN_POINT('Ctrl Pts',(5.80656326373418,-2.92914202500443,10.0395394944507));
#10886=CARTESIAN_POINT('Ctrl Pts',(5.48328746815852,-3.06280054959406,10.0594566277609));
#10887=CARTESIAN_POINT('Ctrl Pts',(5.27059749632247,-3.12606645338749,10.0715583081962));
#10888=CARTESIAN_POINT('Ctrl Pts',(4.98300132281416,-3.18024704468283,10.0882581043715));
#10889=CARTESIAN_POINT('Ctrl Pts',(4.91247621747375,-3.191122637554,10.0923832836022));
#10890=CARTESIAN_POINT('Ctrl Pts',(4.80011499180572,-3.20464904221776,10.0990828012916));
#10891=CARTESIAN_POINT('Ctrl Pts',(4.75848570554201,-3.20883991113459,10.1015924755917));
#10892=CARTESIAN_POINT('Ctrl Pts',(4.70367986426045,-3.21328140379905,10.1049463944504));
#10893=CARTESIAN_POINT('Ctrl Pts',(4.69056467201822,-3.21426349125607,10.1057527423508));
#10894=CARTESIAN_POINT('Ctrl Pts',(4.6690726628246,-3.21574061487841,10.1070807815817));
#10895=CARTESIAN_POINT('Ctrl Pts',(4.66069912534194,-3.21628326954639,10.1075998576704));
#10896=CARTESIAN_POINT('Ctrl Pts',(4.64432358831088,-3.21728029470964,10.1086183820768));
#10897=CARTESIAN_POINT('Ctrl Pts',(4.63632186690846,-3.21773752516636,10.1091176691765));
#10898=CARTESIAN_POINT('Ctrl Pts',(4.61845220994846,-3.21869176236602,10.1102361335892));
#10899=CARTESIAN_POINT('Ctrl Pts',(4.60858353533303,-3.21917324502341,10.1108561574953));
#10900=CARTESIAN_POINT('Ctrl Pts',(4.57448175627935,-3.22067987760433,10.1130064138393));
#10901=CARTESIAN_POINT('Ctrl Pts',(4.55024007181425,-3.22147680173744,10.1145484250521));
#10902=CARTESIAN_POINT('Ctrl Pts',(4.29616469113471,-3.22695917221954,10.1308352988315));
#10903=CARTESIAN_POINT('Ctrl Pts',(4.06648349227644,-3.20731360671786,10.1465799268687));
#10904=CARTESIAN_POINT('Ctrl Pts',(3.70099283993351,-3.13618846072786,10.1716873463901));
#10905=CARTESIAN_POINT('Ctrl Pts',(3.56306871174581,-3.09972026253991,10.1811864651691));
#10906=CARTESIAN_POINT('Ctrl Pts',(3.35180460885189,-3.02858017083324,10.1956401664037));
#10907=CARTESIAN_POINT('Ctrl Pts',(3.27659185432677,-3.00007883328078,10.2007681317039));
#10908=CARTESIAN_POINT('Ctrl Pts',(3.18042427302851,-2.95945981174252,10.2073051036386));
#10909=CARTESIAN_POINT('Ctrl Pts',(3.15843467449651,-2.94988126161821,10.2087985632167));
#10910=CARTESIAN_POINT('Ctrl Pts',(3.12272162497368,-2.93384817300427,10.2112224742302));
#10911=CARTESIAN_POINT('Ctrl Pts',(3.10893349353527,-2.92754081629147,10.212157908962));
#10912=CARTESIAN_POINT('Ctrl Pts',(3.08237725562864,-2.91516534221846,10.2139590087169));
#10913=CARTESIAN_POINT('Ctrl Pts',(3.06960358064444,-2.90911007188638,10.2148250901254));
#10914=CARTESIAN_POINT('Ctrl Pts',(3.04021798882582,-2.8949425001514,10.2168171160729));
#10915=CARTESIAN_POINT('Ctrl Pts',(3.02363510516452,-2.88677086970675,10.2179409746657));
#10916=CARTESIAN_POINT('Ctrl Pts',(2.97021676268909,-2.85987393827861,10.2215611171192));
#10917=CARTESIAN_POINT('Ctrl Pts',(2.93366996804725,-2.84058233292023,10.2240376089029));
#10918=CARTESIAN_POINT('Ctrl Pts',(2.69654880882918,-2.70952339772059,10.2401256202899));
#10919=CARTESIAN_POINT('Ctrl Pts',(2.50803521632308,-2.5772963129953,10.2529493327028));
#10920=CARTESIAN_POINT('Ctrl Pts',(2.22666211390671,-2.33127640734139,10.273849764921));
#10921=CARTESIAN_POINT('Ctrl Pts',(2.12465760471318,-2.22924605974608,10.281909257287));
#10922=CARTESIAN_POINT('Ctrl Pts',(2.00118547724504,-2.08796426713745,10.2928372009946));
#10923=CARTESIAN_POINT('Ctrl Pts',(1.9732083609513,-2.0546114457606,10.2954021874568));
#10924=CARTESIAN_POINT('Ctrl Pts',(1.92753504017212,-1.99786623534622,10.299761361581));
#10925=CARTESIAN_POINT('Ctrl Pts',(1.90946660175892,-1.97477976225421,10.301533596026));
#10926=CARTESIAN_POINT('Ctrl Pts',(1.88475906339256,-1.94230714134396,10.3040296423266));
#10927=CARTESIAN_POINT('Ctrl Pts',(1.87785085165892,-1.93312634445691,10.3047356939684));
#10928=CARTESIAN_POINT('Ctrl Pts',(1.86618998578101,-1.91745569565183,10.3059418280298));
#10929=CARTESIAN_POINT('Ctrl Pts',(1.86141218419524,-1.91098452024827,10.3064401824557));
#10930=CARTESIAN_POINT('Ctrl Pts',(1.8516383609433,-1.89764235847253,10.3074684035336));
#10931=CARTESIAN_POINT('Ctrl Pts',(1.84664523367791,-1.89076944194156,10.3079984452521));
#10932=CARTESIAN_POINT('Ctrl Pts',(1.83371533825434,-1.87282296342465,10.3093832873325));
#10933=CARTESIAN_POINT('Ctrl Pts',(1.82582160950704,-1.86171880592062,10.3102409320988));
#10934=CARTESIAN_POINT('Ctrl Pts',(1.7940193695222,-1.81637629599524,10.3137451130285));
#10935=CARTESIAN_POINT('Ctrl Pts',(1.77070812026272,-1.7817264079612,10.316427719854));
#10936=CARTESIAN_POINT('Ctrl Pts',(1.5683226537705,-1.46790074628903,10.3406982428882));
#10937=CARTESIAN_POINT('Ctrl Pts',(1.43265990537807,-1.1630787726175,10.3638322221651));
#10938=CARTESIAN_POINT('Ctrl Pts',(1.32938882984028,-0.781965047806497,
10.3896074013916));
#10939=CARTESIAN_POINT('Ctrl Pts',(1.31467511713148,-0.720577389254914,
10.3936779065262));
#10940=CARTESIAN_POINT('Ctrl Pts',(1.29251065704203,-0.614440780181416,
10.4005758452427));
#10941=CARTESIAN_POINT('Ctrl Pts',(1.28418447367038,-0.569895679828085,
10.403429321022));
#10942=CARTESIAN_POINT('Ctrl Pts',(1.27364143085589,-0.506064457583524,
10.4074610393373));
#10943=CARTESIAN_POINT('Ctrl Pts',(1.27065532822734,-0.48691256357353,10.4086634290249));
#10944=CARTESIAN_POINT('Ctrl Pts',(1.2657769651137,-0.453655922467149,10.4107390351009));
#10945=CARTESIAN_POINT('Ctrl Pts',(1.26380503151451,-0.439563592348429,
10.4116147447373));
#10946=CARTESIAN_POINT('Ctrl Pts',(1.25995249102548,-0.410636904172278,
10.4134046293212));
#10947=CARTESIAN_POINT('Ctrl Pts',(1.25808165901963,-0.395801576177258,
10.4143184761931));
#10948=CARTESIAN_POINT('Ctrl Pts',(1.25359350737592,-0.358099393691755,
10.4166307673093));
#10949=CARTESIAN_POINT('Ctrl Pts',(1.25111774396813,-0.335216294423932,
10.4180247409525));
#10950=CARTESIAN_POINT('Ctrl Pts',(1.24256620056765,-0.24738709997588,10.4233407297769));
#10951=CARTESIAN_POINT('Ctrl Pts',(1.23821726657937,-0.182286117020922,
10.4272088475887));
#10952=CARTESIAN_POINT('Ctrl Pts',(1.22368624262764,0.217382098415956,10.4506066745609));
#10953=CARTESIAN_POINT('Ctrl Pts',(1.26370030415009,0.551659280171078,10.4684365865389));
#10954=CARTESIAN_POINT('Ctrl Pts',(1.36711407729092,0.918799311953891,10.4905867484897));
#10955=CARTESIAN_POINT('Ctrl Pts',(1.38077800369832,0.963550974159175,10.4933367455716));
#10956=CARTESIAN_POINT('Ctrl Pts',(1.40508433819549,1.03736453542189,10.4979802944308));
#10957=CARTESIAN_POINT('Ctrl Pts',(1.41518016259921,1.06660001078157,10.499848021295));
#10958=CARTESIAN_POINT('Ctrl Pts',(1.42968405265914,1.10671924354929,10.5024564802682));
#10959=CARTESIAN_POINT('Ctrl Pts',(1.43373352358236,1.11773200368874,10.5031772686164));
#10960=CARTESIAN_POINT('Ctrl Pts',(1.44067665639394,1.13630054256862,10.5044010425109));
#10961=CARTESIAN_POINT('Ctrl Pts',(1.44353884711287,1.14386811978149,10.5049021756046));
#10962=CARTESIAN_POINT('Ctrl Pts',(1.44907402817738,1.15833811758942,10.5058651097169));
#10963=CARTESIAN_POINT('Ctrl Pts',(1.4517423455711,1.16524222431301,10.5063266125128));
#10964=CARTESIAN_POINT('Ctrl Pts',(1.4581880719486,1.18175078468853,10.5074349439068));
#10965=CARTESIAN_POINT('Ctrl Pts',(1.46198785217983,1.19134633502655,10.5080830788828));
#10966=CARTESIAN_POINT('Ctrl Pts',(1.47587014289994,1.22591712827557,10.5104319241996));
#10967=CARTESIAN_POINT('Ctrl Pts',(1.48621924417486,1.25078320764716,10.5121473876807));
#10968=CARTESIAN_POINT('Ctrl Pts',(1.56381781853494,1.43083588934329,10.5247438745543));
#10969=CARTESIAN_POINT('Ctrl Pts',(1.64287407995897,1.58063122515684,10.5361627636886));
#10970=CARTESIAN_POINT('Ctrl Pts',(1.81627938863639,1.85461212870683,10.5580975998598));
#10971=CARTESIAN_POINT('Ctrl Pts',(1.90861543588989,1.97955458261038,10.5685822459964));
#10972=CARTESIAN_POINT('Ctrl Pts',(2.0868038257101,2.18743624665154,10.5866209795249));
#10973=CARTESIAN_POINT('Ctrl Pts',(2.16892996767276,2.2731830674006,10.5942735960116));
#10974=CARTESIAN_POINT('Ctrl Pts',(2.27536116286318,2.37268138476804,10.6034218195368));
#10975=CARTESIAN_POINT('Ctrl Pts',(2.29534717572278,2.39089959792077,10.6051091371891));
#10976=CARTESIAN_POINT('Ctrl Pts',(2.32739302150087,2.41938074386109,10.6077673511515));
#10977=CARTESIAN_POINT('Ctrl Pts',(2.33930290370203,2.42980975458787,10.6087451846409));
#10978=CARTESIAN_POINT('Ctrl Pts',(2.36186908260158,2.4492781681474,10.6105792507942));
#10979=CARTESIAN_POINT('Ctrl Pts',(2.37250822472243,2.45833680727787,10.6114362674547));
#10980=CARTESIAN_POINT('Ctrl Pts',(2.39661382577828,2.47859244021172,10.6133610393574));
#10981=CARTESIAN_POINT('Ctrl Pts',(2.41011338371064,2.4897494927842,10.6144271512094));
#10982=CARTESIAN_POINT('Ctrl Pts',(2.4449724021288,2.5180845559845,10.6171505655273));
#10983=CARTESIAN_POINT('Ctrl Pts',(2.46646153845565,2.53510133360284,10.618801412554));
#10984=CARTESIAN_POINT('Ctrl Pts',(2.6552370322235,2.68070886380681,10.6330702431419));
#10985=CARTESIAN_POINT('Ctrl Pts',(2.83456647656753,2.79286318612986,10.6450045564167));
#10986=CARTESIAN_POINT('Ctrl Pts',(3.16975301107138,2.95924060008267,10.6659519200789));
#10987=CARTESIAN_POINT('Ctrl Pts',(3.32120117800465,3.02057999299012,10.6749977637266));
#10988=CARTESIAN_POINT('Ctrl Pts',(3.55305490134623,3.09457521741472,10.6890504051162));
#10989=CARTESIAN_POINT('Ctrl Pts',(3.63035588064386,3.11610135738314,10.6937701190569));
#10990=CARTESIAN_POINT('Ctrl Pts',(3.72411846779949,3.13847768454784,10.6996236759485));
#10991=CARTESIAN_POINT('Ctrl Pts',(3.73989260995214,3.14211676007866,10.7006127815641));
#10992=CARTESIAN_POINT('Ctrl Pts',(3.76453680844162,3.14760692434643,10.7021657742993));
#10993=CARTESIAN_POINT('Ctrl Pts',(3.77338863919336,3.14953976411872,10.702725129671));
#10994=CARTESIAN_POINT('Ctrl Pts',(3.7899311600375,3.15307888509004,10.7037735455463));
#10995=CARTESIAN_POINT('Ctrl Pts',(3.7976196769649,3.15469439313929,10.7042620778659));
#10996=CARTESIAN_POINT('Ctrl Pts',(3.81519923631034,3.15832113531748,10.7053819157759));
#10997=CARTESIAN_POINT('Ctrl Pts',(3.82509386346105,3.16031402493828,10.7060142375981));
#10998=CARTESIAN_POINT('Ctrl Pts',(3.85146027829207,3.16549575428454,10.7077042805933));
#10999=CARTESIAN_POINT('Ctrl Pts',(3.86794763690857,3.16860245291813,10.7087663620851));
#11000=CARTESIAN_POINT('Ctrl Pts',(4.01074615382345,3.1943569096528,10.7180062658649));
#11001=CARTESIAN_POINT('Ctrl Pts',(4.13826869446855,3.20956792258219,10.7265314288199));
#11002=CARTESIAN_POINT('Ctrl Pts',(4.45383763827683,3.22821744047018,10.7477988839086));
#11003=CARTESIAN_POINT('Ctrl Pts',(4.64195671198449,3.22288641439608,10.760605635627));
#11004=CARTESIAN_POINT('Ctrl Pts',(4.96576025145441,3.18525083861677,10.7822263357789));
#11005=CARTESIAN_POINT('Ctrl Pts',(5.10182333892039,3.16049475702027,10.7911851989636));
#11006=CARTESIAN_POINT('Ctrl Pts',(5.26317893870952,3.12027683551355,10.8016360746681));
#11007=CARTESIAN_POINT('Ctrl Pts',(5.29037441969082,3.11311906177195,10.80339183629));
#11008=CARTESIAN_POINT('Ctrl Pts',(5.33295382927633,3.1013142624892,10.8061325678051));
#11009=CARTESIAN_POINT('Ctrl Pts',(5.34840212674062,3.09690670287466,10.8071252251882));
#11010=CARTESIAN_POINT('Ctrl Pts',(5.37720007871632,3.08845698751825,10.8089726954126));
#11011=CARTESIAN_POINT('Ctrl Pts',(5.39055763936269,3.08444333865793,10.8098284111002));
#11012=CARTESIAN_POINT('Ctrl Pts',(5.42031027146503,3.07529233441839,10.8117319214297));
#11013=CARTESIAN_POINT('Ctrl Pts',(5.4366912417463,3.07011031019614,10.8127782299731));
#11014=CARTESIAN_POINT('Ctrl Pts',(5.47805735152002,3.05665954948261,10.8154165561771));
#11015=CARTESIAN_POINT('Ctrl Pts',(5.50298437994152,3.04821521355538,10.8170027980389));
#11016=CARTESIAN_POINT('Ctrl Pts',(5.65967679363376,2.99298501599292,10.8269561947725));
#11017=CARTESIAN_POINT('Ctrl Pts',(5.78839166253631,2.93796819542145,10.8350434064736));
#11018=CARTESIAN_POINT('Ctrl Pts',(6.10210698842642,2.77900544136473,10.8549977946015));
#11019=CARTESIAN_POINT('Ctrl Pts',(6.28116384389513,2.66485979021775,10.8665992928978));
#11020=CARTESIAN_POINT('Ctrl Pts',(6.50244831379754,2.490969994231,10.8826750217225));
#11021=CARTESIAN_POINT('Ctrl Pts',(6.55576630958784,2.44620368932329,10.8867038676878));
#11022=CARTESIAN_POINT('Ctrl Pts',(6.6382163040163,2.37229601826381,10.8932622917179));
#11023=CARTESIAN_POINT('Ctrl Pts',(6.66831281717414,2.34426028257049,10.8957304974198));
#11024=CARTESIAN_POINT('Ctrl Pts',(6.70725468058114,2.30656729856088,10.8990367075264));
#11025=CARTESIAN_POINT('Ctrl Pts',(6.71659082533019,2.29741990194421,10.8998381484173));
#11026=CARTESIAN_POINT('Ctrl Pts',(6.73181610960179,2.28231980434057,10.9011601640503));
#11027=CARTESIAN_POINT('Ctrl Pts',(6.73773825444993,2.27640039199073,10.9016781693041));
#11028=CARTESIAN_POINT('Ctrl Pts',(6.74929243240172,2.26476117804141,10.90269640893));
#11029=CARTESIAN_POINT('Ctrl Pts',(6.75492626945211,2.25904330696814,10.9031964947027));
#11030=CARTESIAN_POINT('Ctrl Pts',(6.76747929628213,2.2462074716817,10.9043186979078));
#11031=CARTESIAN_POINT('Ctrl Pts',(6.77438706980177,2.23907847393418,10.904941679839));
#11032=CARTESIAN_POINT('Ctrl Pts',(6.79824397242794,2.21422883537781,10.9071118543875));
#11033=CARTESIAN_POINT('Ctrl Pts',(6.81502322782553,2.19634724732291,10.9086711067592));
#11034=CARTESIAN_POINT('Ctrl Pts',(6.98524201374017,2.01074581529305,10.9248149443672));
#11035=CARTESIAN_POINT('Ctrl Pts',(7.12071984219153,1.82744233583162,10.9403755491017));
#11036=CARTESIAN_POINT('Ctrl Pts',(7.30868240230257,1.50722842270428,10.9654195617516));
#11037=CARTESIAN_POINT('Ctrl Pts',(7.37318573569044,1.37827066358377,10.9750248647329));
#11038=CARTESIAN_POINT('Ctrl Pts',(7.46012656534164,1.17077304174138,10.9896155046163));
#11039=CARTESIAN_POINT('Ctrl Pts',(7.48858171600869,1.09497152340598,10.9947784050595));
#11040=CARTESIAN_POINT('Ctrl Pts',(7.5217490012014,0.995366539106615,11.0013525290928));
#11041=CARTESIAN_POINT('Ctrl Pts',(7.52908811512436,0.9724751195583,11.0028494023457));
#11042=CARTESIAN_POINT('Ctrl Pts',(7.54064112010471,0.935003096531051,11.0052774403068));
#11043=CARTESIAN_POINT('Ctrl Pts',(7.54500925306155,0.920471387748938,11.0062136205683));
#11044=CARTESIAN_POINT('Ctrl Pts',(7.55324697706468,0.892347510280575,11.0080152048919));
#11045=CARTESIAN_POINT('Ctrl Pts',(7.55713010892174,0.878759703684791,11.0088810323424));
#11046=CARTESIAN_POINT('Ctrl Pts',(7.5658789399078,0.847365777339032,11.0108711256351));
#11047=CARTESIAN_POINT('Ctrl Pts',(7.57068131558189,0.829542410891683,11.0119933187065));
#11048=CARTESIAN_POINT('Ctrl Pts',(7.58569773872903,0.771842050558184,11.0156023696786));
#11049=CARTESIAN_POINT('Ctrl Pts',(7.59530125369099,0.731809378708541,11.0180696082588));
#11050=CARTESIAN_POINT('Ctrl Pts',(7.65404280643009,0.464460910628713,11.0343253648084));
#11051=CARTESIAN_POINT('Ctrl Pts',(7.67921910621825,0.232584571269279,11.0473022341681));
#11052=CARTESIAN_POINT('Ctrl Pts',(7.67921910621823,4.13155620826444E-12,
11.0603093566956));
#11053=CARTESIAN_POINT('Ctrl Pts',(7.67921909637197,0.000251920834644204,
10.8112112888099));
#11054=CARTESIAN_POINT('Ctrl Pts',(7.67921814033762,0.0124821902146477,
10.8104698495681));
#11055=CARTESIAN_POINT('Ctrl Pts',(7.67914756388822,0.0247125160183424,
10.8097305531979));
#11056=CARTESIAN_POINT('Ctrl Pts',(7.67874967167465,0.05942130752487,10.8076383569203));
#11057=CARTESIAN_POINT('Ctrl Pts',(7.67825677579211,0.0818974009304786,
10.8062905276175));
#11058=CARTESIAN_POINT('Ctrl Pts',(7.6747247277413,0.190906431148489,10.7997849037513));
#11059=CARTESIAN_POINT('Ctrl Pts',(7.66843420242991,0.277302262702642,10.7947260112625));
#11060=CARTESIAN_POINT('Ctrl Pts',(7.62986819249719,0.617188526220949,10.7750449003715));
#11061=CARTESIAN_POINT('Ctrl Pts',(7.57098767328278,0.866688250696628,10.7611596897908));
#11062=CARTESIAN_POINT('Ctrl Pts',(7.45931330519997,1.17214008832426,10.7425842695347));
#11063=CARTESIAN_POINT('Ctrl Pts',(7.43323512768143,1.23687045567647,10.7385461720994));
#11064=CARTESIAN_POINT('Ctrl Pts',(7.39389310644517,1.32605652627423,10.7327727756238));
#11065=CARTESIAN_POINT('Ctrl Pts',(7.38238121883419,1.3512675056706,10.7311167162734));
#11066=CARTESIAN_POINT('Ctrl Pts',(7.36167457304223,1.39510941406132,10.7281892017881));
#11067=CARTESIAN_POINT('Ctrl Pts',(7.3526219812279,1.41380605279516,10.7269253570229));
#11068=CARTESIAN_POINT('Ctrl Pts',(7.33894236877195,1.44137627471139,10.7250368680531));
#11069=CARTESIAN_POINT('Ctrl Pts',(7.33445353760921,1.45031833783466,10.7244204555405));
#11070=CARTESIAN_POINT('Ctrl Pts',(7.32637654746597,1.46622310537438,10.7233168422859));
#11071=CARTESIAN_POINT('Ctrl Pts',(7.32280455776994,1.47319380707129,10.72283064942));
#11072=CARTESIAN_POINT('Ctrl Pts',(7.31496459643249,1.48835695411372,10.7217675243059));
#11073=CARTESIAN_POINT('Ctrl Pts',(7.31068686693818,1.49654397189629,10.7211900043192));
#11074=CARTESIAN_POINT('Ctrl Pts',(7.29864963385638,1.51934232925502,10.7195722134272));
#11075=CARTESIAN_POINT('Ctrl Pts',(7.29081285459532,1.53391223808719,10.7185272929));
#11076=CARTESIAN_POINT('Ctrl Pts',(7.2459301501307,1.61583846034783,10.712591966948));
#11077=CARTESIAN_POINT('Ctrl Pts',(7.20659856426446,1.68190748079574,10.7075763979895));
#11078=CARTESIAN_POINT('Ctrl Pts',(7.15186361424725,1.76679054405747,10.7008858081471));
#11079=CARTESIAN_POINT('Ctrl Pts',(7.13855323434307,1.78693174696692,10.6992792594526));
#11080=CARTESIAN_POINT('Ctrl Pts',(7.07294695370399,1.88382229143512,10.6914643690124));
#11081=CARTESIAN_POINT('Ctrl Pts',(7.01757736195909,1.95843467110588,10.6851817318563));
#11082=CARTESIAN_POINT('Ctrl Pts',(6.84713068572379,2.16850543159649,10.6668799908397));
#11083=CARTESIAN_POINT('Ctrl Pts',(6.72396974789081,2.29698320623937,10.654909168971));
#11084=CARTESIAN_POINT('Ctrl Pts',(6.54539046221419,2.45483277018436,10.6393763213304));
#11085=CARTESIAN_POINT('Ctrl Pts',(6.49881868663857,2.49371315790049,10.6354694954964));
#11086=CARTESIAN_POINT('Ctrl Pts',(6.41664802486475,2.55846605256933,10.6288195190014));
#11087=CARTESIAN_POINT('Ctrl Pts',(6.38156696101045,2.58496585879209,10.6260527403455));
#11088=CARTESIAN_POINT('Ctrl Pts',(6.33100225439664,2.62156130129316,10.6221640571411));
#11089=CARTESIAN_POINT('Ctrl Pts',(6.3159583241122,2.63225341700168,10.6210192249988));
#11090=CARTESIAN_POINT('Ctrl Pts',(6.3004210598223,2.64309647869332,10.6198490599527));
#11091=CARTESIAN_POINT('Ctrl Pts',(6.30001893583932,2.64337697436172,10.6198187829466));
#11092=CARTESIAN_POINT('Ctrl Pts',(6.29921621884924,2.64393662552497,10.6197583608425));
#11093=CARTESIAN_POINT('Ctrl Pts',(6.29881562638652,2.64421578176337,10.6197282157169));
#11094=CARTESIAN_POINT('Ctrl Pts',(6.29801409780326,2.64477406315331,10.6196679161316));
#11095=CARTESIAN_POINT('Ctrl Pts',(6.29761316162423,2.64505318819942,10.6196377616764));
#11096=CARTESIAN_POINT('Ctrl Pts',(6.29680893663143,2.64561280470362,10.6195772923983));
#11097=CARTESIAN_POINT('Ctrl Pts',(6.29640564711696,2.64589329514308,10.6195469776147));
#11098=CARTESIAN_POINT('Ctrl Pts',(6.29559451797871,2.64645716552412,10.619486022813));
#11099=CARTESIAN_POINT('Ctrl Pts',(6.29518667695265,2.64674054342506,10.6194553828736));
#11100=CARTESIAN_POINT('Ctrl Pts',(6.29436398932019,2.64731188494822,10.6193935938853));
#11101=CARTESIAN_POINT('Ctrl Pts',(6.29394914049116,2.64759984536359,10.6193624449592));
#11102=CARTESIAN_POINT('Ctrl Pts',(6.29310963216011,2.64818228376005,10.6192994283009));
#11103=CARTESIAN_POINT('Ctrl Pts',(6.29268496947562,2.64847675713325,10.6192675607453));
#11104=CARTESIAN_POINT('Ctrl Pts',(6.29182255474529,2.64907447329488,10.6192028621032));
#11105=CARTESIAN_POINT('Ctrl Pts',(6.29138479830942,2.64937770976522,10.6191700312577));
#11106=CARTESIAN_POINT('Ctrl Pts',(6.29049227124517,2.6499956412216,10.6191031134801));
#11107=CARTESIAN_POINT('Ctrl Pts',(6.29003749471579,2.65031032768843,10.6190690268734));
#11108=CARTESIAN_POINT('Ctrl Pts',(6.28910610913606,2.65095445334739,10.6189992388471));
#11109=CARTESIAN_POINT('Ctrl Pts',(6.28862949218443,2.65128388111927,10.6189635378638));
#11110=CARTESIAN_POINT('Ctrl Pts',(6.28764834724949,2.65196163727851,10.618890069017));
#11111=CARTESIAN_POINT('Ctrl Pts',(6.28714380862485,2.65230995027918,10.6188523017408));
#11112=CARTESIAN_POINT('Ctrl Pts',(6.28639154319504,2.65282896690625,10.6187960101368));
#11113=CARTESIAN_POINT('Ctrl Pts',(6.28614389203217,2.65299977971444,10.6187774816517));
#11114=CARTESIAN_POINT('Ctrl Pts',(6.28553908936986,2.65341680619762,10.6187322398095));
#11115=CARTESIAN_POINT('Ctrl Pts',(6.28518191199602,2.65366298249474,10.6187055278757));
#11116=CARTESIAN_POINT('Ctrl Pts',(6.28427900984817,2.65428501818811,10.6186380196138));
#11117=CARTESIAN_POINT('Ctrl Pts',(6.28373321865466,2.65466078152906,10.6185972269422));
#11118=CARTESIAN_POINT('Ctrl Pts',(6.27258911918289,2.66232814517143,10.6177646198765));
#11119=CARTESIAN_POINT('Ctrl Pts',(6.26194724265096,2.66955647262255,10.6169752174111));
#11120=CARTESIAN_POINT('Ctrl Pts',(6.23771557691386,2.68580427280003,10.6151904192664));
#11121=CARTESIAN_POINT('Ctrl Pts',(6.22409995852453,2.69478473470162,10.6141965039965));
#11122=CARTESIAN_POINT('Ctrl Pts',(6.18576175291082,2.71965589403468,10.6114223956736));
#11123=CARTESIAN_POINT('Ctrl Pts',(6.16088873968896,2.73531260354452,10.609650886681));
#11124=CARTESIAN_POINT('Ctrl Pts',(5.99836490752757,2.83453797257349,10.5982500087928));
#11125=CARTESIAN_POINT('Ctrl Pts',(5.85482130878241,2.90803520114457,10.5889977944774));
#11126=CARTESIAN_POINT('Ctrl Pts',(5.50831813749511,3.05383360086019,10.5677875342344));
#11127=CARTESIAN_POINT('Ctrl Pts',(5.30244567930492,3.11714577108419,10.5560234979026));
#11128=CARTESIAN_POINT('Ctrl Pts',(5.01401086948633,3.17514787783862,10.5390279416438));
#11129=CARTESIAN_POINT('Ctrl Pts',(4.93565558614299,3.18791389076883,10.5343565614428));
#11130=CARTESIAN_POINT('Ctrl Pts',(4.84090049949899,3.19977977300703,10.5285573114725));
#11131=CARTESIAN_POINT('Ctrl Pts',(4.82487020626356,3.20166498818244,10.5275710720516));
#11132=CARTESIAN_POINT('Ctrl Pts',(4.79983154874142,3.20441908764935,10.5260216412684));
#11133=CARTESIAN_POINT('Ctrl Pts',(4.79083228635154,3.20537060498631,10.5254629485834));
#11134=CARTESIAN_POINT('Ctrl Pts',(4.77401200642193,3.20707745585063,10.5244151424474));
#11135=CARTESIAN_POINT('Ctrl Pts',(4.766192129019,3.20784210110908,10.5239265516702));
#11136=CARTESIAN_POINT('Ctrl Pts',(4.74830667786557,3.20952497307624,10.5228057732859));
#11137=CARTESIAN_POINT('Ctrl Pts',(4.73823953463086,3.21042444860722,10.5221725623958));
#11138=CARTESIAN_POINT('Ctrl Pts',(4.71140101003878,3.21269519995637,10.5204784630471));
#11139=CARTESIAN_POINT('Ctrl Pts',(4.69462308961619,3.21398247904009,10.5194131815238));
#11140=CARTESIAN_POINT('Ctrl Pts',(4.51530761655103,3.22632862276993,10.5079668885814));
#11141=CARTESIAN_POINT('Ctrl Pts',(4.35218195265447,3.22517760792805,10.4970302945412));
#11142=CARTESIAN_POINT('Ctrl Pts',(4.0864083979378,3.20311556665918,10.4790062374092));
#11143=CARTESIAN_POINT('Ctrl Pts',(3.98342645371507,3.18953378130472,10.4719685805042));
#11144=CARTESIAN_POINT('Ctrl Pts',(3.71625767697638,3.14107186327914,10.4537411317924));
#11145=CARTESIAN_POINT('Ctrl Pts',(3.55380623430455,3.09829949538152,10.4427021378335));
#11146=CARTESIAN_POINT('Ctrl Pts',(3.35737963528518,3.029808804846,10.429510996831));
#11147=CARTESIAN_POINT('Ctrl Pts',(3.31960746197088,3.01583900378104,10.4269807082249));
#11148=CARTESIAN_POINT('Ctrl Pts',(3.26488118156158,2.99442446693503,10.4233224703249));
#11149=CARTESIAN_POINT('Ctrl Pts',(3.24771482043455,2.98753623740773,10.4221760865794));
#11150=CARTESIAN_POINT('Ctrl Pts',(3.21757926070068,2.97514167545388,10.4201653077777));
#11151=CARTESIAN_POINT('Ctrl Pts',(3.20458521875577,2.96969742241077,10.4192988480017));
#11152=CARTESIAN_POINT('Ctrl Pts',(3.17756157993267,2.95816614888372,10.417497870999));
#11153=CARTESIAN_POINT('Ctrl Pts',(3.16353874408766,2.95206411117862,10.4165638898192));
#11154=CARTESIAN_POINT('Ctrl Pts',(3.12708407684098,2.93589127564845,10.414136999552));
#11155=CARTESIAN_POINT('Ctrl Pts',(3.10472286308955,2.92566305033427,10.412649497066));
#11156=CARTESIAN_POINT('Ctrl Pts',(3.01179839128535,2.88186569061529,10.4064702645387));
#11157=CARTESIAN_POINT('Ctrl Pts',(2.94234769378112,2.84599035929404,10.4018582890044));
#11158=CARTESIAN_POINT('Ctrl Pts',(2.59588690315103,2.65074639365128,10.3787449578783));
#11159=CARTESIAN_POINT('Ctrl Pts',(2.34242583966154,2.45336666498699,10.3616719260676));
#11160=CARTESIAN_POINT('Ctrl Pts',(2.09033280157612,2.18852618607789,10.3404268506277));
#11161=CARTESIAN_POINT('Ctrl Pts',(2.05923392549234,2.15441661484041,10.3377127261952));
#11162=CARTESIAN_POINT('Ctrl Pts',(2.00874133273874,2.09658861521045,10.3331241908187));
#11163=CARTESIAN_POINT('Ctrl Pts',(1.98893340906712,2.0732396151966,10.3312748298298));
#11164=CARTESIAN_POINT('Ctrl Pts',(1.96202936855526,2.04059416341122,10.3286880015695));
#11165=CARTESIAN_POINT('Ctrl Pts',(1.95464599152431,2.03153519230877,10.3279700488556));
#11166=CARTESIAN_POINT('Ctrl Pts',(1.94224097508167,2.01614477879654,10.3267497198601));
#11167=CARTESIAN_POINT('Ctrl Pts',(1.9371934901261,2.00983413070289,10.3262491721954));
#11168=CARTESIAN_POINT('Ctrl Pts',(1.92756264946095,1.99769983150096,10.3252862466478));
#11169=CARTESIAN_POINT('Ctrl Pts',(1.9229755713762,1.9918792609238,10.3248241599439));
#11170=CARTESIAN_POINT('Ctrl Pts',(1.91076251116181,1.97627160029268,10.3235846988326));
#11171=CARTESIAN_POINT('Ctrl Pts',(1.90317299506083,1.96645632120958,10.32280482275));
#11172=CARTESIAN_POINT('Ctrl Pts',(1.87561072898966,1.93038235394059,10.3199378212155));
#11173=CARTESIAN_POINT('Ctrl Pts',(1.85598558581657,1.90386219547677,10.3178287155303));
#11174=CARTESIAN_POINT('Ctrl Pts',(1.63663296470507,1.59772306212793,10.2935094510462));
#11175=CARTESIAN_POINT('Ctrl Pts',(1.48244106606708,1.2881802135927,10.2694733897782));
#11176=CARTESIAN_POINT('Ctrl Pts',(1.36134590021225,0.900150710269656,10.2429449133735));
#11177=CARTESIAN_POINT('Ctrl Pts',(1.34439737374029,0.839684067797136,10.2388963574241));
#11178=CARTESIAN_POINT('Ctrl Pts',(1.3183200539857,0.734965798778296,10.2320316385589));
#11179=CARTESIAN_POINT('Ctrl Pts',(1.30833551111386,0.690948187732318,10.2291897629372));
#11180=CARTESIAN_POINT('Ctrl Pts',(1.29539510715096,0.627776383626155,10.2251714349104));
#11181=CARTESIAN_POINT('Ctrl Pts',(1.29168259212148,0.608784331105901,10.2239710521369));
#11182=CARTESIAN_POINT('Ctrl Pts',(1.28553856506472,0.575777170220123,10.2218978642694));
#11183=CARTESIAN_POINT('Ctrl Pts',(1.28302839148411,0.561777435419149,10.2210225810147));
#11184=CARTESIAN_POINT('Ctrl Pts',(1.27806812888478,0.533018396231397,10.2192326349437));
#11185=CARTESIAN_POINT('Ctrl Pts',(1.27562796928626,0.518257712809005,10.2183183065131));
#11186=CARTESIAN_POINT('Ctrl Pts',(1.26968823921314,0.480704668525556,10.2160029323459));
#11187=CARTESIAN_POINT('Ctrl Pts',(1.26633030225269,0.457890517943861,10.2146063825791));
#11188=CARTESIAN_POINT('Ctrl Pts',(1.25436641683359,0.370074371341196,10.2092675608518));
#11189=CARTESIAN_POINT('Ctrl Pts',(1.24749969664378,0.30484895048233,10.2053798019695));
#11190=CARTESIAN_POINT('Ctrl Pts',(1.21778888700268,-0.0939127560540211,
10.1819900242355));
#11191=CARTESIAN_POINT('Ctrl Pts',(1.24496884967253,-0.429064027471083,
10.1641803265554));
#11192=CARTESIAN_POINT('Ctrl Pts',(1.33411196502905,-0.79949422194072,10.1420542915426));
#11193=CARTESIAN_POINT('Ctrl Pts',(1.34604308381342,-0.844721643567564,
10.1393052262906));
#11194=CARTESIAN_POINT('Ctrl Pts',(1.36748942152943,-0.919390096834596,
10.1346631432224));
#11195=CARTESIAN_POINT('Ctrl Pts',(1.37645224355946,-0.948983460419278,
10.1327959310387));
#11196=CARTESIAN_POINT('Ctrl Pts',(1.3894008882927,-0.989619999092187,10.1301881236437));
#11197=CARTESIAN_POINT('Ctrl Pts',(1.39302364291881,-1.00077823693333,10.1294674605805));
#11198=CARTESIAN_POINT('Ctrl Pts',(1.39924728787083,-1.01959686149254,10.1282438770101));
#11199=CARTESIAN_POINT('Ctrl Pts',(1.40181629092783,-1.02726782428499,10.1277428081568));
#11200=CARTESIAN_POINT('Ctrl Pts',(1.40679088936271,-1.04193815240546,10.126779981652));
#11201=CARTESIAN_POINT('Ctrl Pts',(1.40919175336887,-1.04893902205962,10.1263185220534));
#11202=CARTESIAN_POINT('Ctrl Pts',(1.41499800258247,-1.06568174864628,10.1252102763244));
#11203=CARTESIAN_POINT('Ctrl Pts',(1.41842608299683,-1.07541556893228,10.1245621839069));
#11204=CARTESIAN_POINT('Ctrl Pts',(1.43096977249069,-1.11049393869981,10.1222133581154));
#11205=CARTESIAN_POINT('Ctrl Pts',(1.44035598487733,-1.13573964248514,10.1204978707118));
#11206=CARTESIAN_POINT('Ctrl Pts',(1.51071959095196,-1.31796773368111,10.1079477400085));
#11207=CARTESIAN_POINT('Ctrl Pts',(1.58359761346543,-1.47006048735957,10.0965797370211));
#11208=CARTESIAN_POINT('Ctrl Pts',(1.74224129658463,-1.74384753375148,10.0751739999166));
#11209=CARTESIAN_POINT('Ctrl Pts',(1.82521192110522,-1.8666890527819,10.0651652034073));
#11210=CARTESIAN_POINT('Ctrl Pts',(1.9936839627957,-2.08245067727558,10.0470845675642));
#11211=CARTESIAN_POINT('Ctrl Pts',(2.07676303259264,-2.17690542105144,10.0389618091173));
#11212=CARTESIAN_POINT('Ctrl Pts',(2.18446713668157,-2.28579934459972,10.0293415409776));
#11213=CARTESIAN_POINT('Ctrl Pts',(2.20402626460562,-2.30507546809343,10.0276276947414));
#11214=CARTESIAN_POINT('Ctrl Pts',(2.23531070988738,-2.33512877377327,10.0249375453656));
#11215=CARTESIAN_POINT('Ctrl Pts',(2.24687327493903,-2.34607273728276,10.02395401751));
#11216=CARTESIAN_POINT('Ctrl Pts',(2.26872602069147,-2.36645148495767,10.0221149956874));
#11217=CARTESIAN_POINT('Ctrl Pts',(2.27899728961242,-2.37590591912105,10.0212586709671));
#11218=CARTESIAN_POINT('Ctrl Pts',(2.30218987238983,-2.39697735508031,10.0193428629521));
#11219=CARTESIAN_POINT('Ctrl Pts',(2.31514441889843,-2.4085572569366,10.0182849584729));
#11220=CARTESIAN_POINT('Ctrl Pts',(2.34843585625655,-2.43783513332583,10.0155966868537));
#11221=CARTESIAN_POINT('Ctrl Pts',(2.36890256207908,-2.45538394359089,10.0139724912624));
#11222=CARTESIAN_POINT('Ctrl Pts',(2.51033051776054,-2.57360203504729,10.002935807968));
#11223=CARTESIAN_POINT('Ctrl Pts',(2.63831121799681,-2.66555691806683,9.99388391983638));
#11224=CARTESIAN_POINT('Ctrl Pts',(2.95844616478623,-2.86174768094455,9.97268152184718));
#11225=CARTESIAN_POINT('Ctrl Pts',(3.15544972984387,-2.95651972997849,9.96075153270206));
#11226=CARTESIAN_POINT('Ctrl Pts',(3.4356038586933,-3.05783099988023,9.94354676086417));
#11227=CARTESIAN_POINT('Ctrl Pts',(3.51168780436764,-3.08218791204095,9.93884711582047));
#11228=CARTESIAN_POINT('Ctrl Pts',(3.60416150136919,-3.10804612571095,9.93301614895125));
#11229=CARTESIAN_POINT('Ctrl Pts',(3.61976456362276,-3.11228283680847,9.93202827122564));
#11230=CARTESIAN_POINT('Ctrl Pts',(3.64415508636642,-3.11870894708472,9.93047682585878));
#11231=CARTESIAN_POINT('Ctrl Pts',(3.65292126267374,-3.12097908065923,9.92991777594184));
#11232=CARTESIAN_POINT('Ctrl Pts',(3.66931052833491,-3.12514970186349,9.92886967730495));
#11233=CARTESIAN_POINT('Ctrl Pts',(3.67693110204434,-3.1270592864645,9.92838115447137));
#11234=CARTESIAN_POINT('Ctrl Pts',(3.6943629147211,-3.13135971927985,9.92726101568716));
#11235=CARTESIAN_POINT('Ctrl Pts',(3.7041784525157,-3.13373232815647,9.92662838081642));
#11236=CARTESIAN_POINT('Ctrl Pts',(3.73034939864135,-3.13992831951293,9.92493683146913));
#11237=CARTESIAN_POINT('Ctrl Pts',(3.74672357642959,-3.14366997893885,9.92387354417107));
#11238=CARTESIAN_POINT('Ctrl Pts',(3.88973381179413,-3.17517498538392,9.9145482829503));
#11239=CARTESIAN_POINT('Ctrl Pts',(4.01789618243485,-3.19539847881571,9.90593192464381));
#11240=CARTESIAN_POINT('Ctrl Pts',(4.20200696691789,-3.21316515352719,9.89348491067499));
#11241=CARTESIAN_POINT('Ctrl Pts',(4.25722913526284,-3.21706148196895,9.88974209664869));
#11242=CARTESIAN_POINT('Ctrl Pts',(4.46567809834205,-3.22638124944188,9.87562605688196));
#11243=CARTESIAN_POINT('Ctrl Pts',(4.61913720846135,-3.2222921182501,9.86527056314726));
#11244=CARTESIAN_POINT('Ctrl Pts',(4.88910718369397,-3.19575533144132,9.84740292646025));
#11245=CARTESIAN_POINT('Ctrl Pts',(5.00577176481852,-3.1777822506138,9.83979623955946));
#11246=CARTESIAN_POINT('Ctrl Pts',(5.14761683986571,-3.1478820167745,9.83069447803535));
#11247=CARTESIAN_POINT('Ctrl Pts',(5.17396257660983,-3.14198179059991,9.82901001734078));
#11248=CARTESIAN_POINT('Ctrl Pts',(5.21562399011704,-3.13210020200933,9.82635531884745));
#11249=CARTESIAN_POINT('Ctrl Pts',(5.23098938148993,-3.12833600666929,9.82537817399062));
#11250=CARTESIAN_POINT('Ctrl Pts',(5.25987309208869,-3.12103425665755,9.82354482049152));
#11251=CARTESIAN_POINT('Ctrl Pts',(5.27339727944072,-3.11752163829869,9.82268783274062));
#11252=CARTESIAN_POINT('Ctrl Pts',(5.30383138618866,-3.10940538498125,9.82076236937654));
#11253=CARTESIAN_POINT('Ctrl Pts',(5.32072754507335,-3.10475152812595,9.81969554338449));
#11254=CARTESIAN_POINT('Ctrl Pts',(5.36399133190121,-3.09245446065972,9.81696884373966));
#11255=CARTESIAN_POINT('Ctrl Pts',(5.39030110771465,-3.08461165212121,9.81531545346186));
#11256=CARTESIAN_POINT('Ctrl Pts',(5.61135516975866,-3.01562900693202,9.80145647819413));
#11257=CARTESIAN_POINT('Ctrl Pts',(5.79999452932515,-2.93644933080625,9.78988621295467));
#11258=CARTESIAN_POINT('Ctrl Pts',(6.10843308791325,-2.77099414210449,9.77028060140354));
#11259=CARTESIAN_POINT('Ctrl Pts',(6.23213520906258,-2.69339934632674,9.7621900674558));
#11260=CARTESIAN_POINT('Ctrl Pts',(6.43313875130678,-2.54743271769388,9.74799760587075));
#11261=CARTESIAN_POINT('Ctrl Pts',(6.51319389706793,-2.48324688826594,9.74202403291668));
#11262=CARTESIAN_POINT('Ctrl Pts',(6.60292824027595,-2.40398133360863,9.73476318390896));
#11263=CARTESIAN_POINT('Ctrl Pts',(6.61572025541774,-2.3924981737591,9.73371393261964));
#11264=CARTESIAN_POINT('Ctrl Pts',(6.63527187361856,-2.37466252205988,9.73208711346476));
#11265=CARTESIAN_POINT('Ctrl Pts',(6.64209715994522,-2.36838206348538,9.73151480210709));
#11266=CARTESIAN_POINT('Ctrl Pts',(6.65463365558372,-2.35674595092397,9.73045523153041));
#11267=CARTESIAN_POINT('Ctrl Pts',(6.66035254629726,-2.35139886912497,9.72996861473297));
#11268=CARTESIAN_POINT('Ctrl Pts',(6.67329932843229,-2.33920508862119,9.7288595636404));
#11269=CARTESIAN_POINT('Ctrl Pts',(6.68051497488574,-2.33234573950822,9.7282361759791));
#11270=CARTESIAN_POINT('Ctrl Pts',(6.69921018379128,-2.31440803080173,9.72660750658177));
#11271=CARTESIAN_POINT('Ctrl Pts',(6.71063931635709,-2.30327781949418,9.72559843812134));
#11272=CARTESIAN_POINT('Ctrl Pts',(6.78924499074979,-2.22558258470347,9.71856795432336));
#11273=CARTESIAN_POINT('Ctrl Pts',(6.85353977601534,-2.15617946684834,9.7123563157888));
#11274=CARTESIAN_POINT('Ctrl Pts',(7.03215585607542,-1.94549592777755,9.69393610501191));
#11275=CARTESIAN_POINT('Ctrl Pts',(7.13770172312054,-1.79725061730207,9.68152466652997));
#11276=CARTESIAN_POINT('Ctrl Pts',(7.30562919662112,-1.51339125927077,9.65941997303687));
#11277=CARTESIAN_POINT('Ctrl Pts',(7.37218754747625,-1.38081940793283,9.64966903169383));
#11278=CARTESIAN_POINT('Ctrl Pts',(7.44806036171018,-1.19951553175262,9.63714186858402));
#11279=CARTESIAN_POINT('Ctrl Pts',(7.46572189929812,-1.15449286927154,9.63409274466785));
#11280=CARTESIAN_POINT('Ctrl Pts',(7.48920682767043,-1.09041955082206,9.62983758079859));
#11281=CARTESIAN_POINT('Ctrl Pts',(7.49587653577505,-1.07168810271846,9.62860358436104));
#11282=CARTESIAN_POINT('Ctrl Pts',(7.5070499315085,-1.03936478505215,9.62649095010929));
#11283=CARTESIAN_POINT('Ctrl Pts',(7.51163711669378,-1.02580259617763,9.62560957075305));
#11284=CARTESIAN_POINT('Ctrl Pts',(7.52023498376673,-0.999813337354608,
9.62393002501564));
#11285=CARTESIAN_POINT('Ctrl Pts',(7.52426080021341,-0.987391610319358,
9.62313137485021));
#11286=CARTESIAN_POINT('Ctrl Pts',(7.53352168066227,-0.958213536596063,
9.62126479486707));
#11287=CARTESIAN_POINT('Ctrl Pts',(7.53869558262355,-0.941438099178831,
9.62019888017037));
#11288=CARTESIAN_POINT('Ctrl Pts',(7.55606754108163,-0.883433999148986,
9.61653748320085));
#11289=CARTESIAN_POINT('Ctrl Pts',(7.56757781208675,-0.842002951441,9.61396427375406));
#11290=CARTESIAN_POINT('Ctrl Pts',(7.6452990315115,-0.538850156262905,9.59541229192057));
#11291=CARTESIAN_POINT('Ctrl Pts',(7.67921910621722,-0.269971659946486,
9.5805624267731));
#11292=CARTESIAN_POINT('Ctrl Pts',(7.67921910621823,-1.20008863957466E-11,
9.56539764702567));
#11293=CARTESIAN_POINT('Origin',(4.45646910621825,-5.13094777615093E-16,
-2.31077344927308));
#11294=CARTESIAN_POINT('',(7.67921910621823,-4.32305015001326E-11,8.31612808864258));
#11295=CARTESIAN_POINT('',(7.67921910621823,1.63241365473312E-10,8.56014415614755));
#11296=CARTESIAN_POINT('',(7.67921910621823,-3.51191647465084E-13,-2.31077344927308));
#11297=CARTESIAN_POINT('Ctrl Pts',(7.67921910621823,1.63240393424857E-10,
8.56014415614755));
#11298=CARTESIAN_POINT('Ctrl Pts',(7.67921910623171,-0.266045158755238,
8.57813436331319));
#11299=CARTESIAN_POINT('Ctrl Pts',(7.64627463525177,-0.531126215526067,
8.59606011624979));
#11300=CARTESIAN_POINT('Ctrl Pts',(7.5716381018007,-0.826639474292601,8.61536623206872));
#11301=CARTESIAN_POINT('Ctrl Pts',(7.56150248251137,-0.863932076104476,
8.61779245718516));
#11302=CARTESIAN_POINT('Ctrl Pts',(7.54566539375373,-0.918317973315446,
8.6213172267283));
#11303=CARTESIAN_POINT('Ctrl Pts',(7.54048773856555,-0.935559030440784,
8.62243262266453));
#11304=CARTESIAN_POINT('Ctrl Pts',(7.53100827512552,-0.966190577496588,
8.6244109927897));
#11305=CARTESIAN_POINT('Ctrl Pts',(7.52676279586725,-0.979597877930699,
8.62527577996548));
#11306=CARTESIAN_POINT('Ctrl Pts',(7.51768969288889,-1.00761239587881,8.62708054229396));
#11307=CARTESIAN_POINT('Ctrl Pts',(7.51284495431674,-1.02221372941467,8.6280199304207));
#11308=CARTESIAN_POINT('Ctrl Pts',(7.49985317450248,-1.06045083175874,8.63047695265231));
#11309=CARTESIAN_POINT('Ctrl Pts',(7.49153523983137,-1.0840277542396,8.63198892486271));
#11310=CARTESIAN_POINT('Ctrl Pts',(7.45161767680612,-1.19311021973424,8.63897322441953));
#11311=CARTESIAN_POINT('Ctrl Pts',(7.41667211718725,-1.27735168005217,8.64433354406527));
#11312=CARTESIAN_POINT('Ctrl Pts',(7.3038937192333,-1.51963623994239,8.65978228322838));
#11313=CARTESIAN_POINT('Ctrl Pts',(7.21662746243491,-1.6729171288756,8.66958276301207));
#11314=CARTESIAN_POINT('Ctrl Pts',(7.01585930898204,-1.966710152776,8.68949065761058));
#11315=CARTESIAN_POINT('Ctrl Pts',(6.90221772390692,-2.10635335977743,8.69957173040615));
#11316=CARTESIAN_POINT('Ctrl Pts',(6.75893556217045,-2.25510213429688,8.71195409070326));
#11317=CARTESIAN_POINT('Ctrl Pts',(6.7400823156765,-2.27419172897672,8.71357781679368));
#11318=CARTESIAN_POINT('Ctrl Pts',(6.71366048793978,-2.30028494967422,8.71584962443154));
#11319=CARTESIAN_POINT('Ctrl Pts',(6.70629275556051,-2.30749156522323,8.7164827228139));
#11320=CARTESIAN_POINT('Ctrl Pts',(6.69357717926225,-2.31981028624362,8.71757494768917));
#11321=CARTESIAN_POINT('Ctrl Pts',(6.68824601297749,-2.32493959717168,8.71803275561443));
#11322=CARTESIAN_POINT('Ctrl Pts',(6.67704507023155,-2.33564241038036,8.71899449308323));
#11323=CARTESIAN_POINT('Ctrl Pts',(6.67117191769319,-2.34121219305574,8.71949870999025));
#11324=CARTESIAN_POINT('Ctrl Pts',(6.65672075497676,-2.35481386525024,8.72073906554134));
#11325=CARTESIAN_POINT('Ctrl Pts',(6.64811972410858,-2.36282102938297,8.72147704588266));
#11326=CARTESIAN_POINT('Ctrl Pts',(6.61663497186748,-2.39181207183875,8.72417692219809));
#11327=CARTESIAN_POINT('Ctrl Pts',(6.59349292670909,-2.41251125982059,8.72615841403667));
#11328=CARTESIAN_POINT('Ctrl Pts',(6.53455200237349,-2.46371691097859,8.731189744691));
#11329=CARTESIAN_POINT('Ctrl Pts',(6.49837832581934,-2.49377942678379,8.73426371750534));
#11330=CARTESIAN_POINT('Ctrl Pts',(6.19452092419874,-2.73525903413027,8.75988661147945));
#11331=CARTESIAN_POINT('Ctrl Pts',(5.89546083249698,-2.90376578648535,8.78355480818503));
#11332=CARTESIAN_POINT('Ctrl Pts',(5.51924250453308,-3.04306168929238,8.80931334935854));
#11333=CARTESIAN_POINT('Ctrl Pts',(5.46244827320802,-3.06230606349106,8.8131132733979));
#11334=CARTESIAN_POINT('Ctrl Pts',(5.38385879787382,-3.08651293633397,8.81825402052648));
#11335=CARTESIAN_POINT('Ctrl Pts',(5.36250276052255,-3.09284930179538,8.81963930404839));
#11336=CARTESIAN_POINT('Ctrl Pts',(5.32827778284383,-3.10261897587398,8.82184116021949));
#11337=CARTESIAN_POINT('Ctrl Pts',(5.31545058028242,-3.10619473211106,8.82266234201427));
#11338=CARTESIAN_POINT('Ctrl Pts',(5.28895939846442,-3.11340285848696,8.82435007186715));
#11339=CARTESIAN_POINT('Ctrl Pts',(5.2752929224201,-3.11702502620548,8.8252162735536));
#11340=CARTESIAN_POINT('Ctrl Pts',(5.24337661972674,-3.12525973931445,8.82722897336991));
#11341=CARTESIAN_POINT('Ctrl Pts',(5.22510922013725,-3.12980259306518,8.82837320324312));
#11342=CARTESIAN_POINT('Ctrl Pts',(5.16588216344047,-3.14398173403054,8.83205887573175));
#11343=CARTESIAN_POINT('Ctrl Pts',(5.12477229891581,-3.15297623187847,8.83457979436019));
#11344=CARTESIAN_POINT('Ctrl Pts',(5.02730602995478,-3.1723089970325,8.84047720225616));
#11345=CARTESIAN_POINT('Ctrl Pts',(4.97082618173617,-3.18195482449718,8.84383247538456));
#11346=CARTESIAN_POINT('Ctrl Pts',(4.75526211998063,-3.21287946272154,8.85644815557179));
#11347=CARTESIAN_POINT('Ctrl Pts',(4.59491957481742,-3.22377230872117,8.86542812234982));
#11348=CARTESIAN_POINT('Ctrl Pts',(4.41377157453322,-3.22253334753993,8.87555690556549));
#11349=CARTESIAN_POINT('Ctrl Pts',(4.39311736902046,-3.22219347823403,8.87671176831728));
#11350=CARTESIAN_POINT('Ctrl Pts',(4.19243617140399,-3.21696092972169,8.8879425841779));
#11351=CARTESIAN_POINT('Ctrl Pts',(4.01313653340017,-3.19718484463236,8.89804109646337));
#11352=CARTESIAN_POINT('Ctrl Pts',(3.81001409448675,-3.15736271749901,8.91044946079441));
#11353=CARTESIAN_POINT('Ctrl Pts',(3.78364280649666,-3.15184835847806,8.91207981103353));
#11354=CARTESIAN_POINT('Ctrl Pts',(3.74726884938306,-3.14376511455478,8.9143593040352));
#11355=CARTESIAN_POINT('Ctrl Pts',(3.73720393170334,-3.141477630318,8.91499332768923));
#11356=CARTESIAN_POINT('Ctrl Pts',(3.71994022354113,-3.13746674233525,8.91608672482675));
#11357=CARTESIAN_POINT('Ctrl Pts',(3.71273598971319,-3.13576679666831,8.91654477332416));
#11358=CARTESIAN_POINT('Ctrl Pts',(3.69766982462866,-3.1321568720545,8.91750651295192));
#11359=CARTESIAN_POINT('Ctrl Pts',(3.68980917701839,-3.13024209427628,8.91801048838225));
#11360=CARTESIAN_POINT('Ctrl Pts',(3.67056734597002,-3.1254781452905,8.91924940380384));
#11361=CARTESIAN_POINT('Ctrl Pts',(3.65919441464672,-3.12259639877303,8.91998617595629));
#11362=CARTESIAN_POINT('Ctrl Pts',(3.61790648575937,-3.1118943366093,8.9226767041511));
#11363=CARTESIAN_POINT('Ctrl Pts',(3.58808975881175,-3.10370597441035,8.9246498837514));
#11364=CARTESIAN_POINT('Ctrl Pts',(3.51347975900388,-3.08205711406361,8.92965556461399));
#11365=CARTESIAN_POINT('Ctrl Pts',(3.46885399001639,-3.06804838649118,8.93271190720616));
#11366=CARTESIAN_POINT('Ctrl Pts',(3.10800130231633,-2.94608268908611,8.95785368948979));
#11367=CARTESIAN_POINT('Ctrl Pts',(2.80998669748263,-2.79050925012496,8.98103418809206));
#11368=CARTESIAN_POINT('Ctrl Pts',(2.48839113237206,-2.55285964489084,9.00678788267015));
#11369=CARTESIAN_POINT('Ctrl Pts',(2.43681922827416,-2.51225768061364,9.01095551410693));
#11370=CARTESIAN_POINT('Ctrl Pts',(2.36883995428409,-2.45529105660766,9.01650442373908));
#11371=CARTESIAN_POINT('Ctrl Pts',(2.35131926185671,-2.44028560334203,9.01793981938467));
#11372=CARTESIAN_POINT('Ctrl Pts',(2.32270089967534,-2.41523802340159,9.02029358053654));
#11373=CARTESIAN_POINT('Ctrl Pts',(2.31150961047107,-2.40530460494819,9.02121639215117));
#11374=CARTESIAN_POINT('Ctrl Pts',(2.289816110687,-2.38577758210017,9.02301002776923));
#11375=CARTESIAN_POINT('Ctrl Pts',(2.2793074448476,-2.37619169781858,9.02388114506244));
#11376=CARTESIAN_POINT('Ctrl Pts',(2.25465375755024,-2.35340203371604,9.02593039078003));
#11377=CARTESIAN_POINT('Ctrl Pts',(2.24056340722253,-2.34013972239799,9.02710599428367));
#11378=CARTESIAN_POINT('Ctrl Pts',(2.19402215410672,-2.29553623059744,9.03100478054321));
#11379=CARTESIAN_POINT('Ctrl Pts',(2.16210910024029,-2.26363982599952,9.03370390214333));
#11380=CARTESIAN_POINT('Ctrl Pts',(2.0874332191019,-2.18580058223674,9.04009329732077));
#11381=CARTESIAN_POINT('Ctrl Pts',(2.04532149239832,-2.13925760351277,9.04375703498692));
#11382=CARTESIAN_POINT('Ctrl Pts',(1.78201150245087,-1.83057989472059,9.06717307026251));
#11383=CARTESIAN_POINT('Ctrl Pts',(1.60255103113114,-1.53584644364613,9.08531402281039));
#11384=CARTESIAN_POINT('Ctrl Pts',(1.46022465917345,-1.18733527438123,9.10774119880578));
#11385=CARTESIAN_POINT('Ctrl Pts',(1.44801278370199,-1.15604333573595,9.10976486374217));
#11386=CARTESIAN_POINT('Ctrl Pts',(1.4319320302784,-1.11285632961836,9.1125788556098));
#11387=CARTESIAN_POINT('Ctrl Pts',(1.42763953135996,-1.10111994292676,9.11334569224518));
#11388=CARTESIAN_POINT('Ctrl Pts',(1.42090440914674,-1.08236764478966,9.11457474753833));
#11389=CARTESIAN_POINT('Ctrl Pts',(1.41841754785586,-1.07536759979857,9.11503438431459));
#11390=CARTESIAN_POINT('Ctrl Pts',(1.41328059857458,-1.06074801447655,9.11599621385248));
#11391=CARTESIAN_POINT('Ctrl Pts',(1.41063490261845,-1.0531270779083,9.11649867113346));
#11392=CARTESIAN_POINT('Ctrl Pts',(1.40425077394034,-1.03451227992866,9.11772844880602));
#11393=CARTESIAN_POINT('Ctrl Pts',(1.40054311384935,-1.02350804817362,9.11845754089606));
#11394=CARTESIAN_POINT('Ctrl Pts',(1.38743321627117,-0.983891922355063,
9.12108926359253));
#11395=CARTESIAN_POINT('Ctrl Pts',(1.37837301648705,-0.955169575971337,
9.12301025198625));
#11396=CARTESIAN_POINT('Ctrl Pts',(1.35674321695494,-0.883093602061001,
9.12785574822883));
#11397=CARTESIAN_POINT('Ctrl Pts',(1.34467968281328,-0.839595782798345,
9.13080231114196));
#11398=CARTESIAN_POINT('Ctrl Pts',(1.29551571100217,-0.646677878181749,
9.14392772787879));
#11399=CARTESIAN_POINT('Ctrl Pts',(1.26823750831663,-0.494968703430431,
9.15438865258361));
#11400=CARTESIAN_POINT('Ctrl Pts',(1.22893725100035,-0.12661341600215,9.17942665836086));
#11401=CARTESIAN_POINT('Ctrl Pts',(1.22771743656247,0.090471240857646,9.19385490692827));
#11402=CARTESIAN_POINT('Ctrl Pts',(1.2518510976004,0.343438952699975,9.20998381864488));
#11403=CARTESIAN_POINT('Ctrl Pts',(1.2560692459071,0.380746399084559,9.21234653040841));
#11404=CARTESIAN_POINT('Ctrl Pts',(1.26358433561908,0.438201554196141,9.21596173385019));
#11405=CARTESIAN_POINT('Ctrl Pts',(1.26642229086129,0.458404959575393,9.21722848536505));
#11406=CARTESIAN_POINT('Ctrl Pts',(1.27157122891479,0.492693352333813,9.21937106890253));
#11407=CARTESIAN_POINT('Ctrl Pts',(1.27378425063996,0.506792214607541,9.22024996428723));
#11408=CARTESIAN_POINT('Ctrl Pts',(1.27845639667876,0.535319520210305,9.22202421197417));
#11409=CARTESIAN_POINT('Ctrl Pts',(1.2809203055303,0.549746847444394,9.22291939031988));
#11410=CARTESIAN_POINT('Ctrl Pts',(1.2872481709028,0.585336638259917,9.22512265418461));
#11411=CARTESIAN_POINT('Ctrl Pts',(1.29122592936376,0.606478344885927,9.226427104539));
#11412=CARTESIAN_POINT('Ctrl Pts',(1.30697438209144,0.685801753666355,9.23130640406682));
#11413=CARTESIAN_POINT('Ctrl Pts',(1.32014047879625,0.743696489950744,9.23483691795375));
#11414=CARTESIAN_POINT('Ctrl Pts',(1.3575002890913,0.889255213025787,9.24366292298356));
#11415=CARTESIAN_POINT('Ctrl Pts',(1.38381858613466,0.976321215388722,9.24889427254708));
#11416=CARTESIAN_POINT('Ctrl Pts',(1.47480778565485,1.23696993981106,9.2645786025982));
#11417=CARTESIAN_POINT('Ctrl Pts',(1.55077964248598,1.40618854585699,9.27477692940569));
#11418=CARTESIAN_POINT('Ctrl Pts',(1.70502975984947,1.6831802618863,9.29269784116597));
#11419=CARTESIAN_POINT('Ctrl Pts',(1.77620707446161,1.79435264594643,9.30027923709603));
#11420=CARTESIAN_POINT('Ctrl Pts',(1.86391059012287,1.91442972474918,9.3092798017825));
#11421=CARTESIAN_POINT('Ctrl Pts',(1.87394364872069,1.9279427025321,9.31030497078347));
#11422=CARTESIAN_POINT('Ctrl Pts',(1.89017138523617,1.94944498730195,9.31195712123199));
#11423=CARTESIAN_POINT('Ctrl Pts',(1.8962987615834,1.95748500665026,9.31257961611275));
#11424=CARTESIAN_POINT('Ctrl Pts',(1.90725636858591,1.97172354373008,9.3136907318954));
#11425=CARTESIAN_POINT('Ctrl Pts',(1.91207157520281,1.97793339555126,9.31417830191596));
#11426=CARTESIAN_POINT('Ctrl Pts',(1.92248150434882,1.99125746826845,9.31523095753061));
#11427=CARTESIAN_POINT('Ctrl Pts',(1.92808340188389,1.99836563140001,9.31579653070956));
#11428=CARTESIAN_POINT('Ctrl Pts',(1.94375989538178,2.01808586226907,9.31737654900322));
#11429=CARTESIAN_POINT('Ctrl Pts',(1.95389925840699,2.03064577346947,9.3183954198604));
#11430=CARTESIAN_POINT('Ctrl Pts',(2.01444756607069,2.1045064057208,9.32445907071313));
#11431=CARTESIAN_POINT('Ctrl Pts',(2.06700868473713,2.16399932389914,9.32963874012403));
#11432=CARTESIAN_POINT('Ctrl Pts',(2.26978689608714,2.37711743303975,9.34913649950054));
#11433=CARTESIAN_POINT('Ctrl Pts',(2.43305599542146,2.51755226466315,9.36387158596401));
#11434=CARTESIAN_POINT('Ctrl Pts',(2.74093952176487,2.73294150219422,9.38896817798124));
#11435=CARTESIAN_POINT('Ctrl Pts',(2.87952987834343,2.81518866994653,9.39947475373481));
#11436=CARTESIAN_POINT('Ctrl Pts',(3.04795702900409,2.89878325008511,9.41131052066808));
#11437=CARTESIAN_POINT('Ctrl Pts',(3.0723602282471,2.91051426528434,9.41300416302171));
#11438=CARTESIAN_POINT('Ctrl Pts',(3.1126952480273,2.92928191538089,9.41576946683301));
#11439=CARTESIAN_POINT('Ctrl Pts',(3.12854102844654,2.93649923566308,9.41684731348154));
#11440=CARTESIAN_POINT('Ctrl Pts',(3.15719932133499,2.94927289110232,9.41878164225623));
#11441=CARTESIAN_POINT('Ctrl Pts',(3.16999083872056,2.95487499517214,9.41963967485644));
#11442=CARTESIAN_POINT('Ctrl Pts',(3.19742244743444,2.96667689927876,9.42146851686997));
#11443=CARTESIAN_POINT('Ctrl Pts',(3.21207286133671,2.9728518822163,9.4224384645469));
#11444=CARTESIAN_POINT('Ctrl Pts',(3.25205272451414,2.98935561078739,9.42506737311239));
#11445=CARTESIAN_POINT('Ctrl Pts',(3.27746929624237,2.99947083771479,9.42671912057119));
#11446=CARTESIAN_POINT('Ctrl Pts',(3.41861780200445,3.05357338822391,9.43578932903667));
#11447=CARTESIAN_POINT('Ctrl Pts',(3.53668820235613,3.09118972042258,9.44299247588159));
#11448=CARTESIAN_POINT('Ctrl Pts',(3.80132963962856,3.15899012055374,9.45858169859357));
#11449=CARTESIAN_POINT('Ctrl Pts',(3.94842350481087,3.18595634035313,9.46688365126446));
#11450=CARTESIAN_POINT('Ctrl Pts',(4.26497726317687,3.22150103329119,9.48471988535488));
#11451=CARTESIAN_POINT('Ctrl Pts',(4.43430234091749,3.22710902719359,9.49424553703263));
#11452=CARTESIAN_POINT('Ctrl Pts',(4.63016688893988,3.21817837587943,9.50599930267023));
#11453=CARTESIAN_POINT('Ctrl Pts',(4.65705505683749,3.21661439212084,9.50762917500264));
#11454=CARTESIAN_POINT('Ctrl Pts',(4.69421431713357,3.2139852662894,9.50990811436239));
#11455=CARTESIAN_POINT('Ctrl Pts',(4.70450545833392,3.21320743783238,9.51054207211688));
#11456=CARTESIAN_POINT('Ctrl Pts',(4.72217056553544,3.21178689899271,9.51163538574469));
#11457=CARTESIAN_POINT('Ctrl Pts',(4.72954645462876,3.21116818450954,9.5120934170893));
#11458=CARTESIAN_POINT('Ctrl Pts',(4.74498026531459,3.20981998502131,9.51305515645851));
#11459=CARTESIAN_POINT('Ctrl Pts',(4.75303762487338,3.20908556037863,9.5135591490009));
#11460=CARTESIAN_POINT('Ctrl Pts',(4.77277326862014,3.20721170517433,9.51479816659046));
#11461=CARTESIAN_POINT('Ctrl Pts',(4.78444819446088,3.206038825815,9.51553502447527));
#11462=CARTESIAN_POINT('Ctrl Pts',(4.82687340356939,3.20154257311573,9.5182262151274));
#11463=CARTESIAN_POINT('Ctrl Pts',(4.85758074885276,3.19784043956469,9.52019998363712));
#11464=CARTESIAN_POINT('Ctrl Pts',(4.93459511234618,3.18742877891503,9.52520748049599));
#11465=CARTESIAN_POINT('Ctrl Pts',(4.98081723437808,3.18015177227774,9.52826507083558));
#11466=CARTESIAN_POINT('Ctrl Pts',(5.35619857844323,3.11264749751272,9.55343987891822));
#11467=CARTESIAN_POINT('Ctrl Pts',(5.67433219540271,3.00249483702527,9.57665383900076));
#11468=CARTESIAN_POINT('Ctrl Pts',(6.0274476628766,2.81467544986075,9.60240744874631));
#11469=CARTESIAN_POINT('Ctrl Pts',(6.0840911855857,2.78230459657241,9.60654937497545));
#11470=CARTESIAN_POINT('Ctrl Pts',(6.15895410478027,2.73645232010687,9.61204146543004));
#11471=CARTESIAN_POINT('Ctrl Pts',(6.17806766158924,2.72446782441143,9.61344534544333));
#11472=CARTESIAN_POINT('Ctrl Pts',(6.20946225631597,2.70432060666752,9.61575447174331));
#11473=CARTESIAN_POINT('Ctrl Pts',(6.22181568382887,2.69627268657626,9.61666392412165));
#11474=CARTESIAN_POINT('Ctrl Pts',(6.24528831253729,2.68075043441964,9.61839374398925));
#11475=CARTESIAN_POINT('Ctrl Pts',(6.25641695316132,2.67329100574122,9.61921464416099));
#11476=CARTESIAN_POINT('Ctrl Pts',(6.26827235891255,2.66523683945707,9.62009006891609));
#11477=CARTESIAN_POINT('Ctrl Pts',(6.26904560022436,2.66471103316141,9.62014717065128));
#11478=CARTESIAN_POINT('Ctrl Pts',(6.27061807886667,2.66364074206354,9.62026330243684));
#11479=CARTESIAN_POINT('Ctrl Pts',(6.27141730022208,2.6630962338653,9.62032233160112));
#11480=CARTESIAN_POINT('Ctrl Pts',(6.27305688328217,2.66197810771712,9.62044343781818));
#11481=CARTESIAN_POINT('Ctrl Pts',(6.27389721874535,2.661404451327,9.62050551341895));
#11482=CARTESIAN_POINT('Ctrl Pts',(6.27563407862643,2.66021757483399,9.62063382579028));
#11483=CARTESIAN_POINT('Ctrl Pts',(6.27653056508238,2.65960429918707,9.62070006046501));
#11484=CARTESIAN_POINT('Ctrl Pts',(6.2948981954135,2.647025587143,9.62205722674283));
#11485=CARTESIAN_POINT('Ctrl Pts',(6.31225160747897,2.63488848263993,9.62334166572541));
#11486=CARTESIAN_POINT('Ctrl Pts',(6.37581474063395,2.58949246836366,9.6280559916815));
#11487=CARTESIAN_POINT('Ctrl Pts',(6.42126200904066,2.55518068788699,9.63144542802615));
#11488=CARTESIAN_POINT('Ctrl Pts',(6.53285765499646,2.46618919740773,9.63983997420649));
#11489=CARTESIAN_POINT('Ctrl Pts',(6.5977769382923,2.41003752486692,9.64478906306018));
#11490=CARTESIAN_POINT('Ctrl Pts',(6.76636931785504,2.25201704023173,9.65794871897998));
#11491=CARTESIAN_POINT('Ctrl Pts',(6.8655215118462,2.14562059496171,9.6660214995519));
#11492=CARTESIAN_POINT('Ctrl Pts',(7.06237476122235,1.90346935274722,9.68349955097179));
#11493=CARTESIAN_POINT('Ctrl Pts',(7.15737231332272,1.76608273114505,9.69289979448135));
#11494=CARTESIAN_POINT('Ctrl Pts',(7.25486556595784,1.59869359353365,9.70451207683384));
#11495=CARTESIAN_POINT('Ctrl Pts',(7.2681368998726,1.57523587512892,9.70614302223234));
#11496=CARTESIAN_POINT('Ctrl Pts',(7.28608208116538,1.54256751548184,9.70842320453637));
#11497=CARTESIAN_POINT('Ctrl Pts',(7.29100860406667,1.53349599158762,9.70905731007857));
#11498=CARTESIAN_POINT('Ctrl Pts',(7.29939285755834,1.51787908070096,9.71015081099103));
#11499=CARTESIAN_POINT('Ctrl Pts',(7.30287181140591,1.51134509522469,9.71060888080686));
#11500=CARTESIAN_POINT('Ctrl Pts',(7.31010579137443,1.49764504630892,9.7115706207782));
#11501=CARTESIAN_POINT('Ctrl Pts',(7.31385636976276,1.49047678165576,9.7120745749631));
#11502=CARTESIAN_POINT('Ctrl Pts',(7.32297904085902,1.47288016108919,9.71331336351387));
#11503=CARTESIAN_POINT('Ctrl Pts',(7.32832123107935,1.46243650708679,9.71405002920095));
#11504=CARTESIAN_POINT('Ctrl Pts',(7.3475318437883,1.42436974928348,9.71673973492031));
#11505=CARTESIAN_POINT('Ctrl Pts',(7.3610592096519,1.39657763922609,9.71871218338841));
#11506=CARTESIAN_POINT('Ctrl Pts',(7.39403593651121,1.32627445428034,9.72371560995369));
#11507=CARTESIAN_POINT('Ctrl Pts',(7.41296354051476,1.28352757171271,9.72677040374641));
#11508=CARTESIAN_POINT('Ctrl Pts',(7.5593332846058,0.932528445929391,9.75187139471307));
#11509=CARTESIAN_POINT('Ctrl Pts',(7.63915824174214,0.606582303620659,9.77501056737986));
#11510=CARTESIAN_POINT('Ctrl Pts',(7.67298196595207,0.210372040167672,9.8006275531688));
#11511=CARTESIAN_POINT('Ctrl Pts',(7.67652483621499,0.146469788826136,9.80469393872761));
#11512=CARTESIAN_POINT('Ctrl Pts',(7.6786045497387,0.0652558286983623,9.8097819554415));
#11513=CARTESIAN_POINT('Ctrl Pts',(7.67890769140363,0.0480075293663571,
9.81085800952626));
#11514=CARTESIAN_POINT('Ctrl Pts',(7.6791688049711,0.0206493426565398,9.8125577449811));
#11515=CARTESIAN_POINT('Ctrl Pts',(7.67921772144553,0.0105408608178574,
9.81318425199337));
#11516=CARTESIAN_POINT('Ctrl Pts',(7.67921907723176,0.00043224100879341,
9.81380927132941));
#11517=CARTESIAN_POINT('',(7.6792185144777,-0.00195296268717014,8.31625837989182));
#11518=CARTESIAN_POINT('Ctrl Pts',(7.67921910621823,-1.20018596680688E-11,
9.56539764702567));
#11519=CARTESIAN_POINT('Ctrl Pts',(7.67921910621823,0.000928979248483444,
9.56534546463779));
#11520=CARTESIAN_POINT('Ctrl Pts',(7.67921870454109,0.00185797137808247,
9.56529327719194));
#11521=CARTESIAN_POINT('Ctrl Pts',(7.67908108221349,0.160998824745607,9.55635255496428));
#11522=CARTESIAN_POINT('Ctrl Pts',(7.66729393926749,0.318966012123944,9.54735584768415));
#11523=CARTESIAN_POINT('Ctrl Pts',(7.64121861529879,0.493795320519256,9.53665832976546));
#11524=CARTESIAN_POINT('Ctrl Pts',(7.63831687549237,0.512160121540664,9.53552529949506));
#11525=CARTESIAN_POINT('Ctrl Pts',(7.63366137680432,0.540056234942165,9.53378863017499));
#11526=CARTESIAN_POINT('Ctrl Pts',(7.63202320403941,0.549606793336955,9.53319127180097));
#11527=CARTESIAN_POINT('Ctrl Pts',(7.62898559348343,0.566849027923784,9.53210754245388));
#11528=CARTESIAN_POINT('Ctrl Pts',(7.62760121391902,0.574543153378958,9.53162202410102));
#11529=CARTESIAN_POINT('Ctrl Pts',(7.62447236094279,0.591576883365306,9.53054287359425));
#11530=CARTESIAN_POINT('Ctrl Pts',(7.62271459685533,0.60091373629595,9.52994851702363));
#11531=CARTESIAN_POINT('Ctrl Pts',(7.61745727106482,0.628175890443109,9.52820507911565));
#11532=CARTESIAN_POINT('Ctrl Pts',(7.61384665196991,0.646079039391844,9.52705002124847));
#11533=CARTESIAN_POINT('Ctrl Pts',(7.58048149277343,0.804556126150436,9.51674133023832));
#11534=CARTESIAN_POINT('Ctrl Pts',(7.54151157380808,0.943009835652374,9.50715272205079));
#11535=CARTESIAN_POINT('Ctrl Pts',(7.41696977463348,1.29374746990147,9.48205220968626));
#11536=CARTESIAN_POINT('Ctrl Pts',(7.31779480623073,1.50039525453802,9.4665017367109));
#11537=CARTESIAN_POINT('Ctrl Pts',(7.15162526328535,1.76914873444427,9.44593374946827));
#11538=CARTESIAN_POINT('Ctrl Pts',(7.10266214854912,1.84158048239401,9.44034332390495));
#11539=CARTESIAN_POINT('Ctrl Pts',(7.03562121897747,1.9325494825861,9.43325674475015));
#11540=CARTESIAN_POINT('Ctrl Pts',(7.02018593284587,1.95297957415063,9.43166062736506));
#11541=CARTESIAN_POINT('Ctrl Pts',(6.99500900985691,1.98549072806798,9.42911265003299));
#11542=CARTESIAN_POINT('Ctrl Pts',(6.98542098667627,1.99768883297143,9.428154802837));
#11543=CARTESIAN_POINT('Ctrl Pts',(6.9669968461074,2.02078321726404,9.42633758750628));
#11544=CARTESIAN_POINT('Ctrl Pts',(6.95817696770307,2.03169193765794,9.4254776013639));
#11545=CARTESIAN_POINT('Ctrl Pts',(6.93785154048757,2.05649806044339,9.42351809388139));
#11546=CARTESIAN_POINT('Ctrl Pts',(6.92629988962827,2.07035721062324,9.42242046693408));
#11547=CARTESIAN_POINT('Ctrl Pts',(6.89017039888718,2.11297099137802,9.4190359302423));
#11548=CARTESIAN_POINT('Ctrl Pts',(6.86520171802142,2.14139108476953,9.41676505221556));
#11549=CARTESIAN_POINT('Ctrl Pts',(6.74027412602419,2.27863671791143,9.40571825013802));
#11550=CARTESIAN_POINT('Ctrl Pts',(6.63340781961554,2.38094428309651,9.39724061723168));
#11551=CARTESIAN_POINT('Ctrl Pts',(6.36955494584345,2.60086922266454,9.37785829637783));
#11552=CARTESIAN_POINT('Ctrl Pts',(6.20813059345895,2.71221190874339,9.36710733478918));
#11553=CARTESIAN_POINT('Ctrl Pts',(6.00796732460519,2.82491209176933,9.35395477517526));
#11554=CARTESIAN_POINT('Ctrl Pts',(5.97805991253678,2.84113293260986,9.35199320792766));
#11555=CARTESIAN_POINT('Ctrl Pts',(5.89001273870715,2.88709797537025,9.34621301093907));
#11556=CARTESIAN_POINT('Ctrl Pts',(5.83122243176929,2.9155503890975,9.34234684049696));
#11557=CARTESIAN_POINT('Ctrl Pts',(5.75721662172873,2.94863055274336,9.33742280260646));
#11558=CARTESIAN_POINT('Ctrl Pts',(5.74277333751813,2.95495983679112,9.33645914857957));
#11559=CARTESIAN_POINT('Ctrl Pts',(5.71995876033456,2.96475860091453,9.33493190334445));
#11560=CARTESIAN_POINT('Ctrl Pts',(5.71161807211486,2.96829930035014,9.33437250629055));
#11561=CARTESIAN_POINT('Ctrl Pts',(5.69674516361641,2.97453909349972,9.33337293359196));
#11562=CARTESIAN_POINT('Ctrl Pts',(5.6902188654052,2.97725192850503,9.33293359736946));
#11563=CARTESIAN_POINT('Ctrl Pts',(5.67459404603141,2.98368661694464,9.33188007457149));
#11564=CARTESIAN_POINT('Ctrl Pts',(5.66548744366219,2.98738829931156,9.33126469738929));
#11565=CARTESIAN_POINT('Ctrl Pts',(5.63791107676984,2.99845089169941,9.32939745888321));
#11566=CARTESIAN_POINT('Ctrl Pts',(5.61939038516162,3.0056824404082,9.32813830207602));
#11567=CARTESIAN_POINT('Ctrl Pts',(5.50229806781728,3.05015783442555,9.32015095681529));
#11568=CARTESIAN_POINT('Ctrl Pts',(5.40202519605113,3.08271637719427,9.31319428078877));
#11569=CARTESIAN_POINT('Ctrl Pts',(5.07905714932123,3.17034331364465,9.29078539536379));
#11570=CARTESIAN_POINT('Ctrl Pts',(4.85196264475413,3.20660156158906,9.27508030286756));
#11571=CARTESIAN_POINT('Ctrl Pts',(4.616822210384,3.21876404643781,9.25956287856023));
#11572=CARTESIAN_POINT('Ctrl Pts',(4.61070230772222,3.21906309737384,9.25915947788318));
#11573=CARTESIAN_POINT('Ctrl Pts',(4.49241392159903,3.22450519353561,9.25137143399491));
#11574=CARTESIAN_POINT('Ctrl Pts',(4.38004385680494,3.22380052051984,9.2441349681423));
#11575=CARTESIAN_POINT('Ctrl Pts',(4.24061651282348,3.21562959926465,9.2353606021019));
#11576=CARTESIAN_POINT('Ctrl Pts',(4.21332549654666,3.21368127246703,9.23365268476979));
#11577=CARTESIAN_POINT('Ctrl Pts',(4.17006267615006,3.21003842805254,9.23095972401324));
#11578=CARTESIAN_POINT('Ctrl Pts',(4.15407351087644,3.2085716871511,9.22996760015403));
#11579=CARTESIAN_POINT('Ctrl Pts',(4.12421772103346,3.20560775471976,9.22812072759481));
#11580=CARTESIAN_POINT('Ctrl Pts',(4.11034862242366,3.20413992835018,9.22726507958984));
#11581=CARTESIAN_POINT('Ctrl Pts',(4.07940940498913,3.2006622679169,9.22536122264338));
#11582=CARTESIAN_POINT('Ctrl Pts',(4.06234487629347,3.19860580265221,9.2243145036489));
#11583=CARTESIAN_POINT('Ctrl Pts',(4.01209575932957,3.19214198894333,9.2212416203021));
#11584=CARTESIAN_POINT('Ctrl Pts',(3.97896183375215,3.18735393080534,9.21922743830035));
#11585=CARTESIAN_POINT('Ctrl Pts',(3.90373524086754,3.17528378692003,9.21467814508613));
#11586=CARTESIAN_POINT('Ctrl Pts',(3.86170031213639,3.16767930432509,9.21215310095929));
#11587=CARTESIAN_POINT('Ctrl Pts',(3.7212926299111,3.13938473560258,9.20376119053553));
#11588=CARTESIAN_POINT('Ctrl Pts',(3.62373618248316,3.11492842314315,9.19800269917268));
#11589=CARTESIAN_POINT('Ctrl Pts',(3.40256911854199,3.04834843071644,9.18493426390847));
#11590=CARTESIAN_POINT('Ctrl Pts',(3.28005828268848,3.00319687258149,9.17768701315366));
#11591=CARTESIAN_POINT('Ctrl Pts',(3.0835836036963,2.91691316400997,9.16565599881432));
#11592=CARTESIAN_POINT('Ctrl Pts',(3.00790311934487,2.88007854927287,9.16091418279482));
#11593=CARTESIAN_POINT('Ctrl Pts',(2.85518445675,2.79820521440139,9.15096023855335));
#11594=CARTESIAN_POINT('Ctrl Pts',(2.77840373927628,2.75284554436341,9.14574115564873));
#11595=CARTESIAN_POINT('Ctrl Pts',(2.69041031728837,2.69581181023556,9.13938419453255));
#11596=CARTESIAN_POINT('Ctrl Pts',(2.67727450207947,2.68716049020513,9.13842499582302));
#11597=CARTESIAN_POINT('Ctrl Pts',(2.65598477174093,2.67291442082524,9.13685275024214));
#11598=CARTESIAN_POINT('Ctrl Pts',(2.64779217954587,2.66737757144264,9.13624342704031));
#11599=CARTESIAN_POINT('Ctrl Pts',(2.63316200120205,2.65739157825737,9.13514733235075));
#11600=CARTESIAN_POINT('Ctrl Pts',(2.62671498926561,2.65295659002752,9.13466151125581));
#11601=CARTESIAN_POINT('Ctrl Pts',(2.61261755429364,2.64318293799529,9.13359296167823));
#11602=CARTESIAN_POINT('Ctrl Pts',(2.60497424168383,2.63783459502239,9.13300959757436));
#11603=CARTESIAN_POINT('Ctrl Pts',(2.58310667852573,2.62239108835879,9.13132927099558));
#11604=CARTESIAN_POINT('Ctrl Pts',(2.56894127601944,2.61221370956518,9.13022695600439));
#11605=CARTESIAN_POINT('Ctrl Pts',(2.46617285079706,2.53710561252241,9.12213244115718));
#11606=CARTESIAN_POINT('Ctrl Pts',(2.38086696761499,2.46780362593014,9.114883216524));
#11607=CARTESIAN_POINT('Ctrl Pts',(2.12866586809538,2.24057693872543,9.09214864491327));
#11608=CARTESIAN_POINT('Ctrl Pts',(1.97495576443553,2.06904829350985,9.07642041301047));
#11609=CARTESIAN_POINT('Ctrl Pts',(1.77242115453936,1.78765196040579,9.05357734024762));
#11610=CARTESIAN_POINT('Ctrl Pts',(1.70927570441868,1.68900764002873,9.04602532154727));
#11611=CARTESIAN_POINT('Ctrl Pts',(1.63800597973549,1.56305744109691,9.03693134391803));
#11612=CARTESIAN_POINT('Ctrl Pts',(1.62469144566678,1.53880418423814,9.03520392313672));
#11613=CARTESIAN_POINT('Ctrl Pts',(1.60411296453515,1.50014734094187,9.0324872429685));
#11614=CARTESIAN_POINT('Ctrl Pts',(1.59664223650824,1.4858559465593,9.03149069189127));
#11615=CARTESIAN_POINT('Ctrl Pts',(1.58291364085979,1.45910619690964,9.02963968737945));
#11616=CARTESIAN_POINT('Ctrl Pts',(1.57662876521555,1.44666220188011,9.02878429972129));
#11617=CARTESIAN_POINT('Ctrl Pts',(1.56281654165101,1.41886739591356,9.02688616956951));
#11618=CARTESIAN_POINT('Ctrl Pts',(1.55533016776276,1.40349660809365,9.0258448738598));
#11619=CARTESIAN_POINT('Ctrl Pts',(1.53374105391334,1.35825959221902,9.02280424365691));
#11620=CARTESIAN_POINT('Ctrl Pts',(1.51997442969955,1.32823473977894,9.02081650635699));
#11621=CARTESIAN_POINT('Ctrl Pts',(1.48975999653348,1.25957042538472,9.01633561077226));
#11622=CARTESIAN_POINT('Ctrl Pts',(1.47360078736609,1.22081014871945,9.01385207868912));
#11623=CARTESIAN_POINT('Ctrl Pts',(1.42227687165443,1.09059347651488,9.00564634477162));
#11624=CARTESIAN_POINT('Ctrl Pts',(1.39052424784582,0.997848125242633,9.00002697589843));
#11625=CARTESIAN_POINT('Ctrl Pts',(1.32586111105626,0.776525130115015,8.98696760051298));
#11626=CARTESIAN_POINT('Ctrl Pts',(1.29656636971623,0.647080421732769,8.97960075979825));
#11627=CARTESIAN_POINT('Ctrl Pts',(1.26215553017199,0.435019620977347,8.96755879082327));
#11628=CARTESIAN_POINT('Ctrl Pts',(1.25209532960429,0.353368032262696,8.96292675735798));
#11629=CARTESIAN_POINT('Ctrl Pts',(1.23736822778804,0.179127570220786,8.95289841079886));
#11630=CARTESIAN_POINT('Ctrl Pts',(1.23355060378722,0.0865458005470657,
8.94748415899529));
#11631=CARTESIAN_POINT('Ctrl Pts',(1.23375466895951,-0.0219365159964151,
8.94090896896696));
#11632=CARTESIAN_POINT('Ctrl Pts',(1.23390181612946,-0.0378099516884193,
8.93994106217947));
#11633=CARTESIAN_POINT('Ctrl Pts',(1.23433165877112,-0.0636119274055645,
8.93835737351153));
#11634=CARTESIAN_POINT('Ctrl Pts',(1.23454299988932,-0.0735415990230416,
8.9377454057285));
#11635=CARTESIAN_POINT('Ctrl Pts',(1.23500297903915,-0.0912952931957789,
8.93664652168846));
#11636=CARTESIAN_POINT('Ctrl Pts',(1.23523422697856,-0.0991195726215972,
8.93616057729858));
#11637=CARTESIAN_POINT('Ctrl Pts',(1.23580238771824,-0.116231778231468,
8.93509411985661));
#11638=CARTESIAN_POINT('Ctrl Pts',(1.2361509670397,-0.12551898385345,8.93451298942317));
#11639=CARTESIAN_POINT('Ctrl Pts',(1.23726241310558,-0.152066911768491,
8.93284536390891));
#11640=CARTESIAN_POINT('Ctrl Pts',(1.23812390864203,-0.169322878409737,
8.93175363800632));
#11641=CARTESIAN_POINT('Ctrl Pts',(1.24520168967922,-0.291376725418134,
8.92398055944772));
#11642=CARTESIAN_POINT('Ctrl Pts',(1.25639623687191,-0.395812937733077,
8.91706414910813));
#11643=CARTESIAN_POINT('Ctrl Pts',(1.30667914247089,-0.716312161538888,
8.89536709799072));
#11644=CARTESIAN_POINT('Ctrl Pts',(1.36275520070235,-0.929099397203223,
8.88033493726173));
#11645=CARTESIAN_POINT('Ctrl Pts',(1.48609837219437,-1.25703835319484,8.85713857048745));
#11646=CARTESIAN_POINT('Ctrl Pts',(1.53959816372505,-1.37663326723985,8.84866028843823));
#11647=CARTESIAN_POINT('Ctrl Pts',(1.6134158586213,-1.51788541816975,8.83863829944873));
#11648=CARTESIAN_POINT('Ctrl Pts',(1.62693454821042,-1.54293946088116,8.83686000024468));
#11649=CARTESIAN_POINT('Ctrl Pts',(1.64871703675081,-1.58205935714622,8.83408151332681));
#11650=CARTESIAN_POINT('Ctrl Pts',(1.65675843348644,-1.59624674087481,8.83307347065534));
#11651=CARTESIAN_POINT('Ctrl Pts',(1.67180157114896,-1.62232384028896,8.8312197086133));
#11652=CARTESIAN_POINT('Ctrl Pts',(1.67877261068145,-1.63423074004063,8.83037291119591));
#11653=CARTESIAN_POINT('Ctrl Pts',(1.6944097390735,-1.66055064123587,8.82850009316388));
#11654=CARTESIAN_POINT('Ctrl Pts',(1.70311265109821,-1.67494138031732,8.82747543901985));
#11655=CARTESIAN_POINT('Ctrl Pts',(1.72852904315753,-1.71623531232519,8.82453277910791));
#11656=CARTESIAN_POINT('Ctrl Pts',(1.74552726119505,-1.74296157598743,8.82262523867793));
#11657=CARTESIAN_POINT('Ctrl Pts',(1.88652935879342,-1.95760453343155,8.80726958512924));
#11658=CARTESIAN_POINT('Ctrl Pts',(2.02952215622663,-2.13231125178817,8.7946048573358));
#11659=CARTESIAN_POINT('Ctrl Pts',(2.34010307766225,-2.43966393757368,8.77016899421306));
#11660=CARTESIAN_POINT('Ctrl Pts',(2.50492532105668,-2.57340583191477,8.75842800160268));
#11661=CARTESIAN_POINT('Ctrl Pts',(2.70298346429899,-2.70408198943641,8.74418389645411));
#11662=CARTESIAN_POINT('Ctrl Pts',(2.72449118569299,-2.71790796241603,8.74263511190485));
#11663=CARTESIAN_POINT('Ctrl Pts',(2.75472452676728,-2.73683851359313,8.74045190722554));
#11664=CARTESIAN_POINT('Ctrl Pts',(2.76331373284463,-2.74216056029999,8.73983098896695));
#11665=CARTESIAN_POINT('Ctrl Pts',(2.77818978169496,-2.75128152444725,8.73875417118699));
#11666=CARTESIAN_POINT('Ctrl Pts',(2.7844649064416,-2.75509953926674,8.73829950656211));
#11667=CARTESIAN_POINT('Ctrl Pts',(2.79772659707692,-2.76310644206574,8.737337597468));
#11668=CARTESIAN_POINT('Ctrl Pts',(2.80471605401932,-2.76729033022415,8.7368300245143));
#11669=CARTESIAN_POINT('Ctrl Pts',(2.82205124340896,-2.77757810069329,8.735569790862));
#11670=CARTESIAN_POINT('Ctrl Pts',(2.83241531176789,-2.78365068170309,8.73481515603995));
#11671=CARTESIAN_POINT('Ctrl Pts',(2.87125690608195,-2.80611824627147,8.73198327799059));
#11672=CARTESIAN_POINT('Ctrl Pts',(2.89994963406066,-2.82213470074953,8.72988391942714));
#11673=CARTESIAN_POINT('Ctrl Pts',(3.11536615215668,-2.93809717043213,8.71409573711287));
#11674=CARTESIAN_POINT('Ctrl Pts',(3.31127969950151,-3.0198513671987,8.69962580070306));
#11675=CARTESIAN_POINT('Ctrl Pts',(3.70505476047866,-3.14030303706421,8.67183545717458));
#11676=CARTESIAN_POINT('Ctrl Pts',(3.90138712320724,-3.18088578870972,8.65855784381704));
#11677=CARTESIAN_POINT('Ctrl Pts',(4.14180448333265,-3.20762411232021,8.64320293557294));
#11678=CARTESIAN_POINT('Ctrl Pts',(4.18345330094341,-3.21143720239514,8.64057341405049));
#11679=CARTESIAN_POINT('Ctrl Pts',(4.24369109510046,-3.21577176280041,8.63681259202144));
#11680=CARTESIAN_POINT('Ctrl Pts',(4.26222750451843,-3.21694462740009,8.63566106843576));
#11681=CARTESIAN_POINT('Ctrl Pts',(4.29490093229314,-3.21872854892906,8.63364117886267));
#11682=CARTESIAN_POINT('Ctrl Pts',(4.30903363253705,-3.21940686117232,8.63277073186177));
#11683=CARTESIAN_POINT('Ctrl Pts',(4.33828138555654,-3.22061763558807,8.63097586696577));
#11684=CARTESIAN_POINT('Ctrl Pts',(4.35339666174785,-3.2211368141386,8.6300518855014));
#11685=CARTESIAN_POINT('Ctrl Pts',(4.39232011918263,-3.22219949176642,8.6276815078878));
#11686=CARTESIAN_POINT('Ctrl Pts',(4.41613194417036,-3.22258554846624,8.62624004953389));
#11687=CARTESIAN_POINT('Ctrl Pts',(4.51869826278476,-3.22311140355569,8.62006599642272));
#11688=CARTESIAN_POINT('Ctrl Pts',(4.59744261371916,-3.22062843877784,8.61541526334332));
#11689=CARTESIAN_POINT('Ctrl Pts',(4.81359696306451,-3.20586842908658,8.60281850345185));
#11690=CARTESIAN_POINT('Ctrl Pts',(4.95043414859862,-3.18765357362187,8.59503880545987));
#11691=CARTESIAN_POINT('Ctrl Pts',(5.29806979917756,-3.11844808992389,8.5751848008833));
#11692=CARTESIAN_POINT('Ctrl Pts',(5.50562206020022,-3.05487583790019,8.5632575008652));
#11693=CARTESIAN_POINT('Ctrl Pts',(5.7411787905244,-2.95586894980729,8.54810622880221));
#11694=CARTESIAN_POINT('Ctrl Pts',(5.77687233089303,-2.94009782790998,8.54576325528096));
#11695=CARTESIAN_POINT('Ctrl Pts',(5.82430658877819,-2.91810113794584,8.54257457692905));
#11696=CARTESIAN_POINT('Ctrl Pts',(5.83630945116774,-2.91244471850141,8.54176117690007));
#11697=CARTESIAN_POINT('Ctrl Pts',(5.85511333458684,-2.90344094808087,8.54047607343421));
#11698=CARTESIAN_POINT('Ctrl Pts',(5.86193821675647,-2.90014337457348,8.54000739085381));
#11699=CARTESIAN_POINT('Ctrl Pts',(5.87576635642736,-2.89340176701809,8.53905306794945));
#11700=CARTESIAN_POINT('Ctrl Pts',(5.88276875855161,-2.8899563606369,8.53856733150461));
#11701=CARTESIAN_POINT('Ctrl Pts',(5.89925924756005,-2.88176798014905,8.53741766891512));
#11702=CARTESIAN_POINT('Ctrl Pts',(5.90873652238066,-2.87700355020117,8.53675242885094));
#11703=CARTESIAN_POINT('Ctrl Pts',(5.92896577514654,-2.86670844625675,8.53532306453999));
#11704=CARTESIAN_POINT('Ctrl Pts',(5.93971046608167,-2.86116389145982,8.53455813576977));
#11705=CARTESIAN_POINT('Ctrl Pts',(5.96911069580212,-2.84578245441171,8.53244985369507));
#11706=CARTESIAN_POINT('Ctrl Pts',(5.98770093686906,-2.83582287642731,8.53109980657977));
#11707=CARTESIAN_POINT('Ctrl Pts',(6.04723101679982,-2.80317408374387,8.52672500247137));
#11708=CARTESIAN_POINT('Ctrl Pts',(6.08777324691131,-2.7797760262058,8.52366619160925));
#11709=CARTESIAN_POINT('Ctrl Pts',(6.41431278253724,-2.58171714974494,8.4984575836249));
#11710=CARTESIAN_POINT('Ctrl Pts',(6.67200624246284,-2.36429467617147,8.47520927718465));
#11711=CARTESIAN_POINT('Ctrl Pts',(6.93404981340766,-2.06201681177209,8.44945534797583));
#11712=CARTESIAN_POINT('Ctrl Pts',(6.97502514629658,-2.01176438373979,8.44533941364197));
#11713=CARTESIAN_POINT('Ctrl Pts',(7.0284249128865,-1.94208342591629,8.43984758741855));
#11714=CARTESIAN_POINT('Ctrl Pts',(7.04219570772101,-1.92371065671693,8.4384189906345));
#11715=CARTESIAN_POINT('Ctrl Pts',(7.06460096029538,-1.89314261959641,8.43607350344447));
#11716=CARTESIAN_POINT('Ctrl Pts',(7.07334887032411,-1.88103191322775,8.43515222794963));
#11717=CARTESIAN_POINT('Ctrl Pts',(7.09026642093851,-1.85726461894156,8.43335954003556));
#11718=CARTESIAN_POINT('Ctrl Pts',(7.098443660284,-1.84561388857948,8.43248784898087));
#11719=CARTESIAN_POINT('Ctrl Pts',(7.11759174077314,-1.8179441226612,8.43043408051115));
#11720=CARTESIAN_POINT('Ctrl Pts',(7.12849561901404,-1.80187925502417,8.42925456087466));
#11721=CARTESIAN_POINT('Ctrl Pts',(7.16447121463733,-1.74783104754734,8.42532809204456));
#11722=CARTESIAN_POINT('Ctrl Pts',(7.18888412320446,-1.709414307437,8.42260568762478));
#11723=CARTESIAN_POINT('Ctrl Pts',(7.2453806841808,-1.61620528356107,8.41615118502481));
#11724=CARTESIAN_POINT('Ctrl Pts',(7.2766754419555,-1.56095619535568,8.412446381932));
#11725=CARTESIAN_POINT('Ctrl Pts',(7.41819558545888,-1.2929425944155,8.39496273568616));
#11726=CARTESIAN_POINT('Ctrl Pts',(7.50609147992221,-1.06926399160712,8.38186764287226));
#11727=CARTESIAN_POINT('Ctrl Pts',(7.58606020599265,-0.772268420479377,
8.36444103141177));
#11728=CARTESIAN_POINT('Ctrl Pts',(7.60165288054581,-0.706085748941868,
8.36055045159957));
#11729=CARTESIAN_POINT('Ctrl Pts',(7.62726270620167,-0.57958427145637,8.35301918685649));
#11730=CARTESIAN_POINT('Ctrl Pts',(7.63767898783902,-0.519377124168955,
8.34939458018844));
#11731=CARTESIAN_POINT('Ctrl Pts',(7.64857245229546,-0.443656866994801,
8.34474539364199));
#11732=CARTESIAN_POINT('Ctrl Pts',(7.65065798754777,-0.428383655577541,
8.34380303184777));
#11733=CARTESIAN_POINT('Ctrl Pts',(7.65378488134748,-0.404190592809645,
8.34230221639636));
#11734=CARTESIAN_POINT('Ctrl Pts',(7.6548986933696,-0.395280119225564,8.34174772096573));
#11735=CARTESIAN_POINT('Ctrl Pts',(7.65689661803388,-0.378735224277724,
8.34071472768886));
#11736=CARTESIAN_POINT('Ctrl Pts',(7.6577906759714,-0.371102183949988,8.34023679040597));
#11737=CARTESIAN_POINT('Ctrl Pts',(7.6595268722726,-0.355806045237808,8.33927634923776));
#11738=CARTESIAN_POINT('Ctrl Pts',(7.66036882904639,-0.348143013255039,
8.33879384922559));
#11739=CARTESIAN_POINT('Ctrl Pts',(7.66225149399062,-0.330422577657364,
8.3376751077898));
#11740=CARTESIAN_POINT('Ctrl Pts',(7.66327237515316,-0.320363208981211,
8.3370378139275));
#11741=CARTESIAN_POINT('Ctrl Pts',(7.6658015915591,-0.294216968424916,8.33537589654803));
#11742=CARTESIAN_POINT('Ctrl Pts',(7.66723629441381,-0.278123471324824,
8.33434758398818));
#11743=CARTESIAN_POINT('Ctrl Pts',(7.67560750110016,-0.175501658053048,
8.32775910133968));
#11744=CARTESIAN_POINT('Ctrl Pts',(7.67916592121515,-0.0887415669224956,
8.32204787422042));
#11745=CARTESIAN_POINT('Ctrl Pts',(7.6792185144777,-0.00195296268717014,
8.31625837989182));
#11746=CARTESIAN_POINT('Ctrl Pts',(7.67921851169523,-0.00195754888720522,
8.31625868582799));
#11747=CARTESIAN_POINT('Ctrl Pts',(7.67921890804601,-0.0013050291805212,
8.31621515756297));
#11748=CARTESIAN_POINT('Ctrl Pts',(7.67921910621822,-0.000652512869385687,
8.31617162515749));
#11749=CARTESIAN_POINT('Ctrl Pts',(7.67921910621823,-4.32305015001326E-11,
8.31612808864258));
#11750=CARTESIAN_POINT('Origin',(4.45646910621825,-5.13094777615093E-16,
-2.31077344927308));
#11751=CARTESIAN_POINT('',(7.67921910621823,-4.71466720739905E-12,7.06143953130409));
#11752=CARTESIAN_POINT('',(7.67921910621823,3.2100258423573E-11,7.30846150265208));
#11753=CARTESIAN_POINT('',(7.67921910621823,-3.51191647465084E-13,-2.31077344927308));
#11754=CARTESIAN_POINT('',(7.6792190806041,-0.00206625803567177,7.30858154752831));
#11755=CARTESIAN_POINT('Ctrl Pts',(7.67921910621823,3.2100258423573E-11,
7.30846150265207));
#11756=CARTESIAN_POINT('Ctrl Pts',(7.67921910621824,-0.000687215974718567,
7.30850105516546));
#11757=CARTESIAN_POINT('Ctrl Pts',(7.67921888640636,-0.00137443588253173,
7.30854061414169));
#11758=CARTESIAN_POINT('Ctrl Pts',(7.6792184467751,-0.00206165958607078,
7.30858017961946));
#11759=CARTESIAN_POINT('Ctrl Pts',(7.67921844378978,-0.00206632091524094,
7.3085804479859));
#11760=CARTESIAN_POINT('Ctrl Pts',(7.67918020638304,-0.0617035129651612,
7.3120139379522));
#11761=CARTESIAN_POINT('Ctrl Pts',(7.67748658974212,-0.121325551268667,
7.31549377261651));
#11762=CARTESIAN_POINT('Ctrl Pts',(7.67242000325691,-0.211463230508943,
7.32087119381463));
#11763=CARTESIAN_POINT('Ctrl Pts',(7.67026365826296,-0.242035732280913,
7.32271546731949));
#11764=CARTESIAN_POINT('Ctrl Pts',(7.66679089382596,-0.282948839811236,
7.32521639024807));
#11765=CARTESIAN_POINT('Ctrl Pts',(7.66585977297981,-0.293321610761411,
7.32585328936783));
#11766=CARTESIAN_POINT('Ctrl Pts',(7.66414196846598,-0.311469816463751,
7.32697285839252));
#11767=CARTESIAN_POINT('Ctrl Pts',(7.66337724195445,-0.319247308115157,
7.32745434428977));
#11768=CARTESIAN_POINT('Ctrl Pts',(7.66181770050518,-0.334537018894052,
7.32840435288995));
#11769=CARTESIAN_POINT('Ctrl Pts',(7.66102474504478,-0.342049389227136,
7.32887277415009));
#11770=CARTESIAN_POINT('Ctrl Pts',(7.65925805141564,-0.358241281463178,
7.32988604944475));
#11771=CARTESIAN_POINT('Ctrl Pts',(7.65827544404199,-0.366919628846942,
7.33043138121957));
#11772=CARTESIAN_POINT('Ctrl Pts',(7.65554427546374,-0.390194491264422,
7.33189977082851));
#11773=CARTESIAN_POINT('Ctrl Pts',(7.65373111810975,-0.404783012952968,
7.33282631555129));
#11774=CARTESIAN_POINT('Ctrl Pts',(7.64514939637772,-0.470172437357681,
7.33700547659333));
#11775=CARTESIAN_POINT('Ctrl Pts',(7.63726979041701,-0.520817092241585,
7.34031311758333));
#11776=CARTESIAN_POINT('Ctrl Pts',(7.61659074472771,-0.63563234806109,7.34794181485242));
#11777=CARTESIAN_POINT('Ctrl Pts',(7.6030376960173,-0.699644529982602,7.35228830604115));
#11778=CARTESIAN_POINT('Ctrl Pts',(7.53514353935692,-0.978186076470445,
7.37149837338241));
#11779=CARTESIAN_POINT('Ctrl Pts',(7.46072994356382,-1.18722989462073,7.38664401679061));
#11780=CARTESIAN_POINT('Ctrl Pts',(7.31189390507405,-1.49938982229062,7.40947636014331));
#11781=CARTESIAN_POINT('Ctrl Pts',(7.25183399838337,-1.60859015487668,7.41752141132423));
#11782=CARTESIAN_POINT('Ctrl Pts',(7.17102722442641,-1.73725135190454,7.42706402989331));
#11783=CARTESIAN_POINT('Ctrl Pts',(7.15616147287261,-1.76026396790633,7.4287737602139));
#11784=CARTESIAN_POINT('Ctrl Pts',(7.13220263814914,-1.79633534285425,7.43145901354115));
#11785=CARTESIAN_POINT('Ctrl Pts',(7.12330345040149,-1.80952070810709,7.43244171590857));
#11786=CARTESIAN_POINT('Ctrl Pts',(7.10640998992296,-1.83415534870922,7.43428010288028));
#11787=CARTESIAN_POINT('Ctrl Pts',(7.09843825459297,-1.84561955967894,7.43513661089269));
#11788=CARTESIAN_POINT('Ctrl Pts',(7.08036672374754,-1.87125133572545,7.43705400370565));
#11789=CARTESIAN_POINT('Ctrl Pts',(7.07022615083744,-1.88538972069481,7.43811329921883));
#11790=CARTESIAN_POINT('Ctrl Pts',(7.04403919945474,-1.92128324234704,7.44080735050458));
#11791=CARTESIAN_POINT('Ctrl Pts',(7.02783250030479,-1.94292013403791,7.44243588926601));
#11792=CARTESIAN_POINT('Ctrl Pts',(6.91411423935617,-2.09082505716037,7.45360588244969));
#11793=CARTESIAN_POINT('Ctrl Pts',(6.80761068029022,-2.20991211346664,7.46277599905399));
#11794=CARTESIAN_POINT('Ctrl Pts',(6.50215932831748,-2.50425576562502,7.48671709111689));
#11795=CARTESIAN_POINT('Ctrl Pts',(6.28974365737954,-2.66368421642327,7.50106549903362));
#11796=CARTESIAN_POINT('Ctrl Pts',(6.03810119144741,-2.80806174922007,7.518295346561));
#11797=CARTESIAN_POINT('Ctrl Pts',(6.01578179550669,-2.82051674223762,7.51982600830751));
#11798=CARTESIAN_POINT('Ctrl Pts',(5.97631918044489,-2.84192668803427,7.52254084281685));
#11799=CARTESIAN_POINT('Ctrl Pts',(5.95923881759403,-2.85099538778073,7.52371863883487));
#11800=CARTESIAN_POINT('Ctrl Pts',(5.93348912295942,-2.8643713297818,7.52549990586779));
#11801=CARTESIAN_POINT('Ctrl Pts',(5.92487996514342,-2.86879430919172,7.52609639684756));
#11802=CARTESIAN_POINT('Ctrl Pts',(5.91622426249262,-2.87319203102394,7.52669718606732));
#11803=CARTESIAN_POINT('Ctrl Pts',(5.91619738017794,-2.87320568870586,7.52669905196951));
#11804=CARTESIAN_POINT('Ctrl Pts',(5.91614332399392,-2.87323315124092,7.52670280403155));
#11805=CARTESIAN_POINT('Ctrl Pts',(5.91611615016522,-2.87324695606307,7.52670469018881));
#11806=CARTESIAN_POINT('Ctrl Pts',(5.91606150714547,-2.87327471478184,7.52670848302596));
#11807=CARTESIAN_POINT('Ctrl Pts',(5.91603403793397,-2.87328866867825,7.52671038970751));
#11808=CARTESIAN_POINT('Ctrl Pts',(5.91597880022802,-2.87331672750524,7.5267142238661));
#11809=CARTESIAN_POINT('Ctrl Pts',(5.9159510318188,-2.87333083238168,7.52671615133745));
#11810=CARTESIAN_POINT('Ctrl Pts',(5.91589519186165,-2.87335919509461,7.526720027344));
#11811=CARTESIAN_POINT('Ctrl Pts',(5.91586712023358,-2.8733734529607,7.526721975885));
#11812=CARTESIAN_POINT('Ctrl Pts',(5.91581066986365,-2.87340212363845,7.52672589430751));
#11813=CARTESIAN_POINT('Ctrl Pts',(5.91578229109896,-2.87341653645034,7.52672786419085));
#11814=CARTESIAN_POINT('Ctrl Pts',(5.91572522238854,-2.8734455190511,7.52673182558112));
#11815=CARTESIAN_POINT('Ctrl Pts',(5.91569653241074,-2.87346008884462,7.52673381709053));
#11816=CARTESIAN_POINT('Ctrl Pts',(5.91563883706423,-2.87348938751146,7.52673782202595));
#11817=CARTESIAN_POINT('Ctrl Pts',(5.91560983180642,-2.87350411631655,7.52673983544451));
#11818=CARTESIAN_POINT('Ctrl Pts',(5.91555150177167,-2.87353373506692,7.5267438844856));
#11819=CARTESIAN_POINT('Ctrl Pts',(5.91552217695326,-2.87354862502103,7.52674592011126));
#11820=CARTESIAN_POINT('Ctrl Pts',(5.9154632035932,-2.87357856816732,7.52675001385919));
#11821=CARTESIAN_POINT('Ctrl Pts',(5.91543355502112,-2.87359362136243,7.52675207198385));
#11822=CARTESIAN_POINT('Ctrl Pts',(5.91537392983196,-2.87362389314725,7.5267562110306));
#11823=CARTESIAN_POINT('Ctrl Pts',(5.91534395319029,-2.87363911173661,7.52675829195469));
#11824=CARTESIAN_POINT('Ctrl Pts',(5.9152836674988,-2.87366971648641,7.52676247690405));
#11825=CARTESIAN_POINT('Ctrl Pts',(5.91525335839336,-2.87368510266194,7.52676458093347));
#11826=CARTESIAN_POINT('Ctrl Pts',(5.91519240325465,-2.87371604483886,7.52676881240812));
#11827=CARTESIAN_POINT('Ctrl Pts',(5.9151617572847,-2.87373160079465,7.52677093984926));
#11828=CARTESIAN_POINT('Ctrl Pts',(5.91510012389725,-2.87376288478576,7.526775218462));
#11829=CARTESIAN_POINT('Ctrl Pts',(5.91506913648204,-2.87377861280613,7.52677736963376));
#11830=CARTESIAN_POINT('Ctrl Pts',(5.915006815644,-2.87381024319937,7.52678169602523));
#11831=CARTESIAN_POINT('Ctrl Pts',(5.91497548220631,-2.87382614556565,7.52678387124629));
#11832=CARTESIAN_POINT('Ctrl Pts',(5.91491246465541,-2.87385812697718,7.52678824606137));
#11833=CARTESIAN_POINT('Ctrl Pts',(5.91488078054145,-2.87387420600834,7.52679044565577));
#11834=CARTESIAN_POINT('Ctrl Pts',(5.91481705688783,-2.87390654311663,7.52679486954826));
#11835=CARTESIAN_POINT('Ctrl Pts',(5.91478501735916,-2.87392280117334,7.52679709384592));
#11836=CARTESIAN_POINT('Ctrl Pts',(5.9147205781317,-2.8739554986955,7.52680156747532));
#11837=CARTESIAN_POINT('Ctrl Pts',(5.91468817833591,-2.87397193819497,7.52680381681412));
#11838=CARTESIAN_POINT('Ctrl Pts',(5.91462301360079,-2.87400500108034,7.52680834087211));
#11839=CARTESIAN_POINT('Ctrl Pts',(5.91459024874631,-2.87402162440758,7.52681061558574));
#11840=CARTESIAN_POINT('Ctrl Pts',(5.91452434893773,-2.87405505741602,7.5268151907385));
#11841=CARTESIAN_POINT('Ctrl Pts',(5.91449121396325,-2.87407186709156,7.5268174911794));
#11842=CARTESIAN_POINT('Ctrl Pts',(5.91442456887314,-2.87410567530606,7.52682211813778));
#11843=CARTESIAN_POINT('Ctrl Pts',(5.91439105878632,-2.87412267381402,7.52682444465363));
#11844=CARTESIAN_POINT('Ctrl Pts',(5.91432365834847,-2.87415686224275,7.52682912411869));
#11845=CARTESIAN_POINT('Ctrl Pts',(5.91428976800086,-2.874174052145,7.52683147706804));
#11846=CARTESIAN_POINT('Ctrl Pts',(5.9142216018802,-2.87420862592962,7.52683620975957));
#11847=CARTESIAN_POINT('Ctrl Pts',(5.91418732605847,-2.87422600981947,7.52683858950551));
#11848=CARTESIAN_POINT('Ctrl Pts',(5.91411838365043,-2.87426097423532,7.52684337616208));
#11849=CARTESIAN_POINT('Ctrl Pts',(5.91408371712026,-2.8742785547152,7.52684578306921));
#11850=CARTESIAN_POINT('Ctrl Pts',(5.91401398798716,-2.8743139149499,7.52685062441787));
#11851=CARTESIAN_POINT('Ctrl Pts',(5.91397892529484,-2.87433169473196,7.52685305886602));
#11852=CARTESIAN_POINT('Ctrl Pts',(5.91390839834184,-2.87436745630325,7.52685795567954));
#11853=CARTESIAN_POINT('Ctrl Pts',(5.91387293412571,-2.87438543805134,7.52686041804222));
#11854=CARTESIAN_POINT('Ctrl Pts',(5.91380159858358,-2.87442160630858,7.52686537107079));
#11855=CARTESIAN_POINT('Ctrl Pts',(5.91376572723567,-2.87443979280982,7.52686786173863));
#11856=CARTESIAN_POINT('Ctrl Pts',(5.91369357179188,-2.87447637337453,7.5268728717703));
#11857=CARTESIAN_POINT('Ctrl Pts',(5.91365728772179,-2.87449476740542,7.52687539113275));
#11858=CARTESIAN_POINT('Ctrl Pts',(5.9135843010979,-2.87453176587839,7.52688045895323));
#11859=CARTESIAN_POINT('Ctrl Pts',(5.91354759857372,-2.87455037028544,7.52688300740962));
#11860=CARTESIAN_POINT('Ctrl Pts',(5.91347376934107,-2.8745877923401,7.52688813381515));
#11861=CARTESIAN_POINT('Ctrl Pts',(5.91343664250006,-2.87460661003437,7.52689071177393));
#11862=CARTESIAN_POINT('Ctrl Pts',(5.91336195868054,-2.87464446161903,7.52689589759898));
#11863=CARTESIAN_POINT('Ctrl Pts',(5.91332440173229,-2.87466349547306,7.52689850546361));
#11864=CARTESIAN_POINT('Ctrl Pts',(5.91324885164239,-2.874701782383,7.52690375152228));
#11865=CARTESIAN_POINT('Ctrl Pts',(5.91321085854592,-2.87472103539445,7.52690638971367));
#11866=CARTESIAN_POINT('Ctrl Pts',(5.9131344301249,-2.87475976361232,7.52691169684635));
#11867=CARTESIAN_POINT('Ctrl Pts',(5.91309599476147,-2.87477923881632,7.52691436579084));
#11868=CARTESIAN_POINT('Ctrl Pts',(5.9130186756693,-2.87481841446236,7.52691973485741));
#11869=CARTESIAN_POINT('Ctrl Pts',(5.91297979187752,-2.87483811491365,7.52692243498437));
#11870=CARTESIAN_POINT('Ctrl Pts',(5.91290156963042,-2.87487774417691,7.52692786685476));
#11871=CARTESIAN_POINT('Ctrl Pts',(5.91286223115425,-2.87489767297615,7.52693059860015));
#11872=CARTESIAN_POINT('Ctrl Pts',(5.91278309312252,-2.87493776211543,7.52693609415454));
#11873=CARTESIAN_POINT('Ctrl Pts',(5.91274329358416,-2.87495792242288,7.52693885796286));
#11874=CARTESIAN_POINT('Ctrl Pts',(5.91266322700936,-2.87499847775797,7.52694441809044));
#11875=CARTESIAN_POINT('Ctrl Pts',(5.91262295988501,-2.87501887280566,7.52694721441635));
#11876=CARTESIAN_POINT('Ctrl Pts',(5.91254195146517,-2.87505990092728,7.5269528400442));
#11877=CARTESIAN_POINT('Ctrl Pts',(5.91250121027844,-2.875080533921,7.52695566933913));
#11878=CARTESIAN_POINT('Ctrl Pts',(5.91241924706806,-2.87512204123482,7.52696136136963));
#11879=CARTESIAN_POINT('Ctrl Pts',(5.91237802503446,-2.87514291553416,7.52696422410646));
#11880=CARTESIAN_POINT('Ctrl Pts',(5.91229509340215,-2.87518490878858,7.52696998348976));
#11881=CARTESIAN_POINT('Ctrl Pts',(5.91225338377053,-2.87520602773387,7.5269728801391));
#11882=CARTESIAN_POINT('Ctrl Pts',(5.91216947004982,-2.87524851369029,7.52697870782789));
#11883=CARTESIAN_POINT('Ctrl Pts',(5.91212726594579,-2.87526988068185,7.52698163886898));
#11884=CARTESIAN_POINT('Ctrl Pts',(5.91204235630175,-2.8753128661821,7.52698753582775));
#11885=CARTESIAN_POINT('Ctrl Pts',(5.91199965071389,-2.87533448468717,7.52699050174938));
#11886=CARTESIAN_POINT('Ctrl Pts',(5.9119137309574,-2.87537797674735,7.52699646896736));
#11887=CARTESIAN_POINT('Ctrl Pts',(5.91187051682151,-2.87539985025732,7.52699947026206));
#11888=CARTESIAN_POINT('Ctrl Pts',(5.91178357278943,-2.87544385587524,7.52700550872677));
#11889=CARTESIAN_POINT('Ctrl Pts',(5.91173984283814,-2.87546598798174,7.52700854590125));
#11890=CARTESIAN_POINT('Ctrl Pts',(5.91165185983416,-2.87551051441975,7.52701465663737));
#11891=CARTESIAN_POINT('Ctrl Pts',(5.91160760679998,-2.87553290871179,7.52701773019839));
#11892=CARTESIAN_POINT('Ctrl Pts',(5.91152199272508,-2.87557623131725,7.5270236765146));
#11893=CARTESIAN_POINT('Ctrl Pts',(5.91148063168748,-2.87559715979139,7.52702654926596));
#11894=CARTESIAN_POINT('Ctrl Pts',(5.90442868615588,-2.8791652171741,7.52751634990232));
#11895=CARTESIAN_POINT('Ctrl Pts',(5.89740538435486,-2.88268658207869,7.52800489810312));
#11896=CARTESIAN_POINT('Ctrl Pts',(5.88132808729335,-2.89067403331396,7.52912488672838));
#11897=CARTESIAN_POINT('Ctrl Pts',(5.87226594297745,-2.89512327775316,7.52975734441413));
#11898=CARTESIAN_POINT('Ctrl Pts',(5.84808164591235,-2.90685634952692,7.53144798854324));
#11899=CARTESIAN_POINT('Ctrl Pts',(5.83292346582989,-2.91406462960333,7.5325105400672));
#11900=CARTESIAN_POINT('Ctrl Pts',(5.7006482605295,-2.9757041137638,7.54180335861236));
#11901=CARTESIAN_POINT('Ctrl Pts',(5.5804255078002,-3.02316247948295,7.55038537350614));
#11902=CARTESIAN_POINT('Ctrl Pts',(5.27968466108615,-3.12145907507314,7.57167483474776));
#11903=CARTESIAN_POINT('Ctrl Pts',(5.09692751588153,-3.16401822938152,7.58444290431546));
#11904=CARTESIAN_POINT('Ctrl Pts',(4.82108046907848,-3.2033605936835,7.60292190032956));
#11905=CARTESIAN_POINT('Ctrl Pts',(4.73014240208535,-3.21240810900902,7.60889424641218));
#11906=CARTESIAN_POINT('Ctrl Pts',(4.5989436049025,-3.2198483055755,7.61732455134665));
#11907=CARTESIAN_POINT('Ctrl Pts',(4.55891111003898,-3.22137050923549,7.6198723556987));
#11908=CARTESIAN_POINT('Ctrl Pts',(4.48704260334128,-3.22276209130484,7.62440318758332));
#11909=CARTESIAN_POINT('Ctrl Pts',(4.45521778407727,-3.22290688458961,7.62639438847226));
#11910=CARTESIAN_POINT('Ctrl Pts',(4.40654629590824,-3.22240735903025,7.62941741368368));
#11911=CARTESIAN_POINT('Ctrl Pts',(4.38969885983033,-3.22210229911656,7.63045975220696));
#11912=CARTESIAN_POINT('Ctrl Pts',(4.35905913390518,-3.22130707872627,7.63234823771107));
#11913=CARTESIAN_POINT('Ctrl Pts',(4.34526621214669,-3.22086043222862,7.63319572265086));
#11914=CARTESIAN_POINT('Ctrl Pts',(4.31520614677569,-3.21969369026665,7.63503713135469));
#11915=CARTESIAN_POINT('Ctrl Pts',(4.29894067307012,-3.21893887652395,7.6360299473));
#11916=CARTESIAN_POINT('Ctrl Pts',(4.25437073889694,-3.21653192777853,7.63874106001821));
#11917=CARTESIAN_POINT('Ctrl Pts',(4.22608084949324,-3.2146294842955,7.64045152062713));
#11918=CARTESIAN_POINT('Ctrl Pts',(4.06960495898306,-3.20203046835265,7.64986036240773));
#11919=CARTESIAN_POINT('Ctrl Pts',(3.94211569634664,-3.18403973880444,7.65732633446367));
#11920=CARTESIAN_POINT('Ctrl Pts',(3.59907319593254,-3.11448164008162,7.67725560294875));
#11921=CARTESIAN_POINT('Ctrl Pts',(3.38723747971508,-3.04825535591424,7.6893597258122));
#11922=CARTESIAN_POINT('Ctrl Pts',(3.08691799803865,-2.91917508021386,7.70801264061929));
#11923=CARTESIAN_POINT('Ctrl Pts',(2.99208253731074,-2.87277229552128,7.71415091209754));
#11924=CARTESIAN_POINT('Ctrl Pts',(2.88455813027404,-2.81345209126844,7.72159702695786));
#11925=CARTESIAN_POINT('Ctrl Pts',(2.86948000446817,-2.80497457150385,7.72265275069675));
#11926=CARTESIAN_POINT('Ctrl Pts',(2.8464026799731,-2.791753952857,7.72428754469633));
#11927=CARTESIAN_POINT('Ctrl Pts',(2.83835428256579,-2.787096776688,7.72486127794301));
#11928=CARTESIAN_POINT('Ctrl Pts',(2.82356738299414,-2.77845475238457,7.72592220226524));
#11929=CARTESIAN_POINT('Ctrl Pts',(2.81682314219335,-2.77448012380268,7.72640873909922));
#11930=CARTESIAN_POINT('Ctrl Pts',(2.80155849066583,-2.76540900899988,7.72751596400573));
#11931=CARTESIAN_POINT('Ctrl Pts',(2.79304715648399,-2.76029772733014,7.72813759138408));
#11932=CARTESIAN_POINT('Ctrl Pts',(2.77100103982271,-2.74691945536921,7.72975854261043));
#11933=CARTESIAN_POINT('Ctrl Pts',(2.75750360660644,-2.73859184703327,7.7307615956832));
#11934=CARTESIAN_POINT('Ctrl Pts',(2.66592016021447,-2.68114933368016,7.73763754250189));
#11935=CARTESIAN_POINT('Ctrl Pts',(2.58991955152757,-2.62880519832061,7.74369153494054));
#11936=CARTESIAN_POINT('Ctrl Pts',(2.45029939372569,-2.52353484522955,7.75534358972921));
#11937=CARTESIAN_POINT('Ctrl Pts',(2.3862622701084,-2.47127251457562,7.76091947144446));
#11938=CARTESIAN_POINT('Ctrl Pts',(2.22491934130544,-2.32892041412423,7.77547060486515));
#11939=CARTESIAN_POINT('Ctrl Pts',(2.13103174148922,-2.2351798280881,7.78444642351581));
#11940=CARTESIAN_POINT('Ctrl Pts',(1.97822316920715,-2.06252772218843,7.79978315762799));
#11941=CARTESIAN_POINT('Ctrl Pts',(1.9166431221908,-1.98620502305204,7.80620995802105));
#11942=CARTESIAN_POINT('Ctrl Pts',(1.83377796619093,-1.87333199146408,7.81520790277436));
#11943=CARTESIAN_POINT('Ctrl Pts',(1.80958614019447,-1.83899222202472,7.81788285931309));
#11944=CARTESIAN_POINT('Ctrl Pts',(1.76757732791114,-1.77681454085119,7.82261699510284));
#11945=CARTESIAN_POINT('Ctrl Pts',(1.74950455849487,-1.74915750459717,7.82468544725825));
#11946=CARTESIAN_POINT('Ctrl Pts',(1.72272723230812,-1.70677043338548,7.82780048587873));
#11947=CARTESIAN_POINT('Ctrl Pts',(1.71370983839016,-1.69224157915713,7.82885859756701));
#11948=CARTESIAN_POINT('Ctrl Pts',(1.69755052014457,-1.66573712999991,7.83077173601058));
#11949=CARTESIAN_POINT('Ctrl Pts',(1.6903699147922,-1.65378572485089,7.83162816576033));
#11950=CARTESIAN_POINT('Ctrl Pts',(1.67505134751849,-1.62791059094059,7.83346912942253));
#11951=CARTESIAN_POINT('Ctrl Pts',(1.66693985842808,-1.61397157069171,7.8344526860514));
#11952=CARTESIAN_POINT('Ctrl Pts',(1.64519805344523,-1.57595623186843,7.83711340459795));
#11953=CARTESIAN_POINT('Ctrl Pts',(1.63177239035655,-1.55176400028695,7.83878321308081));
#11954=CARTESIAN_POINT('Ctrl Pts',(1.56347530074076,-1.42487257312192,7.84742519107584));
#11955=CARTESIAN_POINT('Ctrl Pts',(1.51388445119901,-1.31942215157096,7.85420960525952));
#11956=CARTESIAN_POINT('Ctrl Pts',(1.38368678183428,-0.9984857233354,7.87401250631363));
#11957=CARTESIAN_POINT('Ctrl Pts',(1.3203121997983,-0.776839055453567,7.88656885806303));
#11958=CARTESIAN_POINT('Ctrl Pts',(1.26223768874595,-0.441756111965293,
7.90593875558007));
#11959=CARTESIAN_POINT('Ctrl Pts',(1.24900235386584,-0.33228689170426,7.9123361068974));
#11960=CARTESIAN_POINT('Ctrl Pts',(1.24019546835171,-0.204954002497827,
7.92007381077273));
#11961=CARTESIAN_POINT('Ctrl Pts',(1.23913257910733,-0.187531056072594,
7.92113897962062));
#11962=CARTESIAN_POINT('Ctrl Pts',(1.2377187398344,-0.160781624375865,7.92278535130385));
#11963=CARTESIAN_POINT('Ctrl Pts',(1.23726666439664,-0.151460507343538,
7.9233610982383));
#11964=CARTESIAN_POINT('Ctrl Pts',(1.23650991752259,-0.134319151317417,
7.92442387195206));
#11965=CARTESIAN_POINT('Ctrl Pts',(1.23619324114858,-0.126499645035582,
7.92491022724559));
#11966=CARTESIAN_POINT('Ctrl Pts',(1.23554097158206,-0.10879916617651,7.92601463282506));
#11967=CARTESIAN_POINT('Ctrl Pts',(1.23522236523769,-0.0989178178291134,
7.92663360166204));
#11968=CARTESIAN_POINT('Ctrl Pts',(1.23451489317406,-0.0733197131773398,
7.92824309285351));
#11969=CARTESIAN_POINT('Ctrl Pts',(1.23419556495815,-0.0576015065964676,
7.92923726057324));
#11970=CARTESIAN_POINT('Ctrl Pts',(1.23283769636146,0.0468754824732806,
7.93588165931194));
#11971=CARTESIAN_POINT('Ctrl Pts',(1.23535174813176,0.135634740869622,7.94169968024144));
#11972=CARTESIAN_POINT('Ctrl Pts',(1.26132431000045,0.508124649788423,7.96655106455441));
#11973=CARTESIAN_POINT('Ctrl Pts',(1.3186644953888,0.788266175328424,7.98616575056507));
#11974=CARTESIAN_POINT('Ctrl Pts',(1.4413368717694,1.14151496394501,8.01051003475562));
#11975=CARTESIAN_POINT('Ctrl Pts',(1.47409728168568,1.22455689598729,8.01621672730507));
#11976=CARTESIAN_POINT('Ctrl Pts',(1.5203274404603,1.32883637393786,8.02336502965246));
#11977=CARTESIAN_POINT('Ctrl Pts',(1.53065206413788,1.35141728633027,8.02491195998822));
#11978=CARTESIAN_POINT('Ctrl Pts',(1.54777897483766,1.38775890729739,8.02740052833206));
#11979=CARTESIAN_POINT('Ctrl Pts',(1.55442026339144,1.4015939469134,8.02834766363145));
#11980=CARTESIAN_POINT('Ctrl Pts',(1.56734123721506,1.42802513734399,8.03015683888255));
#11981=CARTESIAN_POINT('Ctrl Pts',(1.57360509450719,1.44062859066464,8.03101940235089));
#11982=CARTESIAN_POINT('Ctrl Pts',(1.58810281202865,1.4693260901403,8.03298334545138));
#11983=CARTESIAN_POINT('Ctrl Pts',(1.59638997514467,1.4853927902967,8.0340828310382));
#11984=CARTESIAN_POINT('Ctrl Pts',(1.6230067431694,1.53594723462193,8.03754293156664));
#11985=CARTESIAN_POINT('Ctrl Pts',(1.64182870891379,1.57017276203312,8.03988617000821));
#11986=CARTESIAN_POINT('Ctrl Pts',(1.79223939164411,1.83227699111076,8.05785837035122));
#11987=CARTESIAN_POINT('Ctrl Pts',(1.95066497013704,2.04360432280226,8.07240389583344));
#11988=CARTESIAN_POINT('Ctrl Pts',(2.21698782117833,2.32067176489093,8.09394482351849));
#11989=CARTESIAN_POINT('Ctrl Pts',(2.30579273130685,2.40320218412119,8.10077976953727));
#11990=CARTESIAN_POINT('Ctrl Pts',(2.4293382507474,2.50567539337132,8.11016519909149));
#11991=CARTESIAN_POINT('Ctrl Pts',(2.46010912082101,2.53025991095954,8.11249365982654));
#11992=CARTESIAN_POINT('Ctrl Pts',(2.51287651295211,2.57085686763634,8.1164860939486));
#11993=CARTESIAN_POINT('Ctrl Pts',(2.53463990663532,2.58716632998767,8.11813259316799));
#11994=CARTESIAN_POINT('Ctrl Pts',(2.5656150363775,2.6097725637616,8.12047987779021));
#11995=CARTESIAN_POINT('Ctrl Pts',(2.57465771893149,2.61630041129315,8.12116558733931));
#11996=CARTESIAN_POINT('Ctrl Pts',(2.59023089661888,2.6274200726489,8.12234763207773));
#11997=CARTESIAN_POINT('Ctrl Pts',(2.5967450034474,2.63203486937701,8.12284240796897));
#11998=CARTESIAN_POINT('Ctrl Pts',(2.60945017514427,2.64096489562136,8.12380820106755));
#11999=CARTESIAN_POINT('Ctrl Pts',(2.61563930681297,2.6452826235604,8.12427901506673));
#12000=CARTESIAN_POINT('Ctrl Pts',(2.63261176668727,2.65703472289611,8.12557093494879));
#12001=CARTESIAN_POINT('Ctrl Pts',(2.64342520256819,2.66442506055483,8.12639492415659));
#12002=CARTESIAN_POINT('Ctrl Pts',(2.68557725377455,2.69285805718569,8.12960941123526));
#12003=CARTESIAN_POINT('Ctrl Pts',(2.71723824940221,2.71341449249602,8.13202912134047));
#12004=CARTESIAN_POINT('Ctrl Pts',(2.9342345175239,2.84894484384315,8.14861014994374));
#12005=CARTESIAN_POINT('Ctrl Pts',(3.13045713424751,2.94539784774797,8.16354602207032));
#12006=CARTESIAN_POINT('Ctrl Pts',(3.46421289675029,3.06929472137217,8.18753027230061));
#12007=CARTESIAN_POINT('Ctrl Pts',(3.59648062561646,3.10894986088775,8.19671114121583));
#12008=CARTESIAN_POINT('Ctrl Pts',(3.80764083140854,3.15774347995749,8.21075221561559));
#12009=CARTESIAN_POINT('Ctrl Pts',(3.88501603441871,3.17265899957625,8.21577357468115));
#12010=CARTESIAN_POINT('Ctrl Pts',(3.98640183300925,3.18837287213575,8.22219696813252));
#12011=CARTESIAN_POINT('Ctrl Pts',(4.00997804591508,3.19175979595857,8.22367985372211));
#12012=CARTESIAN_POINT('Ctrl Pts',(4.04858499230612,3.19686985914933,8.22609098274487));
#12013=CARTESIAN_POINT('Ctrl Pts',(4.06359381253402,3.19874903091438,8.22702411003635));
#12014=CARTESIAN_POINT('Ctrl Pts',(4.09266808050719,3.20218153814956,8.22882373855212));
#12015=CARTESIAN_POINT('Ctrl Pts',(4.10673159485959,3.20374803516124,8.22969063431562));
#12016=CARTESIAN_POINT('Ctrl Pts',(4.13927872823666,3.20715650421183,8.23168877857485));
#12017=CARTESIAN_POINT('Ctrl Pts',(4.1577689783552,3.20893141627922,8.23281789943001));
#12018=CARTESIAN_POINT('Ctrl Pts',(4.21793631374609,3.21418242347375,8.23647324008585));
#12019=CARTESIAN_POINT('Ctrl Pts',(4.25966696016786,3.21700725859855,8.23897911424938));
#12020=CARTESIAN_POINT('Ctrl Pts',(4.50190175096816,3.22867320150942,8.25337507169849));
#12021=CARTESIAN_POINT('Ctrl Pts',(4.70283233463573,3.21958265723146,8.26468506574211));
#12022=CARTESIAN_POINT('Ctrl Pts',(5.11079804496556,3.16268445186581,8.28773024144073));
#12023=CARTESIAN_POINT('Ctrl Pts',(5.31656451498272,3.11302629196946,8.29941041425671));
#12024=CARTESIAN_POINT('Ctrl Pts',(5.54696446468353,3.03282290172023,8.31396256820595));
#12025=CARTESIAN_POINT('Ctrl Pts',(5.57779452658766,3.02155986071374,8.31594218524855));
#12026=CARTESIAN_POINT('Ctrl Pts',(5.61966022357567,3.00553625378433,8.31868178756917));
#12027=CARTESIAN_POINT('Ctrl Pts',(5.63085035083276,3.00118150568075,8.31941911094992));
#12028=CARTESIAN_POINT('Ctrl Pts',(5.64959024471379,2.99376783750807,8.32066282950014));
#12029=CARTESIAN_POINT('Ctrl Pts',(5.65715335538297,2.99074259131064,8.32116723011931));
#12030=CARTESIAN_POINT('Ctrl Pts',(5.6715163033913,2.98493414579692,8.32212995161071));
#12031=CARTESIAN_POINT('Ctrl Pts',(5.67831823436919,2.98215630904535,8.32258793389401));
#12032=CARTESIAN_POINT('Ctrl Pts',(5.69445694871588,2.97550094534822,8.32367937508729));
#12033=CARTESIAN_POINT('Ctrl Pts',(5.70378503718952,2.97160272174388,8.32431405417834));
#12034=CARTESIAN_POINT('Ctrl Pts',(5.73666564368688,2.95767976753859,8.32656440058392));
#12035=CARTESIAN_POINT('Ctrl Pts',(5.76011621206759,2.94741868593203,8.32819329414516));
#12036=CARTESIAN_POINT('Ctrl Pts',(5.97573646161604,2.84999486250812,8.34337631647785));
#12037=CARTESIAN_POINT('Ctrl Pts',(6.15901774324404,2.74444139178069,8.35776824686605));
#12038=CARTESIAN_POINT('Ctrl Pts',(6.5143542283234,2.49042519431466,8.38727555731693));
#12039=CARTESIAN_POINT('Ctrl Pts',(6.68377496669091,2.3401394133331,8.40227131845801));
#12040=CARTESIAN_POINT('Ctrl Pts',(6.85747211421996,2.14995478200649,8.41850437641143));
#12041=CARTESIAN_POINT('Ctrl Pts',(6.87848903416943,2.12625035985636,8.42048632743801));
#12042=CARTESIAN_POINT('Ctrl Pts',(6.91012524069904,2.08949085486792,8.42349831389009));
#12043=CARTESIAN_POINT('Ctrl Pts',(6.92099701478286,2.07665660712555,8.42453874523332));
#12044=CARTESIAN_POINT('Ctrl Pts',(6.94060418750484,2.05313927056341,8.42642523986893));
#12045=CARTESIAN_POINT('Ctrl Pts',(6.94937234057136,2.04248413456387,8.42727262684278));
#12046=CARTESIAN_POINT('Ctrl Pts',(6.96835372211582,2.01911347263982,8.42911551416144));
#12047=CARTESIAN_POINT('Ctrl Pts',(6.97853944706148,2.00637602410008,8.43010989376353));
#12048=CARTESIAN_POINT('Ctrl Pts',(7.00623826510674,1.97119385912471,8.43282953838485));
#12049=CARTESIAN_POINT('Ctrl Pts',(7.02355159699357,1.9485932253829,8.43454688414816));
#12050=CARTESIAN_POINT('Ctrl Pts',(7.11876933368087,1.82082501074837,8.44409646428369));
#12051=CARTESIAN_POINT('Ctrl Pts',(7.1905151353312,1.71121134777246,8.45168749756149));
#12052=CARTESIAN_POINT('Ctrl Pts',(7.36420963234959,1.40689148490349,8.47162362218473));
#12053=CARTESIAN_POINT('Ctrl Pts',(7.45325094019838,1.20564944144229,8.48362897184219));
#12054=CARTESIAN_POINT('Ctrl Pts',(7.54309826241073,0.929447941818175,8.50020645125321));
#12055=CARTESIAN_POINT('Ctrl Pts',(7.56281332800213,0.861264970790674,8.504310451108));
#12056=CARTESIAN_POINT('Ctrl Pts',(7.58715373160293,0.765321537309864,8.51017070011551));
#12057=CARTESIAN_POINT('Ctrl Pts',(7.59369160941581,0.738063774908442,8.51184510428537));
#12058=CARTESIAN_POINT('Ctrl Pts',(7.60449467943694,0.690283827154938,8.51480219077887));
#12059=CARTESIAN_POINT('Ctrl Pts',(7.60891683439086,0.66979850714309,8.51607704978918));
#12060=CARTESIAN_POINT('Ctrl Pts',(7.61516187107677,0.639436018637407,8.51797892254679));
#12061=CARTESIAN_POINT('Ctrl Pts',(7.61713897306658,0.629590653664814,8.51859753561515));
#12062=CARTESIAN_POINT('Ctrl Pts',(7.62057693334679,0.61204626401379,8.51970355782792));
#12063=CARTESIAN_POINT('Ctrl Pts',(7.62205576479485,0.604350954379263,8.52018994162952));
#12064=CARTESIAN_POINT('Ctrl Pts',(7.62521206953694,0.58759719240185,8.52125166951141));
#12065=CARTESIAN_POINT('Ctrl Pts',(7.62687874837235,0.578537055053457,8.5218275876985));
#12066=CARTESIAN_POINT('Ctrl Pts',(7.63140984296587,0.553298147141996,8.52343657092831));
#12067=CARTESIAN_POINT('Ctrl Pts',(7.63418936528196,0.537104691961789,8.52447420680797));
#12068=CARTESIAN_POINT('Ctrl Pts',(7.64896042166707,0.446917874928872,8.53027994021497));
#12069=CARTESIAN_POINT('Ctrl Pts',(7.65849043901687,0.372550488443372,8.53516703147698));
#12070=CARTESIAN_POINT('Ctrl Pts',(7.66699191607319,0.280981187684177,8.54125397867788));
#12071=CARTESIAN_POINT('Ctrl Pts',(7.66843079228126,0.26402509759489,8.54238404061981));
#12072=CARTESIAN_POINT('Ctrl Pts',(7.67598553012433,0.165767519409022,8.54894685044929));
#12073=CARTESIAN_POINT('Ctrl Pts',(7.67914849102628,0.0842710249388068,
8.55444595359864));
#12074=CARTESIAN_POINT('Ctrl Pts',(7.67921871651019,0.0018301419827333,
8.56002040187424));
#12075=CARTESIAN_POINT('Ctrl Pts',(7.67921910621818,0.000915065319246332,
8.5600822786385));
#12076=CARTESIAN_POINT('Ctrl Pts',(7.67921910621823,1.63241365473312E-10,
8.56014415614755));
#12077=CARTESIAN_POINT('Ctrl Pts',(7.67921910621823,-4.32286151319516E-11,
8.31612808864259));
#12078=CARTESIAN_POINT('Ctrl Pts',(7.67921910622028,0.152894774448002,8.30592674797713));
#12079=CARTESIAN_POINT('Ctrl Pts',(7.6683387014842,0.305598992240482,8.29551152918883));
#12080=CARTESIAN_POINT('Ctrl Pts',(7.6272739193954,0.592287328368467,8.27600540816731));
#12081=CARTESIAN_POINT('Ctrl Pts',(7.59929648326779,0.726257753529316,8.26690949802179));
#12082=CARTESIAN_POINT('Ctrl Pts',(7.54203676515252,0.933554726933015,8.25297924861768));
#12083=CARTESIAN_POINT('Ctrl Pts',(7.51843640605665,1.00827087518957,8.24798693863413));
#12084=CARTESIAN_POINT('Ctrl Pts',(7.48415433602558,1.10444768529297,8.24159465152635));
#12085=CARTESIAN_POINT('Ctrl Pts',(7.4759260392699,1.12674860479593,8.24011479010671));
#12086=CARTESIAN_POINT('Ctrl Pts',(7.46206317765897,1.1630779327418,8.23770738401184));
#12087=CARTESIAN_POINT('Ctrl Pts',(7.45657542378966,1.17716103214207,8.23677498330327));
#12088=CARTESIAN_POINT('Ctrl Pts',(7.44575760007654,1.20435549483327,8.23497594434296));
#12089=CARTESIAN_POINT('Ctrl Pts',(7.44043984567187,1.21747135227674,8.23410891757477));
#12090=CARTESIAN_POINT('Ctrl Pts',(7.4279349260634,1.24773967039451,8.23210930921201));
#12091=CARTESIAN_POINT('Ctrl Pts',(7.42068530394154,1.26486590561796,8.23097886625832));
#12092=CARTESIAN_POINT('Ctrl Pts',(7.39659943288182,1.32042090748783,8.22731422220286));
#12093=CARTESIAN_POINT('Ctrl Pts',(7.3791605492576,1.35858480921884,8.22480051620933));
#12094=CARTESIAN_POINT('Ctrl Pts',(7.27274319629282,1.57993308830166,8.2102227037136));
#12095=CARTESIAN_POINT('Ctrl Pts',(7.1673059260598,1.75469793342222,8.19875771206775));
#12096=CARTESIAN_POINT('Ctrl Pts',(6.95438750816694,2.04211719908581,8.17874959744835));
#12097=CARTESIAN_POINT('Ctrl Pts',(6.85395957507722,2.15913700917035,8.17018921603032));
#12098=CARTESIAN_POINT('Ctrl Pts',(6.70845988300255,2.30595594055005,8.15824427225181));
#12099=CARTESIAN_POINT('Ctrl Pts',(6.6704504084308,2.34247336420976,8.15515993018695));
#12100=CARTESIAN_POINT('Ctrl Pts',(6.6146693449649,2.39349400703087,8.15065443385224));
#12101=CARTESIAN_POINT('Ctrl Pts',(6.59761017182726,2.4087666361266,8.14927923258981));
#12102=CARTESIAN_POINT('Ctrl Pts',(6.5707670866307,2.43228808361965,8.1471167813232));
#12103=CARTESIAN_POINT('Ctrl Pts',(6.56109399440802,2.44066288939511,8.14633781778985));
#12104=CARTESIAN_POINT('Ctrl Pts',(6.54311147480594,2.4560454679067,8.14488968315624));
#12105=CARTESIAN_POINT('Ctrl Pts',(6.53481592518202,2.46306926557597,8.14422163290536));
#12106=CARTESIAN_POINT('Ctrl Pts',(6.52040969160513,2.475142350857,8.14306114787766));
#12107=CARTESIAN_POINT('Ctrl Pts',(6.51431552608102,2.48021138365959,8.14257013286076));
#12108=CARTESIAN_POINT('Ctrl Pts',(6.50249414975144,2.4899706589433,8.14161733695782));
#12109=CARTESIAN_POINT('Ctrl Pts',(6.49676939396589,2.49466372370422,8.14115578426719));
#12110=CARTESIAN_POINT('Ctrl Pts',(6.48302091996156,2.50585552717981,8.14004709731872));
#12111=CARTESIAN_POINT('Ctrl Pts',(6.47498209743747,2.51233546214467,8.1393986545137));
#12112=CARTESIAN_POINT('Ctrl Pts',(6.44583006920326,2.53560410015474,8.13704689884219));
#12113=CARTESIAN_POINT('Ctrl Pts',(6.42453808279569,2.55216566599599,8.13532878378228));
#12114=CARTESIAN_POINT('Ctrl Pts',(6.27208697801919,2.66770471378783,8.12303870143831));
#12115=CARTESIAN_POINT('Ctrl Pts',(6.13374605277013,2.75678226366342,8.11195887552769));
#12116=CARTESIAN_POINT('Ctrl Pts',(5.8497801566302,2.91031511352275,8.09012365574392));
#12117=CARTESIAN_POINT('Ctrl Pts',(5.7049431817029,2.9753267497044,8.07940108838415));
#12118=CARTESIAN_POINT('Ctrl Pts',(5.44322473042737,3.07030928418576,8.06104957621094));
#12119=CARTESIAN_POINT('Ctrl Pts',(5.32834455960816,3.10488724798534,8.05331454530127));
#12120=CARTESIAN_POINT('Ctrl Pts',(5.18543114207754,3.13934184155351,8.04408339348481));
#12121=CARTESIAN_POINT('Ctrl Pts',(5.15899048265322,3.14536430890173,8.04239134876867));
#12122=CARTESIAN_POINT('Ctrl Pts',(5.11698346033278,3.15437623401253,8.03972749817557));
#12123=CARTESIAN_POINT('Ctrl Pts',(5.10146610631022,3.15758571093394,8.03874870381919));
#12124=CARTESIAN_POINT('Ctrl Pts',(5.072225475103,3.16340904581196,8.03691389956197));
#12125=CARTESIAN_POINT('Ctrl Pts',(5.05850770076668,3.16604836307615,8.03605709713987));
#12126=CARTESIAN_POINT('Ctrl Pts',(5.02758159219517,3.17179031847486,8.03413419705184));
#12127=CARTESIAN_POINT('Ctrl Pts',(5.01036420957287,3.17484228415048,8.03306973028545));
#12128=CARTESIAN_POINT('Ctrl Pts',(4.96618270092223,3.18230357902081,8.03035320643503));
#12129=CARTESIAN_POINT('Ctrl Pts',(4.939185466422,3.18651047422589,8.02870754946587));
#12130=CARTESIAN_POINT('Ctrl Pts',(4.70087441575128,3.22054748427962,8.01429858010636));
#12131=CARTESIAN_POINT('Ctrl Pts',(4.48712808632995,3.22966504285192,8.00223656807286));
#12132=CARTESIAN_POINT('Ctrl Pts',(4.10348530604978,3.20791170107139,7.98073046126447));
#12133=CARTESIAN_POINT('Ctrl Pts',(3.93399610626441,3.18469916452879,7.97126329965214));
#12134=CARTESIAN_POINT('Ctrl Pts',(3.72058703479672,3.13797195970881,7.95858633430621));
#12135=CARTESIAN_POINT('Ctrl Pts',(3.67424988293245,3.12674320585354,7.95578607917916));
#12136=CARTESIAN_POINT('Ctrl Pts',(3.59787452101686,3.1064314512102,7.95106567799243));
#12137=CARTESIAN_POINT('Ctrl Pts',(3.56768833987926,3.09792989033976,7.94917246547854));
#12138=CARTESIAN_POINT('Ctrl Pts',(3.52632540868807,3.08562626099909,7.94653413009217));
#12139=CARTESIAN_POINT('Ctrl Pts',(3.51503724998766,3.08220096208138,7.94580955543328));
#12140=CARTESIAN_POINT('Ctrl Pts',(3.49602794043152,3.07631857596444,7.94458126721166));
#12141=CARTESIAN_POINT('Ctrl Pts',(3.48829665050208,3.07389416015902,7.94407943867261));
#12142=CARTESIAN_POINT('Ctrl Pts',(3.47353393773413,3.06920357631316,7.94311672195272));
#12143=CARTESIAN_POINT('Ctrl Pts',(3.4665010388713,3.06694234724588,7.94265614161233));
#12144=CARTESIAN_POINT('Ctrl Pts',(3.44779319335072,3.06085631805267,7.9414259060653));
#12145=CARTESIAN_POINT('Ctrl Pts',(3.43613237391788,3.05698894964509,7.94065381460934));
#12146=CARTESIAN_POINT('Ctrl Pts',(3.39402305271583,3.04275541544234,7.93784727361805));
#12147=CARTESIAN_POINT('Ctrl Pts',(3.36370915505603,3.03200060045672,7.93579200578562));
#12148=CARTESIAN_POINT('Ctrl Pts',(3.01051345801012,2.90070873838357,7.91147604308592));
#12149=CARTESIAN_POINT('Ctrl Pts',(2.70880247699491,2.72958178960875,7.8873621280405));
#12150=CARTESIAN_POINT('Ctrl Pts',(2.39089588386221,2.47456491838673,7.86076337936925));
#12151=CARTESIAN_POINT('Ctrl Pts',(2.34304904065818,2.43382841231113,7.8567120042757));
#12152=CARTESIAN_POINT('Ctrl Pts',(2.26291194355601,2.36145363289537,7.84984302497023));
#12153=CARTESIAN_POINT('Ctrl Pts',(2.23004130218746,2.3304883289731,7.84699966567669));
#12154=CARTESIAN_POINT('Ctrl Pts',(2.18402482035561,2.28527659908884,7.84297963478266));
#12155=CARTESIAN_POINT('Ctrl Pts',(2.17034103651119,2.27158769185718,7.84177900504115));
#12156=CARTESIAN_POINT('Ctrl Pts',(2.14681666123005,2.24762662576877,7.83970552878154));
#12157=CARTESIAN_POINT('Ctrl Pts',(2.13691933887628,2.23741117201143,7.83883020218593));
#12158=CARTESIAN_POINT('Ctrl Pts',(2.11675196397681,2.21631790107348,7.83704029090279));
#12159=CARTESIAN_POINT('Ctrl Pts',(2.10648936097224,2.2054334161559,7.83612603975568));
#12160=CARTESIAN_POINT('Ctrl Pts',(2.08060539129778,2.17759514147273,7.83381110847673));
#12161=CARTESIAN_POINT('Ctrl Pts',(2.06508929793362,2.16054429412465,7.83241492081288));
#12162=CARTESIAN_POINT('Ctrl Pts',(2.00618139749804,2.0943974695644,7.82707921742073));
#12163=CARTESIAN_POINT('Ctrl Pts',(1.96410594502064,2.04414710025331,7.82319413091853));
#12164=CARTESIAN_POINT('Ctrl Pts',(1.71685983785065,1.72986920957065,7.79980321937745));
#12165=CARTESIAN_POINT('Ctrl Pts',(1.55230942071272,1.43656660179051,7.78199074100371));
#12166=CARTESIAN_POINT('Ctrl Pts',(1.41949591364359,1.07939759052762,7.7598613866478));
#12167=CARTESIAN_POINT('Ctrl Pts',(1.40415087593605,1.03520931207224,7.75711219847908));
#12168=CARTESIAN_POINT('Ctrl Pts',(1.38026803102447,0.961280735814901,7.75246992716725));
#12169=CARTESIAN_POINT('Ctrl Pts',(1.37118679470257,0.931722386840167,7.75060265233535));
#12170=CARTESIAN_POINT('Ctrl Pts',(1.35924892011026,0.890776244890207,7.74799477134266));
#12171=CARTESIAN_POINT('Ctrl Pts',(1.3560267805261,0.879495636640035,7.74727409880327));
#12172=CARTESIAN_POINT('Ctrl Pts',(1.35068700399735,0.86040719462833,7.7460505038462));
#12173=CARTESIAN_POINT('Ctrl Pts',(1.34853700450162,0.852608383955271,7.74554943316304));
#12174=CARTESIAN_POINT('Ctrl Pts',(1.34447629307104,0.837659280509856,7.74458660697104));
#12175=CARTESIAN_POINT('Ctrl Pts',(1.34256081524545,0.830510380490131,7.74412514953906));
#12176=CARTESIAN_POINT('Ctrl Pts',(1.33803347506568,0.813377695398469,7.74301691408169));
#12177=CARTESIAN_POINT('Ctrl Pts',(1.33544492848741,0.803387911429119,7.74236882982181));
#12178=CARTESIAN_POINT('Ctrl Pts',(1.32627397301453,0.767281815049695,7.74002007194676));
#12179=CARTESIAN_POINT('Ctrl Pts',(1.31997124311823,0.741096485203178,7.73830464541641));
#12180=CARTESIAN_POINT('Ctrl Pts',(1.27651707821088,0.550068861059934,7.72571811881177));
#12181=CARTESIAN_POINT('Ctrl Pts',(1.25205672688252,0.38262409411107,7.71431011086639));
#12182=CARTESIAN_POINT('Ctrl Pts',(1.23093908259382,0.0653811834219913,
7.69280154349986));
#12183=CARTESIAN_POINT('Ctrl Pts',(1.23136434704622,-0.0838073757847299,
7.68272999060841));
#12184=CARTESIAN_POINT('Ctrl Pts',(1.2510776512479,-0.356419311215628,7.66468579819657));
#12185=CARTESIAN_POINT('Ctrl Pts',(1.26720923235708,-0.479788574623397,
7.65665459465783));
#12186=CARTESIAN_POINT('Ctrl Pts',(1.2955451970621,-0.62883011445333,7.64712597316299));
#12187=CARTESIAN_POINT('Ctrl Pts',(1.30100198708793,-0.655663485905089,
7.64541712858252));
#12188=CARTESIAN_POINT('Ctrl Pts',(1.3101677163521,-0.697967069935794,7.64273301119939));
#12189=CARTESIAN_POINT('Ctrl Pts',(1.31365024797686,-0.713484481510536,
7.64175056816355));
#12190=CARTESIAN_POINT('Ctrl Pts',(1.32040566715821,-0.742575653386324,
7.6399125198569));
#12191=CARTESIAN_POINT('Ctrl Pts',(1.32365216819928,-0.756155101401115,
7.63905609256234));
#12192=CARTESIAN_POINT('Ctrl Pts',(1.33114260867385,-0.786609562489644,
7.63713869280799));
#12193=CARTESIAN_POINT('Ctrl Pts',(1.33543519358248,-0.803472248869386,
7.63607931089189));
#12194=CARTESIAN_POINT('Ctrl Pts',(1.34674681179853,-0.846449040028402,
7.63338468513084));
#12195=CARTESIAN_POINT('Ctrl Pts',(1.35395840339334,-0.872511393424122,
7.63175566390866));
#12196=CARTESIAN_POINT('Ctrl Pts',(1.40606210577076,-1.05199162360801,7.62056647556314));
#12197=CARTESIAN_POINT('Ctrl Pts',(1.46198871831191,-1.20198407748167,7.61137922158509));
#12198=CARTESIAN_POINT('Ctrl Pts',(1.61904192398505,-1.54327609479098,7.59017688995366));
#12199=CARTESIAN_POINT('Ctrl Pts',(1.72871845227857,-1.72975677040328,7.57836374178375));
#12200=CARTESIAN_POINT('Ctrl Pts',(1.88766714357632,-1.94684663133831,7.56282226068313));
#12201=CARTESIAN_POINT('Ctrl Pts',(1.92019644161005,-1.98903888688763,7.55970599223822));
#12202=CARTESIAN_POINT('Ctrl Pts',(1.97518321488984,-2.05681665238036,7.55450543614644));
#12203=CARTESIAN_POINT('Ctrl Pts',(1.99702770382565,-2.08288794567341,7.55245559214156));
#12204=CARTESIAN_POINT('Ctrl Pts',(2.02724406608525,-2.11781289031882,7.5496340212833));
#12205=CARTESIAN_POINT('Ctrl Pts',(2.03526037977817,-2.12697297256629,7.54888675112303));
#12206=CARTESIAN_POINT('Ctrl Pts',(2.04874955188261,-2.1422117098308,7.54763100784953));
#12207=CARTESIAN_POINT('Ctrl Pts',(2.05419409770233,-2.14831544302794,7.54712461634422));
#12208=CARTESIAN_POINT('Ctrl Pts',(2.06455321605354,-2.15984015072397,7.54616183730286));
#12209=CARTESIAN_POINT('Ctrl Pts',(2.06946312898463,-2.1652652411245,7.54570581157442));
#12210=CARTESIAN_POINT('Ctrl Pts',(2.0811213403259,-2.17805885801383,7.54462382834226));
#12211=CARTESIAN_POINT('Ctrl Pts',(2.0878854704134,-2.18541276465219,7.54399669834043));
#12212=CARTESIAN_POINT('Ctrl Pts',(2.11162699873649,-2.21098466382968,7.54179812622171));
#12213=CARTESIAN_POINT('Ctrl Pts',(2.12878077822029,-2.22903670955622,7.54021421677398));
#12214=CARTESIAN_POINT('Ctrl Pts',(2.30180286110789,-2.406944018976,7.52429980588636));
#12215=CARTESIAN_POINT('Ctrl Pts',(2.47366310376377,-2.55037895359194,7.50902976931343));
#12216=CARTESIAN_POINT('Ctrl Pts',(2.78052681236518,-2.7565903635249,7.48408255841565));
#12217=CARTESIAN_POINT('Ctrl Pts',(2.9075419699288,-2.82991267755118,7.47430532702304));
#12218=CARTESIAN_POINT('Ctrl Pts',(3.11256812964798,-2.93031338644525,7.45949384584328));
#12219=CARTESIAN_POINT('Ctrl Pts',(3.18736650189891,-2.96347547386831,7.45427515007964));
#12220=CARTESIAN_POINT('Ctrl Pts',(3.28575893153008,-3.00268831142673,7.44764186331407));
#12221=CARTESIAN_POINT('Ctrl Pts',(3.30826649823546,-3.01136683758988,7.44613969303666));
#12222=CARTESIAN_POINT('Ctrl Pts',(3.3451039708181,-3.02509766077058,7.44370531847486));
#12223=CARTESIAN_POINT('Ctrl Pts',(3.35937558334564,-3.03030264760154,7.44276804795086));
#12224=CARTESIAN_POINT('Ctrl Pts',(3.38698557456558,-3.04015164001144,7.44096587847708));
#12225=CARTESIAN_POINT('Ctrl Pts',(3.40031869737615,-3.04480924569405,7.44010054506261));
#12226=CARTESIAN_POINT('Ctrl Pts',(3.43110378217191,-3.05533672780294,7.43811372720588));
#12227=CARTESIAN_POINT('Ctrl Pts',(3.44857639593675,-3.06114502668276,7.43699429423566));
#12228=CARTESIAN_POINT('Ctrl Pts',(3.50502868465343,-3.07937531491875,7.43340316061855));
#12229=CARTESIAN_POINT('Ctrl Pts',(3.54419635048831,-3.09120524265147,7.43095080365681));
#12230=CARTESIAN_POINT('Ctrl Pts',(3.81365964326605,-3.1670240162034,7.41432395756224));
#12231=CARTESIAN_POINT('Ctrl Pts',(4.05022885863677,-3.20596765644971,7.40101379923618));
#12232=CARTESIAN_POINT('Ctrl Pts',(4.42608717966414,-3.22553128210508,7.37995976634447));
#12233=CARTESIAN_POINT('Ctrl Pts',(4.56353067942897,-3.22389631315354,7.37226130702679));
#12234=CARTESIAN_POINT('Ctrl Pts',(4.74267964850517,-3.21029525195857,7.36178605549637));
#12235=CARTESIAN_POINT('Ctrl Pts',(4.7848505594209,-3.20625597353815,7.35928762822203));
#12236=CARTESIAN_POINT('Ctrl Pts',(4.8554629321712,-3.19808484234549,7.35503132067655));
#12237=CARTESIAN_POINT('Ctrl Pts',(4.88395173418012,-3.19440154096533,7.35329408067575));
#12238=CARTESIAN_POINT('Ctrl Pts',(4.92366873938594,-3.18872575756332,7.35083939479156));
#12239=CARTESIAN_POINT('Ctrl Pts',(4.93494229071351,-3.18705363255897,7.35013894072391));
#12240=CARTESIAN_POINT('Ctrl Pts',(4.95413933561673,-3.18410212180901,7.34893950892251));
#12241=CARTESIAN_POINT('Ctrl Pts',(4.96206748666253,-3.18285284858524,7.34844221269011));
#12242=CARTESIAN_POINT('Ctrl Pts',(4.97737460761431,-3.18038220360127,7.34747817740011));
#12243=CARTESIAN_POINT('Ctrl Pts',(4.98475408340319,-3.17916474605474,7.34701168332264));
#12244=CARTESIAN_POINT('Ctrl Pts',(5.00471091697265,-3.17580088756422,7.34574552855238));
#12245=CARTESIAN_POINT('Ctrl Pts',(5.01727971856154,-3.17360548979258,7.34494317402932));
#12246=CARTESIAN_POINT('Ctrl Pts',(5.06460240635232,-3.16504972200412,7.3419044803148));
#12247=CARTESIAN_POINT('Ctrl Pts',(5.09926256045062,-3.15819286776999,7.33964272835365));
#12248=CARTESIAN_POINT('Ctrl Pts',(5.46692456952255,-3.07915521389287,7.31531447524016));
#12249=CARTESIAN_POINT('Ctrl Pts',(5.78659909684695,-2.95516948877348,7.29149814442993));
#12250=CARTESIAN_POINT('Ctrl Pts',(6.13506398475503,-2.75179263825539,7.26516849734931));
#12251=CARTESIAN_POINT('Ctrl Pts',(6.18824889739357,-2.71863625382783,7.26112816460795));
#12252=CARTESIAN_POINT('Ctrl Pts',(6.27796414239646,-2.65900431523359,7.25427587552249));
#12253=CARTESIAN_POINT('Ctrl Pts',(6.31496621374648,-2.63327494698932,7.25143832987609));
#12254=CARTESIAN_POINT('Ctrl Pts',(6.36706105545717,-2.59540555160179,7.247424972149));
#12255=CARTESIAN_POINT('Ctrl Pts',(6.38260163068106,-2.58389339914262,7.24622531066522));
#12256=CARTESIAN_POINT('Ctrl Pts',(6.40938819663329,-2.56367447575151,7.24415296493719));
#12257=CARTESIAN_POINT('Ctrl Pts',(6.42068179091017,-2.55503196280005,7.24327780812886));
#12258=CARTESIAN_POINT('Ctrl Pts',(6.4437414798932,-2.53714209511834,7.24148775973954));
#12259=CARTESIAN_POINT('Ctrl Pts',(6.45550112494956,-2.5278869630461,7.24057320501637));
#12260=CARTESIAN_POINT('Ctrl Pts',(6.48523023529931,-2.5041522269333,7.23825653430463));
#12261=CARTESIAN_POINT('Ctrl Pts',(6.50310961532524,-2.48956075712994,7.23685892454179));
#12262=CARTESIAN_POINT('Ctrl Pts',(6.57128501873422,-2.43269153521718,7.23151096617996));
#12263=CARTESIAN_POINT('Ctrl Pts',(6.62044243041523,-2.38906985816482,7.22761537674616));
#12264=CARTESIAN_POINT('Ctrl Pts',(6.91125386096917,-2.11466117313467,7.20422891638768));
#12265=CARTESIAN_POINT('Ctrl Pts',(7.11709970765209,-1.84899042296554,7.1864273639643));
#12266=CARTESIAN_POINT('Ctrl Pts',(7.30102871677801,-1.51551481530063,7.16431105229617));
#12267=CARTESIAN_POINT('Ctrl Pts',(7.32271934705333,-1.47408061462171,7.16156234747799));
#12268=CARTESIAN_POINT('Ctrl Pts',(7.35723942624506,-1.40449457136165,7.15692081640959));
#12269=CARTESIAN_POINT('Ctrl Pts',(7.37057930062141,-1.3766027260209,7.1550537879378));
#12270=CARTESIAN_POINT('Ctrl Pts',(7.38842410289604,-1.33786960600319,7.15244619636444));
#12271=CARTESIAN_POINT('Ctrl Pts',(7.39327462216904,-1.32718820700389,7.15172556109115));
#12272=CARTESIAN_POINT('Ctrl Pts',(7.40137122225159,-1.30909683830656,7.15050201091301));
#12273=CARTESIAN_POINT('Ctrl Pts',(7.40464797542145,-1.3017005640678,7.15000094742551));
#12274=CARTESIAN_POINT('Ctrl Pts',(7.41086925895172,-1.28751391401718,7.14903812000192));
#12275=CARTESIAN_POINT('Ctrl Pts',(7.41381829595241,-1.2807256180091,7.14857665404869));
#12276=CARTESIAN_POINT('Ctrl Pts',(7.42082342557149,-1.26444752390577,7.14746837819304));
#12277=CARTESIAN_POINT('Ctrl Pts',(7.42485733866612,-1.25494835194159,7.1468202618492));
#12278=CARTESIAN_POINT('Ctrl Pts',(7.43925521269443,-1.22058600593344,7.14447123678265));
#12279=CARTESIAN_POINT('Ctrl Pts',(7.44935265233791,-1.1956132837017,7.1427555707597));
#12280=CARTESIAN_POINT('Ctrl Pts',(7.52007427991809,-1.01419490974086,7.13024559021496));
#12281=CARTESIAN_POINT('Ctrl Pts',(7.56870678481348,-0.853366255022636,
7.11892184163296));
#12282=CARTESIAN_POINT('Ctrl Pts',(7.63604262722976,-0.545924068564765,
7.09763134699031));
#12283=CARTESIAN_POINT('Ctrl Pts',(7.65763179825853,-0.400354411450338,
7.08769347469783));
#12284=CARTESIAN_POINT('Ctrl Pts',(7.67583711996911,-0.169912452741478,
7.07241736234439));
#12285=CARTESIAN_POINT('Ctrl Pts',(7.67917671221306,-0.0857802343074928,
7.06693207621422));
#12286=CARTESIAN_POINT('Ctrl Pts',(7.67921897253183,-0.00107186857600834,
7.06150815186532));
#12287=CARTESIAN_POINT('Ctrl Pts',(7.67921910621823,-0.000535933988464888,
7.06147383960103));
#12288=CARTESIAN_POINT('Ctrl Pts',(7.67921910621823,-4.71466720739905E-12,
7.06143953130409));
#12289=CARTESIAN_POINT('Origin',(4.45646910621825,-5.13094777615093E-16,
-2.31077344927308));
#12290=CARTESIAN_POINT('',(7.67921910621823,-9.10779638672584E-11,5.81337971654115));
#12291=CARTESIAN_POINT('',(7.67921910621823,3.83865910396161E-12,6.06327685380577));
#12292=CARTESIAN_POINT('',(7.67921910621823,-3.51191647465084E-13,-2.31077344927308));
#12293=CARTESIAN_POINT('',(7.6792176224508,0.00276905877516891,5.81322441567618));
#12294=CARTESIAN_POINT('Ctrl Pts',(7.67921910621823,-9.10779638672584E-11,
5.81337971654115));
#12295=CARTESIAN_POINT('Ctrl Pts',(7.67921910621826,0.000923861410410587,
5.81332772766874));
#12296=CARTESIAN_POINT('Ctrl Pts',(7.67921870895504,0.00184773084885948,
5.81327574292358));
#12297=CARTESIAN_POINT('Ctrl Pts',(7.67921791440811,0.00277160796994168,
5.81322376224255));
#12298=CARTESIAN_POINT('',(7.15082074185096,-1.76821571819255,4.67690209133339));
#12299=CARTESIAN_POINT('Ctrl Pts',(7.6792179166238,0.00276903041849574,
5.81322390726497));
#12300=CARTESIAN_POINT('Ctrl Pts',(7.67900856449745,0.246424467231695,5.79951496557771));
#12301=CARTESIAN_POINT('Ctrl Pts',(7.65116821843853,0.489250992218867,5.78622294437281));
#12302=CARTESIAN_POINT('Ctrl Pts',(7.58979339265802,0.754462998349227,5.77011732124514));
#12303=CARTESIAN_POINT('Ctrl Pts',(7.58297494971163,0.782238196207692,5.76840989669069));
#12304=CARTESIAN_POINT('Ctrl Pts',(7.57043845281463,0.830521272702615,5.76539972955178));
#12305=CARTESIAN_POINT('Ctrl Pts',(7.56488505924565,0.851070434140909,5.76410520256966));
#12306=CARTESIAN_POINT('Ctrl Pts',(7.5563959368466,0.881290709280791,5.76217956363626));
#12307=CARTESIAN_POINT('Ctrl Pts',(7.55361749252557,0.891005912594745,5.7615571591039));
#12308=CARTESIAN_POINT('Ctrl Pts',(7.54860210507242,0.908235958343354,5.76044709417541));
#12309=CARTESIAN_POINT('Ctrl Pts',(7.54638336986067,0.915755906412577,5.75996049006881));
#12310=CARTESIAN_POINT('Ctrl Pts',(7.54151146076358,0.932048944867181,5.75890151687508));
#12311=CARTESIAN_POINT('Ctrl Pts',(7.53884833932929,0.940818698452763,5.75832859813902));
#12312=CARTESIAN_POINT('Ctrl Pts',(7.53136695194085,0.965082421935289,5.75673559457842));
#12313=CARTESIAN_POINT('Ctrl Pts',(7.52646910105616,0.980551298451076,5.75571107863792));
#12314=CARTESIAN_POINT('Ctrl Pts',(7.49924541920163,1.06432809565836,5.75011639906219));
#12315=CARTESIAN_POINT('Ctrl Pts',(7.47475796773551,1.1319066359539,5.74543688440981));
#12316=CARTESIAN_POINT('Ctrl Pts',(7.4354466989433,1.23002261276611,5.73845045926817));
#12317=CARTESIAN_POINT('Ctrl Pts',(7.42236478590468,1.26123979768473,5.73619816128619));
#12318=CARTESIAN_POINT('Ctrl Pts',(7.34076793638534,1.44765996886942,5.72259124765988));
#12319=CARTESIAN_POINT('Ctrl Pts',(7.26057646519738,1.5974612293486,5.71101510603924));
#12320=CARTESIAN_POINT('Ctrl Pts',(7.10402919691497,1.84146781002633,5.69157265587832));
#12321=CARTESIAN_POINT('Ctrl Pts',(7.03347524038021,1.93897458849221,5.68361820729284));
#12322=CARTESIAN_POINT('Ctrl Pts',(6.91232519687503,2.08807317405674,5.67121251013103));
#12323=CARTESIAN_POINT('Ctrl Pts',(6.8651667275426,2.1423015200399,5.66664262983613));
#12324=CARTESIAN_POINT('Ctrl Pts',(6.80112192807073,2.21115646302847,5.66075875143344));
#12325=CARTESIAN_POINT('Ctrl Pts',(6.78584445918166,2.22724499405994,5.65937776061662));
#12326=CARTESIAN_POINT('Ctrl Pts',(6.76127645552357,2.2525879613569,5.6571920901708));
#12327=CARTESIAN_POINT('Ctrl Pts',(6.75209369110902,2.26194544903647,5.65638277993084));
#12328=CARTESIAN_POINT('Ctrl Pts',(6.73300848548805,2.28115785967703,5.65471625633208));
#12329=CARTESIAN_POINT('Ctrl Pts',(6.72309853924008,2.29100496490285,5.65385939928364));
#12330=CARTESIAN_POINT('Ctrl Pts',(6.700633240538,2.31303935285052,5.65193573423835));
#12331=CARTESIAN_POINT('Ctrl Pts',(6.68804197297036,2.32518951243891,5.65087056273352));
#12332=CARTESIAN_POINT('Ctrl Pts',(6.6555095972262,2.35607450474447,5.64815100026633));
#12333=CARTESIAN_POINT('Ctrl Pts',(6.63542748435271,2.37465926160609,5.64650303422928));
#12334=CARTESIAN_POINT('Ctrl Pts',(6.46129972570706,2.53173470703194,5.63246704371628));
#12335=CARTESIAN_POINT('Ctrl Pts',(6.29446373181011,2.65533758430647,5.6207355687472));
#12336=CARTESIAN_POINT('Ctrl Pts',(5.96619680930918,2.85267550021613,5.59928750437024));
#12337=CARTESIAN_POINT('Ctrl Pts',(5.80834629009445,2.93077714346589,5.58955710524609));
#12338=CARTESIAN_POINT('Ctrl Pts',(5.59995643053094,3.01345234605205,5.57655570021058));
#12339=CARTESIAN_POINT('Ctrl Pts',(5.55459130081789,3.03027811864658,5.57371544604752));
#12340=CARTESIAN_POINT('Ctrl Pts',(5.47890323341279,3.05642781959852,5.56893395573933));
#12341=CARTESIAN_POINT('Ctrl Pts',(5.4487896005746,3.06633697192618,5.56702055168781));
#12342=CARTESIAN_POINT('Ctrl Pts',(5.40722980152017,3.07933629201336,5.5643585313215));
#12343=CARTESIAN_POINT('Ctrl Pts',(5.39590438844032,3.08281028274428,5.56363094806922));
#12344=CARTESIAN_POINT('Ctrl Pts',(5.37679148198509,3.088557932028,5.56239903538514));
#12345=CARTESIAN_POINT('Ctrl Pts',(5.36901395099259,3.09086481087599,5.56189661674324));
#12346=CARTESIAN_POINT('Ctrl Pts',(5.35414715794404,3.09521341811359,5.56093395870326));
#12347=CARTESIAN_POINT('Ctrl Pts',(5.34705946440774,3.09726020856029,5.56047403457025));
#12348=CARTESIAN_POINT('Ctrl Pts',(5.32820147412363,3.10263595416122,5.5592478437888));
#12349=CARTESIAN_POINT('Ctrl Pts',(5.31641928224329,3.1059222251656,5.55847916943823));
#12350=CARTESIAN_POINT('Ctrl Pts',(5.27392728363824,3.11751371499186,5.55569845687809));
#12351=CARTESIAN_POINT('Ctrl Pts',(5.24311470579462,3.12543087565918,5.55366608487108));
#12352=CARTESIAN_POINT('Ctrl Pts',(4.87672696202815,3.21381168402107,5.52935134168323));
#12353=CARTESIAN_POINT('Ctrl Pts',(4.53043031056119,3.24033771928698,5.50520394945881));
#12354=CARTESIAN_POINT('Ctrl Pts',(4.12385546154255,3.20615574976477,5.47857501192268));
#12355=CARTESIAN_POINT('Ctrl Pts',(4.06139989117354,3.1990604380419,5.47452243970827));
#12356=CARTESIAN_POINT('Ctrl Pts',(3.95448316596778,3.18373480180905,5.46765165137932));
#12357=CARTESIAN_POINT('Ctrl Pts',(3.90991600046186,3.17638744600244,5.46480766217799));
#12358=CARTESIAN_POINT('Ctrl Pts',(3.84648795812378,3.16455608733335,5.46078690834855));
#12359=CARTESIAN_POINT('Ctrl Pts',(3.82749184868448,3.16083531153208,5.45958617378364));
#12360=CARTESIAN_POINT('Ctrl Pts',(3.79459690432893,3.15408387046255,5.45751257511264));
#12361=CARTESIAN_POINT('Ctrl Pts',(3.78068264301221,3.15113194582629,5.45663723011539));
#12362=CARTESIAN_POINT('Ctrl Pts',(3.75217596959817,3.14488672378497,5.45484733356307));
#12363=CARTESIAN_POINT('Ctrl Pts',(3.7375860145647,3.14158374711049,5.45393311518984));
#12364=CARTESIAN_POINT('Ctrl Pts',(3.7005740931552,3.13293338618671,5.45161837173749));
#12365=CARTESIAN_POINT('Ctrl Pts',(3.67818529136058,3.12744675716123,5.45022233764159));
#12366=CARTESIAN_POINT('Ctrl Pts',(3.59240842939892,3.10544798636379,5.44488795629383));
#12367=CARTESIAN_POINT('Ctrl Pts',(3.52946796365262,3.08724437142873,5.4410040027396));
#12368=CARTESIAN_POINT('Ctrl Pts',(3.14889632712346,2.96448573140725,5.41761261028515));
#12369=CARTESIAN_POINT('Ctrl Pts',(2.84863116048766,2.81295929817016,5.39979895291815));
#12370=CARTESIAN_POINT('Ctrl Pts',(2.53905500581176,2.5907197039378,5.37766819119971));
#12371=CARTESIAN_POINT('Ctrl Pts',(2.50165799437472,2.56261946095399,5.37491895093606));
#12372=CARTESIAN_POINT('Ctrl Pts',(2.44057681596239,2.51460772485839,5.37027659984267));
#12373=CARTESIAN_POINT('Ctrl Pts',(2.41654328533991,2.49515054074021,5.36840929845948));
#12374=CARTESIAN_POINT('Ctrl Pts',(2.38378329971818,2.46783888225906,5.3658013862751));
#12375=CARTESIAN_POINT('Ctrl Pts',(2.37481339281279,2.46027735879909,5.36508070971974));
#12376=CARTESIAN_POINT('Ctrl Pts',(2.35972841357764,2.44741935006658,5.36385710993688));
#12377=CARTESIAN_POINT('Ctrl Pts',(2.35359152472814,2.44214841538127,5.36335603847808));
#12378=CARTESIAN_POINT('Ctrl Pts',(2.34187828697669,2.4320111032381,5.36239321241617));
#12379=CARTESIAN_POINT('Ctrl Pts',(2.33629876087939,2.42714854164853,5.36193175590002));
#12380=CARTESIAN_POINT('Ctrl Pts',(2.32297961733642,2.41545992736965,5.36082352478989));
#12381=CARTESIAN_POINT('Ctrl Pts',(2.31525599725014,2.40861588367227,5.36017544398369));
#12382=CARTESIAN_POINT('Ctrl Pts',(2.28749405493776,2.38377644948445,5.35782671487045));
#12383=CARTESIAN_POINT('Ctrl Pts',(2.26764926382681,2.3655676954434,5.35611131412028));
#12384=CARTESIAN_POINT('Ctrl Pts',(2.12483700205699,2.23119353115142,5.34351300104494));
#12385=CARTESIAN_POINT('Ctrl Pts',(2.01096767671065,2.10576466517582,5.33209202841541));
#12386=CARTESIAN_POINT('Ctrl Pts',(1.81610134889612,1.85388136914968,5.31054840223347));
#12387=CARTESIAN_POINT('Ctrl Pts',(1.73303842616976,1.72955172535244,5.30045479072259));
#12388=CARTESIAN_POINT('Ctrl Pts',(1.59741556759932,1.49240283905983,5.2824223537282));
#12389=CARTESIAN_POINT('Ctrl Pts',(1.54217909739774,1.38143894524199,5.27442231367824));
#12390=CARTESIAN_POINT('Ctrl Pts',(1.48270287028835,1.24240901512131,5.2649249198695));
#12391=CARTESIAN_POINT('Ctrl Pts',(1.47226460153038,1.21712338533716,5.26321779805227));
#12392=CARTESIAN_POINT('Ctrl Pts',(1.45627085619532,1.17693701592555,5.26053575851637));
#12393=CARTESIAN_POINT('Ctrl Pts',(1.45050173426947,1.16212325170144,5.2595536892911));
#12394=CARTESIAN_POINT('Ctrl Pts',(1.43987185727296,1.13421935804556,5.25771597549725));
#12395=CARTESIAN_POINT('Ctrl Pts',(1.43498612362419,1.12113920193156,5.25685951191735));
#12396=CARTESIAN_POINT('Ctrl Pts',(1.42420018748514,1.09168027551467,5.25494155910723));
#12397=CARTESIAN_POINT('Ctrl Pts',(1.41834735073865,1.07528453761948,5.25388166449026));
#12398=CARTESIAN_POINT('Ctrl Pts',(1.4037341917408,1.03327624595637,5.2511848328358));
#12399=CARTESIAN_POINT('Ctrl Pts',(1.39516307214433,1.00759897354941,5.24955413619682));
#12400=CARTESIAN_POINT('Ctrl Pts',(1.3379427952436,0.828705336911774,5.23830944602236));
#12401=CARTESIAN_POINT('Ctrl Pts',(1.30049031183233,0.672135497194382,5.22907291227796));
#12402=CARTESIAN_POINT('Ctrl Pts',(1.24062592285557,0.301154980856729,5.20787029317528));
#12403=CARTESIAN_POINT('Ctrl Pts',(1.22770315884033,0.0860245480225275,
5.19609954522581));
#12404=CARTESIAN_POINT('Ctrl Pts',(1.23946508786304,-0.208099123167737,
5.17909551831905));
#12405=CARTESIAN_POINT('Ctrl Pts',(1.24556704783773,-0.287273149991707,
5.17442298293));
#12406=CARTESIAN_POINT('Ctrl Pts',(1.25641861233058,-0.382171381155469,
5.16862243665321));
#12407=CARTESIAN_POINT('Ctrl Pts',(1.25837291890157,-0.398194525142885,
5.16763613000343));
#12408=CARTESIAN_POINT('Ctrl Pts',(1.26161058041794,-0.423176630674345,
5.166086616547));
#12409=CARTESIAN_POINT('Ctrl Pts',(1.26281147575432,-0.43214626611738,5.16552790919859));
#12410=CARTESIAN_POINT('Ctrl Pts',(1.26512558519124,-0.448894009152649,
5.16448009107429));
#12411=CARTESIAN_POINT('Ctrl Pts',(1.26622947939416,-0.456673208434475,
5.16399150310423));
#12412=CARTESIAN_POINT('Ctrl Pts',(1.26881837561255,-0.474449716181971,
5.16287075105305));
#12413=CARTESIAN_POINT('Ctrl Pts',(1.27032196582853,-0.484444121464008,
5.16223756386857));
#12414=CARTESIAN_POINT('Ctrl Pts',(1.27445396453041,-0.511058038332236,
5.1605435694887));
#12415=CARTESIAN_POINT('Ctrl Pts',(1.27716552152691,-0.527664068159161,
5.1594783700627));
#12416=CARTESIAN_POINT('Ctrl Pts',(1.30224565933314,-0.674042475043102,
5.15002080423962));
#12417=CARTESIAN_POINT('Ctrl Pts',(1.3324166059841,-0.80233851284325,5.14126301938515));
#12418=CARTESIAN_POINT('Ctrl Pts',(1.42372747532276,-1.10586336698008,5.11992547912634));
#12419=CARTESIAN_POINT('Ctrl Pts',(1.49232008490354,-1.27839110651048,5.10729690797321));
#12420=CARTESIAN_POINT('Ctrl Pts',(1.61611270294635,-1.52537333360888,5.08897846802543));
#12421=CARTESIAN_POINT('Ctrl Pts',(1.66028908507281,-1.60491992273071,5.08303307195462));
#12422=CARTESIAN_POINT('Ctrl Pts',(1.72862508160112,-1.71656039342291,5.0746366721406));
#12423=CARTESIAN_POINT('Ctrl Pts',(1.75010755754954,-1.75023427033121,5.07209662052985));
#12424=CARTESIAN_POINT('Ctrl Pts',(1.78978051114918,-1.80994403080671,5.06757826239652));
#12425=CARTESIAN_POINT('Ctrl Pts',(1.80774006623573,-1.8361263699208,5.06559184665267));
#12426=CARTESIAN_POINT('Ctrl Pts',(1.83580985791605,-1.8757787758011,5.06257460105723));
#12427=CARTESIAN_POINT('Ctrl Pts',(1.84564324511415,-1.8894415184518,5.06153331771169));
#12428=CARTESIAN_POINT('Ctrl Pts',(1.86373091063091,-1.91416211148822,5.0596460231123));
#12429=CARTESIAN_POINT('Ctrl Pts',(1.87194996682861,-1.92524511879044,5.05879868121817));
#12430=CARTESIAN_POINT('Ctrl Pts',(1.89002946375878,-1.94930002937856,5.05695675340985));
#12431=CARTESIAN_POINT('Ctrl Pts',(1.89991765084662,-1.96225067567429,5.05596328139648));
#12432=CARTESIAN_POINT('Ctrl Pts',(1.92731267690875,-1.99757157418712,5.05324829395977));
#12433=CARTESIAN_POINT('Ctrl Pts',(1.94501797830594,-2.01978656003651,5.05153465353216));
#12434=CARTESIAN_POINT('Ctrl Pts',(2.04518419433832,-2.1421120176429,5.04205902452874));
#12435=CARTESIAN_POINT('Ctrl Pts',(2.13334101396892,-2.23741375370434,5.0345336028333));
#12436=CARTESIAN_POINT('Ctrl Pts',(2.38623112363911,-2.47968761399129,5.01460042258944));
#12437=CARTESIAN_POINT('Ctrl Pts',(2.56067592803624,-2.61547271564878,5.002542619857));
#12438=CARTESIAN_POINT('Ctrl Pts',(2.83684889586298,-2.78819416487964,4.98395315847202));
#12439=CARTESIAN_POINT('Ctrl Pts',(2.92876067783844,-2.83959479756779,4.97782989872249));
#12440=CARTESIAN_POINT('Ctrl Pts',(3.03849435149316,-2.89409122290364,4.97040074552768));
#12441=CARTESIAN_POINT('Ctrl Pts',(3.05403861451872,-2.90165557867087,4.9693456718687));
#12442=CARTESIAN_POINT('Ctrl Pts',(3.07803374309955,-2.9130945617444,4.96771171290074));
#12443=CARTESIAN_POINT('Ctrl Pts',(3.08644204644958,-2.91705842012141,4.96713815675236));
#12444=CARTESIAN_POINT('Ctrl Pts',(3.10196211357278,-2.92429301611773,4.96607745456314));
#12445=CARTESIAN_POINT('Ctrl Pts',(3.10906875151037,-2.92757427187282,4.96559096164928));
#12446=CARTESIAN_POINT('Ctrl Pts',(3.12521728770776,-2.93495907154992,4.96448370544755));
#12447=CARTESIAN_POINT('Ctrl Pts',(3.13426618886665,-2.93904671537241,4.96386200191928));
#12448=CARTESIAN_POINT('Ctrl Pts',(3.15782257184258,-2.94955699380067,4.96224060591144));
#12449=CARTESIAN_POINT('Ctrl Pts',(3.17235865360718,-2.9559143429365,4.96123718040098));
#12450=CARTESIAN_POINT('Ctrl Pts',(3.27188421095465,-2.99856914547841,4.9543501293015));
#12451=CARTESIAN_POINT('Ctrl Pts',(3.35834654757568,-3.03130035770005,4.94828474923369));
#12452=CARTESIAN_POINT('Ctrl Pts',(3.524419695971,-3.0861313056986,4.93662991481701));
#12453=CARTESIAN_POINT('Ctrl Pts',(3.60371473570473,-3.10897598635012,4.93106316396087));
#12454=CARTESIAN_POINT('Ctrl Pts',(3.81256386908113,-3.16055311967138,4.91651475170433));
#12455=CARTESIAN_POINT('Ctrl Pts',(3.94317824868259,-3.18437523488754,4.90753252958415));
#12456=CARTESIAN_POINT('Ctrl Pts',(4.17212957111309,-3.21167524374345,4.89219568324045));
#12457=CARTESIAN_POINT('Ctrl Pts',(4.26985011691826,-3.21883256511799,4.88577470503153));
#12458=CARTESIAN_POINT('Ctrl Pts',(4.40971127060308,-3.22268415016564,4.87678407014721));
#12459=CARTESIAN_POINT('Ctrl Pts',(4.4516899698963,-3.22301983372493,4.87411078362877));
#12460=CARTESIAN_POINT('Ctrl Pts',(4.52668170766121,-3.22215424995194,4.86937935350788));
#12461=CARTESIAN_POINT('Ctrl Pts',(4.55969168690786,-3.22126575262239,4.86731195122749));
#12462=CARTESIAN_POINT('Ctrl Pts',(4.60976263878109,-3.21914754007146,4.86419823131219));
#12463=CARTESIAN_POINT('Ctrl Pts',(4.6268363177046,-3.21828911428826,4.86314040189775));
#12464=CARTESIAN_POINT('Ctrl Pts',(4.65781965598681,-3.21648408354677,4.86122765054649));
#12465=CARTESIAN_POINT('Ctrl Pts',(4.67173144895827,-3.2155830011184,4.86037132715108));
#12466=CARTESIAN_POINT('Ctrl Pts',(4.70172346486876,-3.2134448722957,4.85853045769639));
#12467=CARTESIAN_POINT('Ctrl Pts',(4.71780118531136,-3.21217733117724,4.85754688970649));
#12468=CARTESIAN_POINT('Ctrl Pts',(4.76143809421167,-3.20840726999045,4.85488581599801));
#12469=CARTESIAN_POINT('Ctrl Pts',(4.78897604549433,-3.20567036692459,4.85321566820236));
#12470=CARTESIAN_POINT('Ctrl Pts',(4.93286645481124,-3.18949542228666,4.8445321855694));
#12471=CARTESIAN_POINT('Ctrl Pts',(5.04846445734408,-3.17007591575075,4.83770903264517));
#12472=CARTESIAN_POINT('Ctrl Pts',(5.38683259219747,-3.0940723463552,4.81788441951594));
#12473=CARTESIAN_POINT('Ctrl Pts',(5.60487242015871,-3.01993770381107,4.8053406301921));
#12474=CARTESIAN_POINT('Ctrl Pts',(5.91273802771762,-2.87705512169928,4.78600568126638));
#12475=CARTESIAN_POINT('Ctrl Pts',(6.00986424974131,-2.82579611135214,4.77963281334741));
#12476=CARTESIAN_POINT('Ctrl Pts',(6.11916369786089,-2.76077315318956,4.77192275847928));
#12477=CARTESIAN_POINT('Ctrl Pts',(6.13407875526853,-2.75173536933379,4.77085853245698));
#12478=CARTESIAN_POINT('Ctrl Pts',(6.15685771003802,-2.73767842783556,4.76921335427777));
#12479=CARTESIAN_POINT('Ctrl Pts',(6.16477465327649,-2.7327452737155,4.76863784638903));
#12480=CARTESIAN_POINT('Ctrl Pts',(6.17929353614584,-2.72361061537892,4.76757535314304));
#12481=CARTESIAN_POINT('Ctrl Pts',(6.18590169278284,-2.71941937279797,4.76708903763024));
#12482=CARTESIAN_POINT('Ctrl Pts',(6.20082610241681,-2.70987712340869,4.76598452049958));
#12483=CARTESIAN_POINT('Ctrl Pts',(6.20913297903031,-2.70451191474658,4.76536539879232));
#12484=CARTESIAN_POINT('Ctrl Pts',(6.23059018547676,-2.6905128571153,4.76375513378521));
#12485=CARTESIAN_POINT('Ctrl Pts',(6.24370205034098,-2.68182091470453,4.76276033895619));
#12486=CARTESIAN_POINT('Ctrl Pts',(6.33073835208014,-2.62320221766511,4.75608725411832));
#12487=CARTESIAN_POINT('Ctrl Pts',(6.40261971842986,-2.5703248582892,4.75023949808361));
#12488=CARTESIAN_POINT('Ctrl Pts',(6.53766763384786,-2.46206594209395,4.73871810019295));
#12489=CARTESIAN_POINT('Ctrl Pts',(6.60105071111069,-2.4070572959987,4.73305891556851));
#12490=CARTESIAN_POINT('Ctrl Pts',(6.80107096415059,-2.21928666995304,4.71450728585569));
#12491=CARTESIAN_POINT('Ctrl Pts',(6.92811460428226,-2.07686633212499,4.70161997360154));
#12492=CARTESIAN_POINT('Ctrl Pts',(7.07969194710109,-1.87318941970666,4.68503221910502));
#12493=CARTESIAN_POINT('Ctrl Pts',(7.11603373663308,-1.82122306534099,4.68093942591495));
#12494=CARTESIAN_POINT('Ctrl Pts',(7.15082074185096,-1.76821571819255,4.67690209133339));
#12495=CARTESIAN_POINT('',(7.49128385400174,-1.0844431793025,4.88098201673873));
#12496=CARTESIAN_POINT('Ctrl Pts',(7.15082074206232,-1.76821571787049,4.67690209167091));
#12497=CARTESIAN_POINT('Ctrl Pts',(7.25658458800507,-1.60705608760082,4.73783237965716));
#12498=CARTESIAN_POINT('Ctrl Pts',(7.34968713435654,-1.43333021245007,4.79384230980414));
#12499=CARTESIAN_POINT('Ctrl Pts',(7.4495156664105,-1.19638506817819,4.85508770712984));
#12500=CARTESIAN_POINT('Ctrl Pts',(7.47117036804548,-1.14073078200022,4.86847594001313));
#12501=CARTESIAN_POINT('Ctrl Pts',(7.49128387097725,-1.08444313179653,4.88098177561639));
#12502=CARTESIAN_POINT('Ctrl Pts',(7.49128385400174,-1.0844431793025,4.88098201673873));
#12503=CARTESIAN_POINT('Ctrl Pts',(7.48571404110737,-1.10003030330939,4.88193244700284));
#12504=CARTESIAN_POINT('Ctrl Pts',(7.48002363766192,-1.11557592977363,4.88288021106361));
#12505=CARTESIAN_POINT('Ctrl Pts',(7.43245320196961,-1.24249495035342,4.89061991409293));
#12506=CARTESIAN_POINT('Ctrl Pts',(7.3845538648513,-1.35151629996845,4.89727582348624));
#12507=CARTESIAN_POINT('Ctrl Pts',(7.28641881897214,-1.54502488880185,4.90940738558587));
#12508=CARTESIAN_POINT('Ctrl Pts',(7.23814284012053,-1.63033968458306,4.91487864608455));
#12509=CARTESIAN_POINT('Ctrl Pts',(7.12794689546593,-1.8058991226053,4.92664895678325));
#12510=CARTESIAN_POINT('Ctrl Pts',(7.06516983124947,-1.89545270042632,4.93296302842427));
#12511=CARTESIAN_POINT('Ctrl Pts',(6.98349610672583,-2.00020158726413,4.94095829133831));
#12512=CARTESIAN_POINT('Ctrl Pts',(6.96881702021602,-2.01860836630284,4.94238748798571));
#12513=CARTESIAN_POINT('Ctrl Pts',(6.94728574912995,-2.04500875282901,4.9444754461981));
#12514=CARTESIAN_POINT('Ctrl Pts',(6.94059360715719,-2.05313268065134,4.94512326244438));
#12515=CARTESIAN_POINT('Ctrl Pts',(6.92881731193899,-2.0672866567847,4.94626154400089));
#12516=CARTESIAN_POINT('Ctrl Pts',(6.92375064219131,-2.0733310378899,4.94675074869134));
#12517=CARTESIAN_POINT('Ctrl Pts',(6.91291530063083,-2.08616130198916,4.94779590577731));
#12518=CARTESIAN_POINT('Ctrl Pts',(6.90714077465332,-2.09294177008912,4.94835226674887));
#12519=CARTESIAN_POINT('Ctrl Pts',(6.89125110948031,-2.11144355019793,4.94988124319343));
#12520=CARTESIAN_POINT('Ctrl Pts',(6.88107964378012,-2.12311586774513,4.95085784337695));
#12521=CARTESIAN_POINT('Ctrl Pts',(6.83126891493184,-2.17945165927551,4.95562808268873));
#12522=CARTESIAN_POINT('Ctrl Pts',(6.79048006076839,-2.22307793353713,4.95949688204261));
#12523=CARTESIAN_POINT('Ctrl Pts',(6.70601718748927,-2.30852855333303,4.96739110501676));
#12524=CARTESIAN_POINT('Ctrl Pts',(6.66232923793585,-2.35030871913189,4.97141637915219));
#12525=CARTESIAN_POINT('Ctrl Pts',(6.47053728010992,-2.52366551895702,4.98875975978848));
#12526=CARTESIAN_POINT('Ctrl Pts',(6.31163388546885,-2.64267475497599,5.00229395102239));
#12527=CARTESIAN_POINT('Ctrl Pts',(6.06307733348232,-2.79529627511069,5.02165740077742));
#12528=CARTESIAN_POINT('Ctrl Pts',(5.98124771099469,-2.84076116939327,5.02778089059002));
#12529=CARTESIAN_POINT('Ctrl Pts',(5.86113495670316,-2.90080830275744,5.03640059343862));
#12530=CARTESIAN_POINT('Ctrl Pts',(5.82437775179795,-2.91832163024682,5.0389911961664));
#12531=CARTESIAN_POINT('Ctrl Pts',(5.75821164430768,-2.94832220318836,5.04357185156247));
#12532=CARTESIAN_POINT('Ctrl Pts',(5.72893086897331,-2.96107727516808,5.04557071651636));
#12533=CARTESIAN_POINT('Ctrl Pts',(5.68396957509363,-2.97987285142317,5.04859814551216));
#12534=CARTESIAN_POINT('Ctrl Pts',(5.66842405960474,-2.98622919746436,5.04963735402027));
#12535=CARTESIAN_POINT('Ctrl Pts',(5.65271848491895,-2.9925081454706,5.05067982369156));
#12536=CARTESIAN_POINT('Ctrl Pts',(5.65260763972783,-2.99255245324175,5.05068718075502));
#12537=CARTESIAN_POINT('Ctrl Pts',(5.65237822650347,-2.99264414102675,5.05070240669615));
#12538=CARTESIAN_POINT('Ctrl Pts',(5.65225965809875,-2.99269152015981,5.0507102755449));
#12539=CARTESIAN_POINT('Ctrl Pts',(5.65201423163662,-2.99278957400101,5.05072656250885));
#12540=CARTESIAN_POINT('Ctrl Pts',(5.65188737315497,-2.99284024769696,5.05073498059069));
#12541=CARTESIAN_POINT('Ctrl Pts',(5.65162475457962,-2.99294513148158,5.05075240644048));
#12542=CARTESIAN_POINT('Ctrl Pts',(5.65148899402042,-2.99299934039864,5.05076141416866));
#12543=CARTESIAN_POINT('Ctrl Pts',(5.65120791024285,-2.99311155440975,5.05078006295485));
#12544=CARTESIAN_POINT('Ctrl Pts',(5.65106258648902,-2.99316955815702,5.05078970396717));
#12545=CARTESIAN_POINT('Ctrl Pts',(5.65076166185503,-2.99328964220238,5.05080966647131));
#12546=CARTESIAN_POINT('Ctrl Pts',(5.65060606034434,-2.99335172095695,5.05081998791156));
#12547=CARTESIAN_POINT('Ctrl Pts',(5.65028380753271,-2.99348025776264,5.05084136223761));
#12548=CARTESIAN_POINT('Ctrl Pts',(5.65011715552066,-2.99354671403099,5.0508524150631));
#12549=CARTESIAN_POINT('Ctrl Pts',(5.64977196567573,-2.9936843328999,5.05087530727756));
#12550=CARTESIAN_POINT('Ctrl Pts',(5.64959342701954,-2.99375549344836,5.05088714659736));
#12551=CARTESIAN_POINT('Ctrl Pts',(5.6492235588312,-2.99390287429107,5.05091167143675));
#12552=CARTESIAN_POINT('Ctrl Pts',(5.64903222835298,-2.99397909221836,5.05092435687643));
#12553=CARTESIAN_POINT('Ctrl Pts',(5.64863579626798,-2.99413696987474,5.05095063850953));
#12554=CARTESIAN_POINT('Ctrl Pts',(5.64843069359028,-2.99421862686485,5.05096423460941));
#12555=CARTESIAN_POINT('Ctrl Pts',(5.64800565500928,-2.99438779576479,5.05099240746333));
#12556=CARTESIAN_POINT('Ctrl Pts',(5.64778571784138,-2.99447530452345,5.05100698411128));
#12557=CARTESIAN_POINT('Ctrl Pts',(5.64732985908287,-2.99465662376272,5.05103719377547));
#12558=CARTESIAN_POINT('Ctrl Pts',(5.64709393602716,-2.99475043060383,5.05105282666945));
#12559=CARTESIAN_POINT('Ctrl Pts',(5.64660485738868,-2.99494482929023,5.05108523085489));
#12560=CARTESIAN_POINT('Ctrl Pts',(5.64635170012362,-2.99504541692232,5.05110200200428));
#12561=CARTESIAN_POINT('Ctrl Pts',(5.64582679973206,-2.99525389989982,5.05113677157762));
#12562=CARTESIAN_POINT('Ctrl Pts',(5.64555505466544,-2.99536179036708,5.05115476983681));
#12563=CARTESIAN_POINT('Ctrl Pts',(5.64499151126087,-2.99558544424274,5.0511920899189));
#12564=CARTESIAN_POINT('Ctrl Pts',(5.64469971067464,-2.99570120200272,5.05121141155123));
#12565=CARTESIAN_POINT('Ctrl Pts',(5.64420359141788,-2.99589792941442,5.05124425783134));
#12566=CARTESIAN_POINT('Ctrl Pts',(5.64399928140574,-2.99597892079054,5.05125778321113));
#12567=CARTESIAN_POINT('Ctrl Pts',(5.63080417725614,-3.0012080847289,5.05213122177585));
#12568=CARTESIAN_POINT('Ctrl Pts',(5.61777988694038,-3.00627179529985,5.05298828167137));
#12569=CARTESIAN_POINT('Ctrl Pts',(5.588350868476,-3.01749370465314,5.05491364613198));
#12570=CARTESIAN_POINT('Ctrl Pts',(5.57192794068415,-3.0236031797876,5.05598030298161));
#12571=CARTESIAN_POINT('Ctrl Pts',(5.52966112792642,-3.03893556429234,5.05870606860748));
#12572=CARTESIAN_POINT('Ctrl Pts',(5.50374748444482,-3.04796301615364,5.06035870267325));
#12573=CARTESIAN_POINT('Ctrl Pts',(5.27865337527585,-3.12316860292018,5.07456242624772));
#12574=CARTESIAN_POINT('Ctrl Pts',(5.07355614975767,-3.17007704354512,5.08643785947386));
#12575=CARTESIAN_POINT('Ctrl Pts',(4.69325033171447,-3.21871839381532,5.10790194083449));
#12576=CARTESIAN_POINT('Ctrl Pts',(4.51968673807162,-3.22679539393264,5.11750902559948));
#12577=CARTESIAN_POINT('Ctrl Pts',(4.29830491589749,-3.21922519160031,5.13035859274909));
#12578=CARTESIAN_POINT('Ctrl Pts',(4.25032413907847,-3.21650906014664,5.13318031983141));
#12579=CARTESIAN_POINT('Ctrl Pts',(4.17097825415433,-3.210234818078,5.13793356555996));
#12580=CARTESIAN_POINT('Ctrl Pts',(4.13957151720611,-3.20728676023203,5.13983767126595));
#12581=CARTESIAN_POINT('Ctrl Pts',(4.0964594566348,-3.2026005726158,5.14248883434007));
#12582=CARTESIAN_POINT('Ctrl Pts',(4.08471177505838,-3.20125816705427,5.14321508312299));
#12583=CARTESIAN_POINT('Ctrl Pts',(4.06492087715667,-3.19888625896635,5.14444542706746));
#12584=CARTESIAN_POINT('Ctrl Pts',(4.05687353249974,-3.19789097515882,5.14494762314535));
#12585=CARTESIAN_POINT('Ctrl Pts',(4.04150640209735,-3.19593148003164,5.1459104150595));
#12586=CARTESIAN_POINT('Ctrl Pts',(4.03418604038425,-3.19497246945622,5.14637069905288));
#12587=CARTESIAN_POINT('Ctrl Pts',(4.01471992001893,-3.1923542241563,5.1475989322333));
#12588=CARTESIAN_POINT('Ctrl Pts',(4.00258036454496,-3.19065084815349,5.1483693030879));
#12589=CARTESIAN_POINT('Ctrl Pts',(3.95880582563907,-3.18425370047042,5.1511624375862));
#12590=CARTESIAN_POINT('Ctrl Pts',(3.92723255635927,-3.17915851512183,5.15320576550251));
#12591=CARTESIAN_POINT('Ctrl Pts',(3.55657512066857,-3.1136688143604,5.17749168822863));
#12592=CARTESIAN_POINT('Ctrl Pts',(3.22919235477271,-2.99976506171877,5.20158973399491));
#12593=CARTESIAN_POINT('Ctrl Pts',(2.87049842934907,-2.80620638166001,5.22819534149876));
#12594=CARTESIAN_POINT('Ctrl Pts',(2.81586992099581,-2.77462293108618,5.23226418374168));
#12595=CARTESIAN_POINT('Ctrl Pts',(2.7236692116218,-2.71764122591282,5.23915961113898));
#12596=CARTESIAN_POINT('Ctrl Pts',(2.68564255018691,-2.69301744349551,5.24201221334999));
#12597=CARTESIAN_POINT('Ctrl Pts',(2.63210419473049,-2.65672464268397,5.24604292947481));
#12598=CARTESIAN_POINT('Ctrl Pts',(2.61616051621262,-2.64570547816168,5.24724517412552));
#12599=CARTESIAN_POINT('Ctrl Pts',(2.58868504033778,-2.62634778873017,5.24932061074586));
#12600=CARTESIAN_POINT('Ctrl Pts',(2.57710741394206,-2.61807556500095,5.25019629483684));
#12601=CARTESIAN_POINT('Ctrl Pts',(2.55347595359909,-2.60095332947705,5.25198619935437));
#12602=CARTESIAN_POINT('Ctrl Pts',(2.54142815547933,-2.59209554798012,5.25290009121145));
#12603=CARTESIAN_POINT('Ctrl Pts',(2.51099163143338,-2.56938997346372,5.25521264031282));
#12604=CARTESIAN_POINT('Ctrl Pts',(2.4926886250003,-2.55542828197969,5.25660682491963));
#12605=CARTESIAN_POINT('Ctrl Pts',(2.42308022284281,-2.50114082246641,5.26192462495208));
#12606=CARTESIAN_POINT('Ctrl Pts',(2.37285240423198,-2.45945483241195,5.26579429457234));
#12607=CARTESIAN_POINT('Ctrl Pts',(2.07300568255103,-2.19481672237145,5.28919145986583));
#12608=CARTESIAN_POINT('Ctrl Pts',(1.85815003519757,-1.93566962973461,5.3070197553109));
#12609=CARTESIAN_POINT('Ctrl Pts',(1.66310396235734,-1.60792342042298,5.32916798777171));
#12610=CARTESIAN_POINT('Ctrl Pts',(1.64005659331291,-1.56720345762136,5.33191791364714));
#12611=CARTESIAN_POINT('Ctrl Pts',(1.60325995589937,-1.49875671423385,5.33656135345852));
#12612=CARTESIAN_POINT('Ctrl Pts',(1.58900851383478,-1.47130681190826,5.33842904403346));
#12613=CARTESIAN_POINT('Ctrl Pts',(1.5698987229574,-1.43316665633793,5.3410374603754));
#12614=CARTESIAN_POINT('Ctrl Pts',(1.56469993956813,-1.42264764410637,5.34175824323515));
#12615=CARTESIAN_POINT('Ctrl Pts',(1.55601370249326,-1.40482791621343,5.34298201053466));
#12616=CARTESIAN_POINT('Ctrl Pts',(1.55249602504105,-1.39754190105146,5.34348314256849));
#12617=CARTESIAN_POINT('Ctrl Pts',(1.54581278685394,-1.38356501145322,5.34444607686191));
#12618=CARTESIAN_POINT('Ctrl Pts',(1.54264278620235,-1.3768763650167,5.34490758091258));
#12619=CARTESIAN_POINT('Ctrl Pts',(1.53510797396376,-1.3608354838305,5.34601591825508));
#12620=CARTESIAN_POINT('Ctrl Pts',(1.53076502248097,-1.35147315426463,5.34666405795526));
#12621=CARTESIAN_POINT('Ctrl Pts',(1.5152506293183,-1.31760270414943,5.34901294258131));
#12622=CARTESIAN_POINT('Ctrl Pts',(1.50434191621799,-1.29297639532269,5.35072844129238));
#12623=CARTESIAN_POINT('Ctrl Pts',(1.42729501356592,-1.11298449445733,5.36330735817016));
#12624=CARTESIAN_POINT('Ctrl Pts',(1.37315556569585,-0.952783833335006,
5.37470692547687));
#12625=CARTESIAN_POINT('Ctrl Pts',(1.29538305061416,-0.644822100003465,
5.39619415002161));
#12626=CARTESIAN_POINT('Ctrl Pts',(1.26898159577177,-0.498186387000548,
5.40625281619682));
#12627=CARTESIAN_POINT('Ctrl Pts',(1.2392680533715,-0.22639783085076,5.42430436075756));
#12628=CARTESIAN_POINT('Ctrl Pts',(1.23291987206655,-0.101860118708508,
5.43235423357902));
#12629=CARTESIAN_POINT('Ctrl Pts',(1.23399276566092,0.0501447910228232,
5.44190168109828));
#12630=CARTESIAN_POINT('Ctrl Pts',(1.23453554598781,0.0775401410268698,
5.44361167635798));
#12631=CARTESIAN_POINT('Ctrl Pts',(1.23594557320512,0.120825494280249,5.4462972492166));
#12632=CARTESIAN_POINT('Ctrl Pts',(1.23658122801304,0.136721223832147,5.44728000905953));
#12633=CARTESIAN_POINT('Ctrl Pts',(1.23799577568304,0.166559142551229,5.44911844753835));
#12634=CARTESIAN_POINT('Ctrl Pts',(1.23874763001121,0.180502184459306,5.44997495004527));
#12635=CARTESIAN_POINT('Ctrl Pts',(1.24063971945123,0.211805519475726,5.4518922581791));
#12636=CARTESIAN_POINT('Ctrl Pts',(1.24182996340243,0.229162437617779,5.45295147514225));
#12637=CARTESIAN_POINT('Ctrl Pts',(1.24522806081473,0.273457489370556,5.45564518853079));
#12638=CARTESIAN_POINT('Ctrl Pts',(1.24763437132642,0.300379362240641,5.45727347066482));
#12639=CARTESIAN_POINT('Ctrl Pts',(1.26656614121557,0.485844734863518,5.46843517751405));
#12640=CARTESIAN_POINT('Ctrl Pts',(1.29449640024636,0.643011548987624,5.4775979383425));
#12641=CARTESIAN_POINT('Ctrl Pts',(1.38745149982558,1.00697475131792,5.49879981854309));
#12642=CARTESIAN_POINT('Ctrl Pts',(1.46189717919662,1.21053465676384,5.51063372901266));
#12643=CARTESIAN_POINT('Ctrl Pts',(1.59085055762625,1.47671291787271,5.52771749959235));
#12644=CARTESIAN_POINT('Ctrl Pts',(1.62818519816741,1.54701603770678,5.53240094293972));
#12645=CARTESIAN_POINT('Ctrl Pts',(1.67617882998829,1.62983572407868,5.53821380031675));
#12646=CARTESIAN_POINT('Ctrl Pts',(1.68438298130972,1.64375089317014,5.53920081332505));
#12647=CARTESIAN_POINT('Ctrl Pts',(1.69734751885659,1.66536710188411,5.54075123291304));
#12648=CARTESIAN_POINT('Ctrl Pts',(1.70203646386184,1.67311097417702,5.54131013210037));
#12649=CARTESIAN_POINT('Ctrl Pts',(1.71085621268371,1.68753937666373,5.54235817379593));
#12650=CARTESIAN_POINT('Ctrl Pts',(1.71497889110163,1.69422864589296,5.54284679222001));
#12651=CARTESIAN_POINT('Ctrl Pts',(1.72445914163435,1.70948566105769,5.54396744401497));
#12652=CARTESIAN_POINT('Ctrl Pts',(1.72983257044811,1.71804332520261,5.54460049917335));
#12653=CARTESIAN_POINT('Ctrl Pts',(1.74425576261011,1.74077544674501,5.54629378771886));
#12654=CARTESIAN_POINT('Ctrl Pts',(1.75337624469967,1.75490436527744,5.54735840716286));
#12655=CARTESIAN_POINT('Ctrl Pts',(1.83449568079927,1.87843711404869,5.55676966787602));
#12656=CARTESIAN_POINT('Ctrl Pts',(1.91298386988069,1.98341772779215,5.56547783271349));
#12657=CARTESIAN_POINT('Ctrl Pts',(2.11776787485982,2.22511409491698,5.58680076541084));
#12658=CARTESIAN_POINT('Ctrl Pts',(2.24995562244796,2.3562601943199,5.5994675741388));
#12659=CARTESIAN_POINT('Ctrl Pts',(2.46265403886111,2.53359648609577,5.61783067491177));
#12660=CARTESIAN_POINT('Ctrl Pts',(2.53503946247744,2.58892258944724,5.62378406187063));
#12661=CARTESIAN_POINT('Ctrl Pts',(2.64243608428466,2.66401945770731,5.63219056559815));
#12662=CARTESIAN_POINT('Ctrl Pts',(2.67562001170284,2.68631573072059,5.63473296499141));
#12663=CARTESIAN_POINT('Ctrl Pts',(2.73590734365723,2.7252145150741,5.63925512966341));
#12664=CARTESIAN_POINT('Ctrl Pts',(2.76285728065968,2.74204413392283,5.6412430231258));
#12665=CARTESIAN_POINT('Ctrl Pts',(2.80446553164012,2.76718002684345,5.64426210178119));
#12666=CARTESIAN_POINT('Ctrl Pts',(2.81894682166643,2.77577410755926,5.64530375881303));
#12667=CARTESIAN_POINT('Ctrl Pts',(2.84541686439616,2.7912038013422,5.64719153226137));
#12668=CARTESIAN_POINT('Ctrl Pts',(2.85738335612172,2.7980766179167,5.64803898153647));
#12669=CARTESIAN_POINT('Ctrl Pts',(2.88357315024145,2.81289553643384,5.64988091535598));
#12670=CARTESIAN_POINT('Ctrl Pts',(2.89781336100139,2.82081110149895,5.65087428748169));
#12671=CARTESIAN_POINT('Ctrl Pts',(2.93703400434898,2.84222460546706,5.65358843416815));
#12672=CARTESIAN_POINT('Ctrl Pts',(2.96213411581703,2.85550113835663,5.65530134306269));
#12673=CARTESIAN_POINT('Ctrl Pts',(3.10260011386277,2.92744022131947,5.66475983340365));
#12674=CARTESIAN_POINT('Ctrl Pts',(3.22124967784707,2.97944727213506,5.67226992560713));
#12675=CARTESIAN_POINT('Ctrl Pts',(3.54983521765312,3.10045943900629,5.69220181741328));
#12676=CARTESIAN_POINT('Ctrl Pts',(3.76422940900722,3.15525455092874,5.70427132166275));
#12677=CARTESIAN_POINT('Ctrl Pts',(4.086712805333,3.20320017475117,5.72287688337272));
#12678=CARTESIAN_POINT('Ctrl Pts',(4.19157952393162,3.21357120854047,5.72900402321083));
#12679=CARTESIAN_POINT('Ctrl Pts',(4.31402348958662,3.21964684228138,5.73643761746604));
#12680=CARTESIAN_POINT('Ctrl Pts',(4.33129946695436,3.22036474236261,5.73749291885307));
#12681=CARTESIAN_POINT('Ctrl Pts',(4.35787204032969,3.22125482087648,5.73912719501438));
#12682=CARTESIAN_POINT('Ctrl Pts',(4.36716530346022,3.22152585402803,5.73970083806339));
#12683=CARTESIAN_POINT('Ctrl Pts',(4.38428572892534,3.22195102548173,5.74076168005068));
#12684=CARTESIAN_POINT('Ctrl Pts',(4.39211239867391,3.22211686018867,5.74124822552181));
#12685=CARTESIAN_POINT('Ctrl Pts',(4.40986821501686,3.22242835871814,5.7423555789701));
#12686=CARTESIAN_POINT('Ctrl Pts',(4.41979742226745,3.22255664830897,5.7429773271956));
#12687=CARTESIAN_POINT('Ctrl Pts',(4.44559249720182,3.22277070176415,5.74459879993989));
#12688=CARTESIAN_POINT('Ctrl Pts',(4.46145847336754,3.22278518976129,5.74560225752012));
#12689=CARTESIAN_POINT('Ctrl Pts',(4.5697223890258,3.22208459893676,5.75248837229417));
#12690=CARTESIAN_POINT('Ctrl Pts',(4.66204432515844,3.2175131728796,5.75855272137907));
#12691=CARTESIAN_POINT('Ctrl Pts',(4.83618207946392,3.20136567169928,5.77020711636286));
#12692=CARTESIAN_POINT('Ctrl Pts',(4.9180061548293,3.19059662434563,5.77577450191839));
#12693=CARTESIAN_POINT('Ctrl Pts',(5.1300548718705,3.15436037967675,5.79032284188314));
#12694=CARTESIAN_POINT('Ctrl Pts',(5.25928824997423,3.12397051426465,5.7993043595104));
#12695=CARTESIAN_POINT('Ctrl Pts',(5.48005337302454,3.05744722787013,5.81464106667898));
#12696=CARTESIAN_POINT('Ctrl Pts',(5.57249081982316,3.02493086279902,5.82106256223416));
#12697=CARTESIAN_POINT('Ctrl Pts',(5.70223427046989,2.97253239714415,5.83005391239988));
#12698=CARTESIAN_POINT('Ctrl Pts',(5.74084812251682,2.95605319656,5.83272741093062));
#12699=CARTESIAN_POINT('Ctrl Pts',(5.80924295328493,2.92527108393362,5.83745922189585));
#12700=CARTESIAN_POINT('Ctrl Pts',(5.83914620930727,2.91125611287085,5.83952679422523));
#12701=CARTESIAN_POINT('Ctrl Pts',(5.88419686780973,2.88929113934443,5.84264078670076));
#12702=CARTESIAN_POINT('Ctrl Pts',(5.89950440546051,2.88167642046806,5.84369872032235));
#12703=CARTESIAN_POINT('Ctrl Pts',(5.92718401559389,2.8676313573661,5.84561166982905));
#12704=CARTESIAN_POINT('Ctrl Pts',(5.93957624948928,2.86124189080065,5.84646808737535));
#12705=CARTESIAN_POINT('Ctrl Pts',(5.96621428233791,2.84728769445016,5.84830917142137));
#12706=CARTESIAN_POINT('Ctrl Pts',(5.98044558904795,2.83969600597366,5.84929285953522));
#12707=CARTESIAN_POINT('Ctrl Pts',(6.01893970269511,2.81878859612649,5.85195429228117));
#12708=CARTESIAN_POINT('Ctrl Pts',(6.0430892866359,2.80526647395741,5.8536246767173));
#12709=CARTESIAN_POINT('Ctrl Pts',(6.16853935120409,2.73288469023007,5.86231035910533));
#12710=CARTESIAN_POINT('Ctrl Pts',(6.26675468142661,2.66884126879553,5.86913536228855));
#12711=CARTESIAN_POINT('Ctrl Pts',(6.54649661368538,2.46386495974867,5.88895982267156));
#12712=CARTESIAN_POINT('Ctrl Pts',(6.71667538330973,2.30874578757954,5.90150195518993));
#12713=CARTESIAN_POINT('Ctrl Pts',(6.94169305425103,2.05470799049169,5.92083457579292));
#12714=CARTESIAN_POINT('Ctrl Pts',(7.01021269064341,1.96889600901355,5.92720684464008));
#12715=CARTESIAN_POINT('Ctrl Pts',(7.08438773944989,1.86560054685676,5.93491630263972));
#12716=CARTESIAN_POINT('Ctrl Pts',(7.09444517964552,1.85135192449132,5.93598058869225));
#12717=CARTESIAN_POINT('Ctrl Pts',(7.10970393636753,1.82935768230533,5.93762587848579));
#12718=CARTESIAN_POINT('Ctrl Pts',(7.11498827056967,1.82166968503891,5.9382014374876));
#12719=CARTESIAN_POINT('Ctrl Pts',(7.12464422717785,1.80749006593233,5.93926403770364));
#12720=CARTESIAN_POINT('Ctrl Pts',(7.12902565175454,1.80100536410118,5.93975040903788));
#12721=CARTESIAN_POINT('Ctrl Pts',(7.13889064768162,1.78628946614509,5.94085507371115));
#12722=CARTESIAN_POINT('Ctrl Pts',(7.14435994029868,1.77804899846363,5.94147428751529));
#12723=CARTESIAN_POINT('Ctrl Pts',(7.15843168451342,1.75663409877361,5.94308483364394));
#12724=CARTESIAN_POINT('Ctrl Pts',(7.16697562524646,1.74342178451079,5.94407981901744));
#12725=CARTESIAN_POINT('Ctrl Pts',(7.22333561207384,1.65485121888495,5.9507558755446));
#12726=CARTESIAN_POINT('Ctrl Pts',(7.26809614297793,1.5776036327733,5.95660657303239));
#12727=CARTESIAN_POINT('Ctrl Pts',(7.3485491223689,1.42443330833082,5.96812352231471));
#12728=CARTESIAN_POINT('Ctrl Pts',(7.38460019395792,1.3487714698252,5.97377503997865));
#12729=CARTESIAN_POINT('Ctrl Pts',(7.49283878168835,1.09675323013322,5.99232203063751));
#12730=CARTESIAN_POINT('Ctrl Pts',(7.55235583180524,0.915373080372865,6.00521257966433));
#12731=CARTESIAN_POINT('Ctrl Pts',(7.61010129434065,0.666991465606748,6.02187337043636));
#12732=CARTESIAN_POINT('Ctrl Pts',(7.62281307446264,0.603771789738278,6.02603446623604));
#12733=CARTESIAN_POINT('Ctrl Pts',(7.64133921587721,0.49481344717113,6.03306899415619));
#12734=CARTESIAN_POINT('Ctrl Pts',(7.64808438469772,0.449255193559716,6.03596985672517));
#12735=CARTESIAN_POINT('Ctrl Pts',(7.65629381970488,0.384213302008736,6.04005588300774));
#12736=CARTESIAN_POINT('Ctrl Pts',(7.65856076712176,0.364838430654508,6.04126609215879));
#12737=CARTESIAN_POINT('Ctrl Pts',(7.66217922042267,0.331275274173806,6.04335084558643));
#12738=CARTESIAN_POINT('Ctrl Pts',(7.66361276032533,0.317096571861515,6.04422794399757));
#12739=CARTESIAN_POINT('Ctrl Pts',(7.6663538376426,0.288062404375125,6.0460168158811));
#12740=CARTESIAN_POINT('Ctrl Pts',(7.66765240828835,0.273206423953281,6.04692828761155));
#12741=CARTESIAN_POINT('Ctrl Pts',(7.67067776633357,0.235587281066092,6.04922693339431));
#12742=CARTESIAN_POINT('Ctrl Pts',(7.67226591368866,0.212813561422698,6.05060974414237));
#12743=CARTESIAN_POINT('Ctrl Pts',(7.67734907811268,0.126754805073478,6.05580405820949));
#12744=CARTESIAN_POINT('Ctrl Pts',(7.67921910621824,0.0633859825749122,
6.0595649876271));
#12745=CARTESIAN_POINT('Ctrl Pts',(7.67921910621823,3.83865910396161E-12,
6.06327685380577));
#12746=CARTESIAN_POINT('Origin',(6.37917532067789,0.,0.));
#12747=CARTESIAN_POINT('',(6.37917532067789,3.3456130901271,3.71576009063693));
#12748=CARTESIAN_POINT('',(6.37917546296132,2.5863715564937,3.37286375486987));
#12749=CARTESIAN_POINT('Ctrl Pts',(6.37917532067789,3.3456130901271,3.71576009063693));
#12750=CARTESIAN_POINT('Ctrl Pts',(6.37917532067789,3.24255076195948,3.66678682150482));
#12751=CARTESIAN_POINT('Ctrl Pts',(6.37917532320414,3.13881135649388,3.61831280819208));
#12752=CARTESIAN_POINT('Ctrl Pts',(6.37917532320414,2.89069148427495,3.50485012599878));
#12753=CARTESIAN_POINT('Ctrl Pts',(6.37917532067789,2.74467927191424,3.44009994888136));
#12754=CARTESIAN_POINT('Ctrl Pts',(6.37917532067789,2.59448758938272,3.3763047103935));
#12755=CARTESIAN_POINT('Ctrl Pts',(6.37917532067789,2.59043006761928,3.3745833507138));
#12756=CARTESIAN_POINT('Ctrl Pts',(6.37917532067789,2.5863715767527,3.3728637070571));
#12757=CARTESIAN_POINT('',(6.37917532067789,-3.03681439448832,3.9721226483366));
#12758=CARTESIAN_POINT('Origin',(6.37917532067789,0.,0.));
#12759=CARTESIAN_POINT('',(6.37917568135534,-2.58637139413976,3.74329856950612));
#12760=CARTESIAN_POINT('Ctrl Pts',(6.37917532067789,-2.58637143681758,3.74329848378769));
#12761=CARTESIAN_POINT('Ctrl Pts',(6.37917532067789,-2.7320504532865,3.8158297039793));
#12762=CARTESIAN_POINT('Ctrl Pts',(6.37917532045944,-2.87765867009868,3.88989647023702));
#12763=CARTESIAN_POINT('Ctrl Pts',(6.37917532045944,-3.02751940626012,3.96731715398979));
#12764=CARTESIAN_POINT('Ctrl Pts',(6.37917532067789,-3.03216640106086,3.96971905726743));
#12765=CARTESIAN_POINT('Ctrl Pts',(6.37917532067789,-3.03681439448831,3.9721226483366));
#12766=CARTESIAN_POINT('',(6.3791877629001,-2.58636241268454,3.49716578845862));
#12767=CARTESIAN_POINT('',(6.37917532067789,-2.58637166226708,-2.31077344927308));
#12768=CARTESIAN_POINT('',(6.37917532067789,-3.43098962587739,3.11492912548425));
#12769=CARTESIAN_POINT('Ctrl Pts',(6.37917532067789,-3.42636936949566,3.11682231207784));
#12770=CARTESIAN_POINT('Ctrl Pts',(6.37917532067789,-3.28944284185674,3.18199139775366));
#12771=CARTESIAN_POINT('Ctrl Pts',(6.37917532239532,-3.1510759240114,3.24655917840321));
#12772=CARTESIAN_POINT('Ctrl Pts',(6.37917532239532,-2.87198388415713,3.37336255932108));
#12773=CARTESIAN_POINT('Ctrl Pts',(6.37917532067789,-2.72904836859129,3.43653015731865));
#12774=CARTESIAN_POINT('Ctrl Pts',(6.37917532067789,-2.58636419175174,3.49716997456519));
#12775=CARTESIAN_POINT('',(6.37998521093114,-3.43053564256519,2.93155396442585));
#12776=CARTESIAN_POINT('',(6.37917532067789,-3.43098962587739,7.61832735979826E-16));
#12777=CARTESIAN_POINT('',(6.37918196868372,-2.58636672013265,2.49808050559515));
#12778=CARTESIAN_POINT('Ctrl Pts',(6.37917532067789,-2.58636751268136,2.49807891470192));
#12779=CARTESIAN_POINT('Ctrl Pts',(6.37917532067789,-2.72887860212156,2.56907486702406));
#12780=CARTESIAN_POINT('Ctrl Pts',(6.37917532053929,-2.87210044244327,2.64173957575438));
#12781=CARTESIAN_POINT('Ctrl Pts',(6.37917532053929,-3.15213081145752,2.78567562114608));
#12782=CARTESIAN_POINT('Ctrl Pts',(6.37917532067789,-3.29129959195667,2.85812191577848));
#12783=CARTESIAN_POINT('Ctrl Pts',(6.37917532067789,-3.42919155682922,2.9305834788995));
#12784=CARTESIAN_POINT('',(6.3791823737616,-2.58636641899648,2.24798337798073));
#12785=CARTESIAN_POINT('',(6.37917532067789,-2.58637166226708,-2.31077344927308));
#12786=CARTESIAN_POINT('',(6.37611478183885,-3.42549916664848,1.86508717508508));
#12787=CARTESIAN_POINT('Ctrl Pts',(6.37917532067789,-3.42379086727351,1.86491054275556));
#12788=CARTESIAN_POINT('Ctrl Pts',(6.37917532067789,-3.28673462067467,1.93071771383031));
#12789=CARTESIAN_POINT('Ctrl Pts',(6.37917532283357,-3.14809308263519,1.99603457995718));
#12790=CARTESIAN_POINT('Ctrl Pts',(6.37917532283357,-2.86996050619901,2.12368388664866));
#12791=CARTESIAN_POINT('Ctrl Pts',(6.37917532067789,-2.72795486563548,2.18712975387996));
#12792=CARTESIAN_POINT('Ctrl Pts',(6.37917532067789,-2.58636741807969,2.2479857024477));
#12793=CARTESIAN_POINT('',(6.37607929534711,-3.42544344211231,1.6817486560154));
#12794=CARTESIAN_POINT('',(6.37917532067789,-3.43098962587739,7.61832735979826E-16));
#12795=CARTESIAN_POINT('',(6.37917539807422,-2.58637160473072,1.24811343365893));
#12796=CARTESIAN_POINT('Ctrl Pts',(6.37917532067789,-2.58637161380091,1.24811341563195));
#12797=CARTESIAN_POINT('Ctrl Pts',(6.37917532067789,-2.72753521492361,1.31913928723047));
#12798=CARTESIAN_POINT('Ctrl Pts',(6.37917532051029,-2.86970473769156,1.39195767065841));
#12799=CARTESIAN_POINT('Ctrl Pts',(6.37917532051029,-3.1477213348857,1.53611018972745));
#12800=CARTESIAN_POINT('Ctrl Pts',(6.37917532067789,-3.2864602980215,1.60891634068854));
#12801=CARTESIAN_POINT('Ctrl Pts',(6.37917532067789,-3.42371299993736,1.68156992689594));
#12802=CARTESIAN_POINT('',(6.37917532113595,-2.58637166192656,1.00259120688551));
#12803=CARTESIAN_POINT('',(6.37917532067789,-2.58637166226708,-2.31077344927308));
#12804=CARTESIAN_POINT('',(6.3791753206778,-3.43420595741608,0.615284103491457));
#12805=CARTESIAN_POINT('Ctrl Pts',(6.37917532067789,-3.43420595741604,0.615284103491447));
#12806=CARTESIAN_POINT('Ctrl Pts',(6.37917532067789,-3.29741891646025,0.681127228409223));
#12807=CARTESIAN_POINT('Ctrl Pts',(6.37917532352613,-3.15892390364414,0.746478675402509));
#12808=CARTESIAN_POINT('Ctrl Pts',(6.37917532352613,-2.8774597106866,0.875641799826454));
#12809=CARTESIAN_POINT('Ctrl Pts',(6.37917532067789,-2.73164810422721,0.940615345270336));
#12810=CARTESIAN_POINT('Ctrl Pts',(6.37917532067789,-2.58637166199141,1.00259120703754));
#12811=CARTESIAN_POINT('',(6.38006015424921,-3.4304936204481,0.431770922268101));
#12812=CARTESIAN_POINT('',(6.37917532067789,-3.43098962587739,7.61832735979826E-16));
#12813=CARTESIAN_POINT('',(6.37917530233775,-2.60059989070202,1.86049092798513E-15));
#12814=CARTESIAN_POINT('Ctrl Pts',(6.37917532067789,-2.60059988642247,8.5336713043227E-9));
#12815=CARTESIAN_POINT('Ctrl Pts',(6.37917532067789,-2.74096448551843,0.0703914931049154));
#12816=CARTESIAN_POINT('Ctrl Pts',(6.37917532047357,-2.88242584110287,0.142797521996279));
#12817=CARTESIAN_POINT('Ctrl Pts',(6.37917532047357,-3.15734889890005,0.285445038517132));
#12818=CARTESIAN_POINT('Ctrl Pts',(6.37917532067789,-3.29408671125374,0.357340193452045));
#12819=CARTESIAN_POINT('Ctrl Pts',(6.37917532067789,-3.42919755846904,0.429047307451443));
#12820=CARTESIAN_POINT('',(6.37917532067381,3.40970963171873,-2.08166817117217E-15));
#12821=CARTESIAN_POINT('',(6.37917532067789,0.,0.));
#12822=CARTESIAN_POINT('',(6.37917532067789,3.43058507618661,0.00996756904321544));
#12823=CARTESIAN_POINT('Ctrl Pts',(6.37917532067789,3.43058507618662,0.00996756904321605));
#12824=CARTESIAN_POINT('Ctrl Pts',(6.37917532067789,3.42363017407561,0.0066432490635038));
#12825=CARTESIAN_POINT('Ctrl Pts',(6.37917532067789,3.41667162062538,0.00332067317801396));
#12826=CARTESIAN_POINT('Ctrl Pts',(6.37917532067789,3.40970963171769,2.18790263684099E-12));
#12827=CARTESIAN_POINT('',(6.37857781428809,3.43132439655042,0.193274600733303));
#12828=CARTESIAN_POINT('',(6.37917532067789,3.43098962587739,-7.61832735979826E-16));
#12829=CARTESIAN_POINT('',(6.38046276496377,2.58541407971855,0.629099045079643));
#12830=CARTESIAN_POINT('Ctrl Pts',(6.37917532067789,2.58599310446573,0.630264828345792));
#12831=CARTESIAN_POINT('Ctrl Pts',(6.37917532067789,2.72634555194803,0.560554151602523));
#12832=CARTESIAN_POINT('Ctrl Pts',(6.3791753205559,2.86720337116213,0.489210445502158));
#12833=CARTESIAN_POINT('Ctrl Pts',(6.3791753205559,3.14680320597834,0.345567079807686));
#12834=CARTESIAN_POINT('Ctrl Pts',(6.37917532067789,3.28758563896518,0.272204329161614));
#12835=CARTESIAN_POINT('Ctrl Pts',(6.37917532067789,3.42894278019802,0.19775621643526));
#12836=CARTESIAN_POINT('Ctrl Pts',(6.37917532067789,3.43079831146947,0.196778831244402));
#12837=CARTESIAN_POINT('Ctrl Pts',(6.37917532067789,3.43265378674765,0.195801337563912));
#12838=CARTESIAN_POINT('',(6.37917532099386,2.58637166203218,0.87851513268152));
#12839=CARTESIAN_POINT('',(6.37917532067789,2.58637166226708,-2.31077344927308));
#12840=CARTESIAN_POINT('',(6.37917532067788,3.4309896258774,1.26003777205275));
#12841=CARTESIAN_POINT('Ctrl Pts',(6.37917532067789,3.42328500954886,1.25880755392709));
#12842=CARTESIAN_POINT('Ctrl Pts',(6.37917532067789,3.29045367565351,1.19543400654417));
#12843=CARTESIAN_POINT('Ctrl Pts',(6.37917532244034,3.15626185421106,1.13259854029751));
#12844=CARTESIAN_POINT('Ctrl Pts',(6.37917532244034,2.87827578392745,1.00567409785647));
#12845=CARTESIAN_POINT('Ctrl Pts',(6.37917532067789,2.73212479642037,0.940755725708482));
#12846=CARTESIAN_POINT('Ctrl Pts',(6.37917532067789,2.58637166207725,0.878515132575993));
#12847=CARTESIAN_POINT('',(6.37730370004177,3.42771650614571,1.44343144191856));
#12848=CARTESIAN_POINT('',(6.37917532067789,3.43098962587739,-7.61832735979826E-16));
#12849=CARTESIAN_POINT('',(6.37917532696298,2.58637165759475,1.87594439571473));
#12850=CARTESIAN_POINT('Ctrl Pts',(6.37917532067789,2.58637165834049,1.87594439720601));
#12851=CARTESIAN_POINT('Ctrl Pts',(6.37917532067789,2.72296207022395,1.80763974829727));
#12852=CARTESIAN_POINT('Ctrl Pts',(6.37917532052268,2.86026107377465,1.73779740731373));
#12853=CARTESIAN_POINT('Ctrl Pts',(6.37917532052268,3.13594275047174,1.59584166551277));
#12854=CARTESIAN_POINT('Ctrl Pts',(6.37917532067789,3.27670524567701,1.52244549425824));
#12855=CARTESIAN_POINT('Ctrl Pts',(6.37917532067789,3.41959079935358,1.44725503297199));
#12856=CARTESIAN_POINT('Ctrl Pts',(6.37917532067789,3.42311930708574,1.44539779726455));
#12857=CARTESIAN_POINT('Ctrl Pts',(6.37917532067789,3.42664762619326,1.44354022985285));
#12858=CARTESIAN_POINT('',(6.37918119522423,2.5863672951246,2.12518466390817));
#12859=CARTESIAN_POINT('',(6.37917532067789,2.58637166226708,-2.31077344927308));
#12860=CARTESIAN_POINT('',(6.37707234371275,3.42716806216857,2.50981808392763));
#12861=CARTESIAN_POINT('Ctrl Pts',(6.37917532067789,3.42600824378348,2.50993925709623));
#12862=CARTESIAN_POINT('Ctrl Pts',(6.37917532067789,3.29337096368447,2.44609345245295));
#12863=CARTESIAN_POINT('Ctrl Pts',(6.37917532292,3.15924007754082,2.38271294856361));
#12864=CARTESIAN_POINT('Ctrl Pts',(6.37917532292,2.88260140945533,2.25527329380387));
#12865=CARTESIAN_POINT('Ctrl Pts',(6.37917532067789,2.73745665096598,2.19022396547602));
#12866=CARTESIAN_POINT('Ctrl Pts',(6.37917532067789,2.59068646954243,2.12704004536091));
#12867=CARTESIAN_POINT('Ctrl Pts',(6.37917532067789,2.58852740148246,2.12611114721521));
#12868=CARTESIAN_POINT('Ctrl Pts',(6.37917532067789,2.58636812502947,2.12518273374011));
#12869=CARTESIAN_POINT('',(6.37692902980926,3.42691262734832,2.69315322924028));
#12870=CARTESIAN_POINT('',(6.37917532067789,3.43098962587739,-7.61832735979826E-16));
#12871=CARTESIAN_POINT('',(6.37918160141763,2.58636699315934,3.1286030352177));
#12872=CARTESIAN_POINT('Ctrl Pts',(6.37917532067789,2.58636772558512,3.12860448938999));
#12873=CARTESIAN_POINT('Ctrl Pts',(6.37917532067789,2.72377271853466,3.05939745007247));
#12874=CARTESIAN_POINT('Ctrl Pts',(6.37917532049074,2.86217419915329,2.98842182782831));
#12875=CARTESIAN_POINT('Ctrl Pts',(6.37917532049074,3.13736378955755,2.84554807880643));
#12876=CARTESIAN_POINT('Ctrl Pts',(6.37917532067789,3.27707963871674,2.77209788112412));
#12877=CARTESIAN_POINT('Ctrl Pts',(6.37917532067789,3.41866961320406,2.69699822902537));
#12878=CARTESIAN_POINT('Ctrl Pts',(6.37917532067789,3.42217110366622,2.69514060888361));
#12879=CARTESIAN_POINT('Ctrl Pts',(6.37917532067789,3.42567240795605,2.69328266938512));
#12880=CARTESIAN_POINT('',(6.37917532067789,2.58637166226708,-2.31077344927308));
#12881=CARTESIAN_POINT('Origin',(206.833344075386,0.,0.));
#12882=CARTESIAN_POINT('',(6.62837333988161,3.27892070654281,3.77474224288293));
#12883=CARTESIAN_POINT('Ctrl Pts',(6.62603580309594,3.28236130364179,3.77175082320597));
#12884=CARTESIAN_POINT('Ctrl Pts',(6.54400502547545,3.30474507000467,3.75227137931291));
#12885=CARTESIAN_POINT('Ctrl Pts',(6.46198795242467,3.32574102461171,3.73365259200797));
#12886=CARTESIAN_POINT('Ctrl Pts',(6.37917532067789,3.3456130901271,3.71576009063693));
#12887=CARTESIAN_POINT('',(6.97215211287823,3.02321484681493,3.97983001953316));
#12888=CARTESIAN_POINT('Ctrl Pts',(6.96745972433549,3.02711333050602,3.97952068524248));
#12889=CARTESIAN_POINT('Ctrl Pts',(6.86017306897531,3.11610761504228,3.91182514943145));
#12890=CARTESIAN_POINT('Ctrl Pts',(6.74689823309609,3.20041018982336,3.84293949843672));
#12891=CARTESIAN_POINT('Ctrl Pts',(6.6284029078717,3.27890112099087,3.77475925573603));
#12892=CARTESIAN_POINT('',(6.63714354025222,2.37292574162162,4.40103865535663));
#12893=CARTESIAN_POINT('Ctrl Pts',(6.63711855526384,2.3729338705341,4.40104360874464));
#12894=CARTESIAN_POINT('Ctrl Pts',(6.66436682263207,2.49766393078106,4.33379224498954));
#12895=CARTESIAN_POINT('Ctrl Pts',(6.70730912100586,2.61378897659334,4.26444374464064));
#12896=CARTESIAN_POINT('Ctrl Pts',(6.82251116401291,2.83139221157415,4.123048075617));
#12897=CARTESIAN_POINT('Ctrl Pts',(6.8922421142993,2.93018531660515,4.05305893528313));
#12898=CARTESIAN_POINT('Ctrl Pts',(6.97154264924743,3.02268510374038,3.98288533237325));
#12899=CARTESIAN_POINT('Ctrl Pts',(6.97215682679145,3.02340044689291,3.98234234385051));
#12900=CARTESIAN_POINT('Ctrl Pts',(6.97277153762443,3.02411535324729,3.98179938347652));
#12901=CARTESIAN_POINT('',(7.19099309084831,1.70543136478218,4.70016067061871));
#12902=CARTESIAN_POINT('Ctrl Pts',(7.19099319326954,1.70543120055785,4.70016004197344));
#12903=CARTESIAN_POINT('Ctrl Pts',(7.05768222863756,1.91918479186951,4.6226005459991));
#12904=CARTESIAN_POINT('Ctrl Pts',(6.90177096221566,2.11235490214046,4.53573987292431));
#12905=CARTESIAN_POINT('Ctrl Pts',(6.70347989827123,2.31064596608489,4.43420714472505));
#12906=CARTESIAN_POINT('Ctrl Pts',(6.67075041713426,2.3420417073132,4.41769984393852));
#12907=CARTESIAN_POINT('Ctrl Pts',(6.63714132687621,2.37292777567092,4.40104689493868));
#12908=CARTESIAN_POINT('Ctrl Pts',(7.49128360962441,-1.08444291718913,4.88098182329727));
#12909=CARTESIAN_POINT('Ctrl Pts',(7.57445070748278,-0.991695767530693,
4.90158812612276));
#12910=CARTESIAN_POINT('Ctrl Pts',(7.65099179058753,-0.8924678343991,4.92086171312852));
#12911=CARTESIAN_POINT('Ctrl Pts',(7.8082523458007,-0.646879580013778,4.9600116730167));
#12912=CARTESIAN_POINT('Ctrl Pts',(7.88168782814486,-0.496205002355483,
4.97788797884683));
#12913=CARTESIAN_POINT('Ctrl Pts',(7.96978192849634,-0.221548058095216,
4.99642020088847));
#12914=CARTESIAN_POINT('Ctrl Pts',(7.99463425444134,-0.103359142162303,
5.00038423568684));
#12915=CARTESIAN_POINT('Ctrl Pts',(8.01211326010161,0.0803660628211763,
4.99975359834527));
#12916=CARTESIAN_POINT('Ctrl Pts',(8.01439868802338,0.143739735844232,4.99833648163297));
#12917=CARTESIAN_POINT('Ctrl Pts',(8.01259138727451,0.221360495872097,4.99511777741445));
#12918=CARTESIAN_POINT('Ctrl Pts',(8.01207221978763,0.235554826120059,4.99446850150878));
#12919=CARTESIAN_POINT('Ctrl Pts',(8.01099445753803,0.257172126518868,4.99338741634105));
#12920=CARTESIAN_POINT('Ctrl Pts',(8.01057226899669,0.264601754000765,4.99299922061733));
#12921=CARTESIAN_POINT('Ctrl Pts',(8.01000948285326,0.27342443630196,4.99251850621268));
#12922=CARTESIAN_POINT('Ctrl Pts',(8.00991855247719,0.274821229604134,4.9924418122137));
#12923=CARTESIAN_POINT('Ctrl Pts',(8.00977582860952,0.27697036175503,4.99232290488944));
#12924=CARTESIAN_POINT('Ctrl Pts',(8.00972532729969,0.277722806958215,4.99228110289905));
#12925=CARTESIAN_POINT('Ctrl Pts',(8.00963608199596,0.279038673397197,4.99220770173184));
#12926=CARTESIAN_POINT('Ctrl Pts',(8.00959757004527,0.279602114059626,4.99217617640346));
#12927=CARTESIAN_POINT('Ctrl Pts',(8.00951618108859,0.280783714389569,4.99210986348361));
#12928=CARTESIAN_POINT('Ctrl Pts',(8.00947324372347,0.281401868345432,4.99207505670626));
#12929=CARTESIAN_POINT('Ctrl Pts',(8.00936645504332,0.2829265290089,4.99198892262566));
#12930=CARTESIAN_POINT('Ctrl Pts',(8.00930219348069,0.283832998435099,4.99193746487618));
#12931=CARTESIAN_POINT('Ctrl Pts',(8.00904765528153,0.287380903063516,4.99173509080762));
#12932=CARTESIAN_POINT('Ctrl Pts',(8.00885163576263,0.290021809101788,4.99158234885387));
#12933=CARTESIAN_POINT('Ctrl Pts',(8.00857581971104,0.293617630215502,4.99137151526392));
#12934=CARTESIAN_POINT('Ctrl Pts',(8.00850167515199,0.294573070581933,4.99131521965872));
#12935=CARTESIAN_POINT('Ctrl Pts',(7.99573391015604,0.457219192837101,4.98168507297965));
#12936=CARTESIAN_POINT('Ctrl Pts',(7.9588726805899,0.614067202363164,4.96447590138363));
#12937=CARTESIAN_POINT('Ctrl Pts',(7.89447382037831,0.782155205343506,4.93847758919872));
#12938=CARTESIAN_POINT('Ctrl Pts',(7.88733759678773,0.799921002710326,4.93563026557539));
#12939=CARTESIAN_POINT('Ctrl Pts',(7.87214710745916,0.836083527033064,4.9296365821974));
#12940=CARTESIAN_POINT('Ctrl Pts',(7.86406639597203,0.854463551329238,4.92648302627241));
#12941=CARTESIAN_POINT('Ctrl Pts',(7.84683912384043,0.891993396233924,4.91983046092911));
#12942=CARTESIAN_POINT('Ctrl Pts',(7.83765954684862,0.911122334981121,4.91632265681671));
#12943=CARTESIAN_POINT('Ctrl Pts',(7.81806182513801,0.950278649661944,4.90890955196389));
#12944=CARTESIAN_POINT('Ctrl Pts',(7.80760352455399,0.970280169205902,4.90499384152793));
#12945=CARTESIAN_POINT('Ctrl Pts',(7.78524190471491,1.01131140639185,4.89670483459671));
#12946=CARTESIAN_POINT('Ctrl Pts',(7.77329998295004,1.03229105411954,4.8923232138641));
#12947=CARTESIAN_POINT('Ctrl Pts',(7.74771939462743,1.07542623486743,4.88303000318918));
#12948=CARTESIAN_POINT('Ctrl Pts',(7.73403417106869,1.09752525896396,4.87810821733423));
#12949=CARTESIAN_POINT('Ctrl Pts',(7.7047137303281,1.14299094381945,4.86766474399873));
#12950=CARTESIAN_POINT('Ctrl Pts',(7.68900907462563,1.16631315349381,4.86212652513195));
#12951=CARTESIAN_POINT('Ctrl Pts',(7.65532437253361,1.21435424181897,4.85036168180865));
#12952=CARTESIAN_POINT('Ctrl Pts',(7.63726195561945,1.23901925752238,4.84411614483842));
#12953=CARTESIAN_POINT('Ctrl Pts',(7.5984706626884,1.28988258743456,4.83083404018334));
#12954=CARTESIAN_POINT('Ctrl Pts',(7.57764365710047,1.31601533654054,4.82377594525967));
#12955=CARTESIAN_POINT('Ctrl Pts',(7.53284793993454,1.36996136284253,4.80874897585579));
#12956=CARTESIAN_POINT('Ctrl Pts',(7.50876158839627,1.39769425420913,4.80075575890809));
#12957=CARTESIAN_POINT('Ctrl Pts',(7.45686085092974,1.45500289392553,4.78371753530002));
#12958=CARTESIAN_POINT('Ctrl Pts',(7.4289043609337,1.48447885289504,4.77464531538174));
#12959=CARTESIAN_POINT('Ctrl Pts',(7.36852762470939,1.54545586007504,4.75528163768685));
#12960=CARTESIAN_POINT('Ctrl Pts',(7.335933276171,1.5768317599979,4.74496009493226));
#12961=CARTESIAN_POINT('Ctrl Pts',(7.26623678847155,1.64098942714486,4.7231778702185));
#12962=CARTESIAN_POINT('Ctrl Pts',(7.22896040182095,1.67365483176265,4.7116899453092));
#12963=CARTESIAN_POINT('Ctrl Pts',(7.19099262183641,1.70543064890463,4.70016024213821));
#12964=CARTESIAN_POINT('',(7.44179868886595,-2.56052656361313,4.29510059109848));
#12965=CARTESIAN_POINT('Ctrl Pts',(7.43760018588873,-2.55681065102966,4.29682665402984));
#12966=CARTESIAN_POINT('Ctrl Pts',(7.37455140393809,-2.44222979000476,4.36500756740177));
#12967=CARTESIAN_POINT('Ctrl Pts',(7.32043150814391,-2.32265920674659,4.42999823940972));
#12968=CARTESIAN_POINT('Ctrl Pts',(7.22351087100368,-2.05881741292851,4.55904201498614));
#12969=CARTESIAN_POINT('Ctrl Pts',(7.18339207724428,-1.91623224743013,4.62094087013212));
#12970=CARTESIAN_POINT('Ctrl Pts',(7.15082074146671,-1.76821571833791,4.67690209149419));
#12971=CARTESIAN_POINT('',(7.19731080507723,-2.82068711164422,4.12982512801404));
#12972=CARTESIAN_POINT('Ctrl Pts',(7.19924459195077,-2.81880677501399,4.1296886523242));
#12973=CARTESIAN_POINT('Ctrl Pts',(7.21211560828053,-2.8062829268458,4.13823707111259));
#12974=CARTESIAN_POINT('Ctrl Pts',(7.22487457054161,-2.79369647649002,4.14674469164499));
#12975=CARTESIAN_POINT('Ctrl Pts',(7.30716927425948,-2.71140177277215,4.2018239446048));
#12976=CARTESIAN_POINT('Ctrl Pts',(7.37554087547359,-2.63778413144905,4.24855436104107));
#12977=CARTESIAN_POINT('Ctrl Pts',(7.44191783873706,-2.56038763969479,4.29469616323415));
#12978=CARTESIAN_POINT('Ctrl Pts',(6.37917532067789,-3.03681439448832,3.9721226483366));
#12979=CARTESIAN_POINT('Ctrl Pts',(6.6575480987566,-2.98017745787073,4.01542339194582));
#12980=CARTESIAN_POINT('Ctrl Pts',(6.93157288344106,-2.90736320883569,4.06919443434768));
#12981=CARTESIAN_POINT('Ctrl Pts',(7.19690031496509,-2.8203511405513,4.12863408938004));
#12982=CARTESIAN_POINT('Origin',(4.45646910621825,0.,0.));
#12983=CARTESIAN_POINT('',(6.32992046864336,-2.62554739444332,-0.00153646747546771));
#12984=CARTESIAN_POINT('Ctrl Pts',(6.33207202947621,-2.6273817546684,8.65193333643433E-16));
#12985=CARTESIAN_POINT('Ctrl Pts',(6.34786150147485,-2.61859153627079,1.51541797368282E-15));
#12986=CARTESIAN_POINT('Ctrl Pts',(6.3635632560086,-2.6096640634631,1.86847043519414E-15));
#12987=CARTESIAN_POINT('Ctrl Pts',(6.37917529771412,-2.60059988273836,2.16580225975704E-15));
#12988=CARTESIAN_POINT('',(6.28979540306975,-2.65047774028998,5.88524282705277E-16));
#12989=CARTESIAN_POINT('Ctrl Pts',(6.28979540306975,-2.65047774028998,5.55111512312578E-16));
#12990=CARTESIAN_POINT('Ctrl Pts',(6.30271977741102,-2.64153799520552,-0.000512155825155562));
#12991=CARTESIAN_POINT('Ctrl Pts',(6.31557876201817,-2.63250371485126,-0.0010243116503117));
#12992=CARTESIAN_POINT('Ctrl Pts',(6.32837098102566,-2.62337586586299,-0.00153646747546782));
#12993=CARTESIAN_POINT('',(2.58488257447922,-2.62360084935056,5.82556414075021E-16));
#12994=CARTESIAN_POINT('Origin',(4.45646910621825,0.,0.));
#12995=CARTESIAN_POINT('',(2.70777160956256,3.52286049471024,6.63097267454378E-5));
#12996=CARTESIAN_POINT('Ctrl Pts',(2.70366602788722,3.52819471846405,1.72691722033491E-15));
#12997=CARTESIAN_POINT('Ctrl Pts',(2.6303277955966,3.48382721479545,-2.31975679365046E-15));
#12998=CARTESIAN_POINT('Ctrl Pts',(2.55868989239216,3.4369761734182,-1.18643451332771E-15));
#12999=CARTESIAN_POINT('Ctrl Pts',(2.48889033901316,3.38764193337989,-1.40339129206524E-15));
#13000=CARTESIAN_POINT('Ctrl Pts',(2.3907080577368,3.31824681553872,-1.82822104457045E-15));
#13001=CARTESIAN_POINT('Ctrl Pts',(2.29616136391543,3.24393985163692,-1.17259527911366E-15));
#13002=CARTESIAN_POINT('Ctrl Pts',(2.20540600264083,3.16513659897062,-2.1163626406917E-15));
#13003=CARTESIAN_POINT('Ctrl Pts',(2.11354814395808,3.08537604328003,-3.07159490148268E-15));
#13004=CARTESIAN_POINT('Ctrl Pts',(2.02557385752853,3.00100846009477,-3.8205868856292E-15));
#13005=CARTESIAN_POINT('Ctrl Pts',(1.9416867490807,2.91243153502283,-1.7277845820729E-15));
#13006=CARTESIAN_POINT('Ctrl Pts',(1.85792069011407,2.82398242685893,3.61997798186831E-16));
#13007=CARTESIAN_POINT('Ctrl Pts',(1.77822967842939,2.7313352228696,-2.48459787165829E-15));
#13008=CARTESIAN_POINT('Ctrl Pts',(1.70286389222234,2.63486608936521,-2.63677968348475E-15));
#13009=CARTESIAN_POINT('Ctrl Pts',(1.6781146665661,2.60318677605715,-2.68675437613003E-15));
#13010=CARTESIAN_POINT('Ctrl Pts',(1.65383227076774,2.5710952091118,-2.8599034388E-15));
#13011=CARTESIAN_POINT('Ctrl Pts',(1.63002677982222,2.53860449291447,-1.94289029309402E-16));
#13012=CARTESIAN_POINT('Ctrl Pts',(1.61755917530988,2.52158819189391,1.2749127461642E-15));
#13013=CARTESIAN_POINT('Ctrl Pts',(1.60522051376831,2.50445961085367,1.310626938495E-16));
#13014=CARTESIAN_POINT('Ctrl Pts',(1.59302690140008,2.48724166221798,-4.16333634234434E-17));
#13015=CARTESIAN_POINT('Ctrl Pts',(1.52372019925809,2.3893773705255,-1.0764802561769E-15));
#13016=CARTESIAN_POINT('Ctrl Pts',(1.458998168726,2.28849803957527,-1.59975950272218E-16));
#13017=CARTESIAN_POINT('Ctrl Pts',(1.39902498721045,2.18499850267992,-8.18789480661053E-16));
#13018=CARTESIAN_POINT('Ctrl Pts',(1.33917053664773,2.0817038673476,-1.476298735435E-15));
#13019=CARTESIAN_POINT('Ctrl Pts',(1.2840458525211,1.97579849696066,-2.5027159982132E-15));
#13020=CARTESIAN_POINT('Ctrl Pts',(1.23386201766705,1.86765533743376,-1.80411241501588E-15));
#13021=CARTESIAN_POINT('Ctrl Pts',(1.1847518022553,1.76182576352577,-1.12045456865919E-15));
#13022=CARTESIAN_POINT('Ctrl Pts',(1.14037317863941,1.65385230743519,-3.75898551344171E-16));
#13023=CARTESIAN_POINT('Ctrl Pts',(1.10097264016064,1.54407841972287,9.99200722162641E-16));
#13024=CARTESIAN_POINT('Ctrl Pts',(1.06978322653079,1.45718155684214,2.08772747025844E-15));
#13025=CARTESIAN_POINT('Ctrl Pts',(1.04171411204053,1.36915624453442,3.10028998944715E-15));
#13026=CARTESIAN_POINT('Ctrl Pts',(1.01691072758221,1.28017498851225,-9.43689570931383E-16));
#13027=CARTESIAN_POINT('Ctrl Pts',(1.01127765022899,1.25996652466321,-1.83529644040914E-15));
#13028=CARTESIAN_POINT('Ctrl Pts',(1.00581310158324,1.23970877167875,1.26058758656943E-15));
#13029=CARTESIAN_POINT('Ctrl Pts',(1.0005189403258,1.21940378536753,3.33066907387547E-16));
#13030=CARTESIAN_POINT('Ctrl Pts',(0.995361168747364,1.19962190185401,1.86042795644021E-17));
#13031=CARTESIAN_POINT('Ctrl Pts',(0.990366678191223,1.17980083040635,-4.01805598180605E-16));
#13032=CARTESIAN_POINT('Ctrl Pts',(0.985540360826723,1.15995762053482,-2.4980018054066E-16));
#13033=CARTESIAN_POINT('Ctrl Pts',(0.95842730415821,1.04848337773237,6.04128641609991E-16));
#13034=CARTESIAN_POINT('Ctrl Pts',(0.93658062937845,0.936170584254423,7.41469670808834E-16));
#13035=CARTESIAN_POINT('Ctrl Pts',(0.920192761507513,0.823356814344894,
5.55111512312578E-16));
#13036=CARTESIAN_POINT('Ctrl Pts',(0.904246281723449,0.713581551608195,
3.73772693226398E-16));
#13037=CARTESIAN_POINT('Ctrl Pts',(0.893468511491124,0.60333123086173,1.04581915629055E-15));
#13038=CARTESIAN_POINT('Ctrl Pts',(0.888084984187708,0.492918270951998,
7.21644966006352E-16));
#13039=CARTESIAN_POINT('Ctrl Pts',(0.882770527429912,0.38392190706839,4.01629923978879E-16));
#13040=CARTESIAN_POINT('Ctrl Pts',(0.882712683316618,0.27476643868936,2.31398886448546E-16));
#13041=CARTESIAN_POINT('Ctrl Pts',(0.888177025122092,0.165763420734776,
-5.55111512312578E-17));
#13042=CARTESIAN_POINT('Ctrl Pts',(0.893809155355859,0.0534133491527256,
2.12453188764699E-16));
#13043=CARTESIAN_POINT('Ctrl Pts',(0.905308962289794,-0.0587755777626049,
-8.65920908799369E-16));
#13044=CARTESIAN_POINT('Ctrl Pts',(0.922516988147342,-0.170434870117333,
8.88178419700125E-16));
#13045=CARTESIAN_POINT('Ctrl Pts',(0.92494514034144,-0.186190643496979,
1.10894341647542E-15));
#13046=CARTESIAN_POINT('Ctrl Pts',(0.92748542236121,-0.20192551582943,5.94353309524359E-16));
#13047=CARTESIAN_POINT('Ctrl Pts',(0.930136948334951,-0.21763816265144,
4.71844785465692E-16));
#13048=CARTESIAN_POINT('Ctrl Pts',(0.94852451933544,-0.326600855043117,
9.40525687969926E-16));
#13049=CARTESIAN_POINT('Ctrl Pts',(0.972258635131026,-0.434502143524435,
1.05264572258918E-15));
#13050=CARTESIAN_POINT('Ctrl Pts',(1.00109425852612,-0.541025619578607,
3.88578058618805E-16));
#13051=CARTESIAN_POINT('Ctrl Pts',(1.03041848882312,-0.649354088883701,
-1.43096128522812E-15));
#13052=CARTESIAN_POINT('Ctrl Pts',(1.06501902951245,-0.756258472851647,
2.29070670693008E-15));
#13053=CARTESIAN_POINT('Ctrl Pts',(1.10468717429828,-0.861384907347987,
1.77635683940025E-15));
#13054=CARTESIAN_POINT('Ctrl Pts',(1.14402738445883,-0.965642266718928,
2.1288356987997E-15));
#13055=CARTESIAN_POINT('Ctrl Pts',(1.18835237636573,-1.068151643539,-9.6169310269721E-16));
#13056=CARTESIAN_POINT('Ctrl Pts',(1.237498022929,-1.16853612940548,-5.55111512312578E-16));
#13057=CARTESIAN_POINT('Ctrl Pts',(1.27435271733458,-1.24381521938361,-8.96320816629977E-16));
#13058=CARTESIAN_POINT('Ctrl Pts',(1.31391921578064,-1.31789876864352,1.35933570826783E-15));
#13059=CARTESIAN_POINT('Ctrl Pts',(1.35613997129588,-1.39061245421914,2.1094237467878E-15));
#13060=CARTESIAN_POINT('Ctrl Pts',(1.37023011538891,-1.41487886761685,1.71588219329404E-15));
#13061=CARTESIAN_POINT('Ctrl Pts',(1.38461938163405,-1.43899786663544,1.51548447731389E-15));
#13062=CARTESIAN_POINT('Ctrl Pts',(1.39928390362746,-1.46292781003586,1.33226762955019E-15));
#13063=CARTESIAN_POINT('Ctrl Pts',(1.45676275832064,-1.55672328050179,6.14133443199526E-16));
#13064=CARTESIAN_POINT('Ctrl Pts',(1.51852300092247,-1.64771721479925,-1.19127808284468E-16));
#13065=CARTESIAN_POINT('Ctrl Pts',(1.58438368534009,-1.73555731024463,-5.55111512312578E-17));
#13066=CARTESIAN_POINT('Ctrl Pts',(1.65182969073821,-1.82551178921746,9.63681121344935E-18));
#13067=CARTESIAN_POINT('Ctrl Pts',(1.72357639497341,-1.91215970296754,2.66635203942124E-15));
#13068=CARTESIAN_POINT('Ctrl Pts',(1.79946346354604,-1.99507596845891,9.43689570931383E-16));
#13069=CARTESIAN_POINT('Ctrl Pts',(1.82652314050868,-2.02464210405154,3.29425628605202E-16));
#13070=CARTESIAN_POINT('Ctrl Pts',(1.85410952977247,-2.05373327548512,1.97952276092729E-15));
#13071=CARTESIAN_POINT('Ctrl Pts',(1.88221618809976,-2.08232847206164,1.94289029309402E-15));
#13072=CARTESIAN_POINT('Ctrl Pts',(1.90343708486131,-2.10391822162776,1.91523229800409E-15));
#13073=CARTESIAN_POINT('Ctrl Pts',(1.92495870310435,-2.12522891105285,6.33416430339438E-16));
#13074=CARTESIAN_POINT('Ctrl Pts',(1.94674902241761,-2.14622370228633,6.66133814775094E-16));
#13075=CARTESIAN_POINT('Ctrl Pts',(2.02283382172196,-2.21953077293877,7.80372417374885E-16));
#13076=CARTESIAN_POINT('Ctrl Pts',(2.10225777717469,-2.28905888221851,5.24876442197073E-16));
#13077=CARTESIAN_POINT('Ctrl Pts',(2.18487568646623,-2.35446233376722,2.77555756156289E-16));
#13078=CARTESIAN_POINT('Ctrl Pts',(2.26524307769197,-2.41808419037438,3.69721042132366E-17));
#13079=CARTESIAN_POINT('Ctrl Pts',(2.34863333307708,-2.47780335795739,-1.51150751606644E-15));
#13080=CARTESIAN_POINT('Ctrl Pts',(2.43493194849077,-2.53325667596464,-1.38777878078145E-15));
#13081=CARTESIAN_POINT('Ctrl Pts',(2.48398201129342,-2.56477501166252,-1.31745433574685E-15));
#13082=CARTESIAN_POINT('Ctrl Pts',(2.53397193040965,-2.59491440821501,-1.7272141774891E-15));
#13083=CARTESIAN_POINT('Ctrl Pts',(2.58488257447923,-2.62360084935056,-4.32986979603811E-15));
#13084=CARTESIAN_POINT('',(6.20516358154937,3.52286199445083,-5.04676743606953E-16));
#13085=CARTESIAN_POINT('Origin',(4.45646910621825,0.,0.));
#13086=CARTESIAN_POINT('Ctrl Pts',(6.37917532067248,3.40970963171683,-2.72004641033163E-15));
#13087=CARTESIAN_POINT('Ctrl Pts',(6.3222949445991,3.44902614310676,-3.07858945357474E-15));
#13088=CARTESIAN_POINT('Ctrl Pts',(6.26428052451075,3.48676815608406,-3.47743989805006E-15));
#13089=CARTESIAN_POINT('Ctrl Pts',(6.20516358154926,3.52286199445089,-3.88578058618805E-15));
#13090=CARTESIAN_POINT('Origin',(4.45646910621825,0.,0.));
#13091=CARTESIAN_POINT('',(8.38922139765086,0.00345161095399406,5.40416349472619));
#13092=CARTESIAN_POINT('Ctrl Pts',(8.38946759139483,0.00345189784424339,
5.40416349114816));
#13093=CARTESIAN_POINT('Ctrl Pts',(8.38934348094969,0.144859962266585,5.3970221751716));
#13094=CARTESIAN_POINT('Ctrl Pts',(8.38158931939786,0.285932740914827,5.38988085919504));
#13095=CARTESIAN_POINT('Ctrl Pts',(8.36633566017505,0.425948976110962,5.38273954321849));
#13096=CARTESIAN_POINT('Ctrl Pts',(8.35085549509945,0.568044351551121,5.37549218384331));
#13097=CARTESIAN_POINT('Ctrl Pts',(8.32765150846094,0.709051616527048,5.36824482446814));
#13098=CARTESIAN_POINT('Ctrl Pts',(8.29690900814658,0.848239565026732,5.36099746509296));
#13099=CARTESIAN_POINT('Ctrl Pts',(8.27698189787658,0.938460385377871,5.35629976881066));
#13100=CARTESIAN_POINT('Ctrl Pts',(8.25388842308756,1.02791726940828,5.35160207252836));
#13101=CARTESIAN_POINT('Ctrl Pts',(8.22768967185264,1.11641589263869,5.34690437624606));
#13102=CARTESIAN_POINT('Ctrl Pts',(8.19493248239052,1.22706873033696,5.34103068685625));
#13103=CARTESIAN_POINT('Ctrl Pts',(8.15724654742994,1.33646292603361,5.33515699746645));
#13104=CARTESIAN_POINT('Ctrl Pts',(8.11474561481755,1.44412672111228,5.32928330807664));
#13105=CARTESIAN_POINT('Ctrl Pts',(8.07229955490193,1.55165151211699,5.32341720217164));
#13106=CARTESIAN_POINT('Ctrl Pts',(8.02505101045592,1.6574499646389,5.31755109626664));
#13107=CARTESIAN_POINT('Ctrl Pts',(7.97316383541589,1.76106421848653,5.31168499036164));
#13108=CARTESIAN_POINT('Ctrl Pts',(7.92132979218209,1.86457237265819,5.30582489127436));
#13109=CARTESIAN_POINT('Ctrl Pts',(7.86486675018913,1.96590040970343,5.29996479218708));
#13110=CARTESIAN_POINT('Ctrl Pts',(7.80398685317266,2.06460987448604,5.2941046930998));
#13111=CARTESIAN_POINT('Ctrl Pts',(7.74091054835004,2.16688055158362,5.28803317500541));
#13112=CARTESIAN_POINT('Ctrl Pts',(7.67309283703732,2.26633972471172,5.28196165691101));
#13113=CARTESIAN_POINT('Ctrl Pts',(7.60082223596538,2.36252669729877,5.27589013881662));
#13114=CARTESIAN_POINT('Ctrl Pts',(7.53114837535926,2.45525759507398,5.27003677522061));
#13115=CARTESIAN_POINT('Ctrl Pts',(7.45733637921637,2.54494703243881,5.2641834116246));
#13116=CARTESIAN_POINT('Ctrl Pts',(7.37968871760434,2.63121190777325,5.2583300480286));
#13117=CARTESIAN_POINT('Ctrl Pts',(7.30205271452735,2.71746383072702,5.25247756329543));
#13118=CARTESIAN_POINT('Ctrl Pts',(7.22058246743452,2.80029190705686,5.24662507856226));
#13119=CARTESIAN_POINT('Ctrl Pts',(7.13561968331908,2.87934735404054,5.24077259382909));
#13120=CARTESIAN_POINT('Ctrl Pts',(7.05064910925681,2.95841004934754,5.23491957250164));
#13121=CARTESIAN_POINT('Ctrl Pts',(6.96218566408682,3.03369914624373,5.22906655117418));
#13122=CARTESIAN_POINT('Ctrl Pts',(6.87060620880603,3.10490435438986,5.22321352984672));
#13123=CARTESIAN_POINT('Ctrl Pts',(6.7789962100083,3.17613331084803,5.21735855642361));
#13124=CARTESIAN_POINT('Ctrl Pts',(6.6842684605794,3.24327541671102,5.21150358300051));
#13125=CARTESIAN_POINT('Ctrl Pts',(6.58683044030583,3.30606255025893,5.2056486095774));
#13126=CARTESIAN_POINT('Ctrl Pts',(6.48928198655146,3.36892084495818,5.19978700029395));
#13127=CARTESIAN_POINT('Ctrl Pts',(6.38901747841869,3.42741409186869,5.1939253910105));
#13128=CARTESIAN_POINT('Ctrl Pts',(6.28647081930378,3.48131910776706,5.18806378172705));
#13129=CARTESIAN_POINT('Ctrl Pts',(6.18385501222344,3.53526047221357,5.1821982199174));
#13130=CARTESIAN_POINT('Ctrl Pts',(6.07895436284824,3.58460726962324,5.17633265810775));
#13131=CARTESIAN_POINT('Ctrl Pts',(5.97222306208261,3.62918433608456,5.17046709629811));
#13132=CARTESIAN_POINT('Ctrl Pts',(5.86533569397726,3.67382658515048,5.16459295759845));
#13133=CARTESIAN_POINT('Ctrl Pts',(5.75661271854766,3.71368504222688,5.15871881889879));
#13134=CARTESIAN_POINT('Ctrl Pts',(5.646523851029,3.74863424520897,5.15284468019913));
#13135=CARTESIAN_POINT('Ctrl Pts',(5.61868417351413,3.75747232813555,5.15135920641089));
#13136=CARTESIAN_POINT('Ctrl Pts',(5.59075719728958,3.76599671884015,5.14987373262265));
#13137=CARTESIAN_POINT('Ctrl Pts',(5.5627506075966,3.77420590849361,5.14838825883441));
#13138=CARTESIAN_POINT('Ctrl Pts',(5.45201017581034,3.80666574086897,5.14251456944487));
#13139=CARTESIAN_POINT('Ctrl Pts',(5.33965547096268,3.83430158792593,5.13664088005533));
#13140=CARTESIAN_POINT('Ctrl Pts',(5.22614457931037,3.85695328803972,5.13076719066579));
#13141=CARTESIAN_POINT('Ctrl Pts',(5.11278024088333,3.87957574268059,5.12490108476107));
#13142=CARTESIAN_POINT('Ctrl Pts',(4.9982630856897,3.89722676737455,5.11903497885635));
#13143=CARTESIAN_POINT('Ctrl Pts',(4.88306668401858,3.90979583950555,5.11316887295164));
#13144=CARTESIAN_POINT('Ctrl Pts',(4.76798824199548,3.92235204106678,5.10730877386465));
#13145=CARTESIAN_POINT('Ctrl Pts',(4.65223234524747,3.9298365964174,5.10144867477766));
#13146=CARTESIAN_POINT('Ctrl Pts',(4.53628243620288,3.93219008090361,5.09558857569067));
#13147=CARTESIAN_POINT('Ctrl Pts',(4.41614931893485,3.93462847374153,5.08951705759617));
#13148=CARTESIAN_POINT('Ctrl Pts',(4.29580836896058,3.93155848245691,5.08344553950168));
#13149=CARTESIAN_POINT('Ctrl Pts',(4.17580312088828,3.92297280192952,5.07737402140718));
#13150=CARTESIAN_POINT('Ctrl Pts',(4.06010975731343,3.91469561176703,5.07152065781149));
#13151=CARTESIAN_POINT('Ctrl Pts',(3.9447288341557,3.90129230922499,5.0656672942158));
#13152=CARTESIAN_POINT('Ctrl Pts',(3.83014624661306,3.88280937924282,5.05981393062012));
#13153=CARTESIAN_POINT('Ctrl Pts',(3.71558086326044,3.8643292244104,5.05396144588728));
#13154=CARTESIAN_POINT('Ctrl Pts',(3.60181398494459,3.84077102442487,5.04810896115444));
#13155=CARTESIAN_POINT('Ctrl Pts',(3.48932393913495,3.812232839923,5.04225647642161));
#13156=CARTESIAN_POINT('Ctrl Pts',(3.37682357949849,3.7836920388528,5.0364034550945));
#13157=CARTESIAN_POINT('Ctrl Pts',(3.26560068557013,3.75017044719279,5.03055043376739));
#13158=CARTESIAN_POINT('Ctrl Pts',(3.15612029668761,3.71181653285184,5.02469741244029));
#13159=CARTESIAN_POINT('Ctrl Pts',(3.04660339398123,3.6734498267398,5.01884243901754));
#13160=CARTESIAN_POINT('Ctrl Pts',(2.93883054162971,3.6302477297295,5.01298746559479));
#13161=CARTESIAN_POINT('Ctrl Pts',(2.83324794308609,3.58240729894856,5.00713249217205));
#13162=CARTESIAN_POINT('Ctrl Pts',(2.72754568022847,3.53451264718414,5.00127088288896));
#13163=CARTESIAN_POINT('Ctrl Pts',(2.62403900236968,3.48196933969022,4.99540927360588));
#13164=CARTESIAN_POINT('Ctrl Pts',(2.52315067528165,3.42502099914743,4.98954766432279));
#13165=CARTESIAN_POINT('Ctrl Pts',(2.42219431845377,3.3680342579204,4.98368210251352));
#13166=CARTESIAN_POINT('Ctrl Pts',(2.32386017762171,3.30663678729406,4.97781654070425));
#13167=CARTESIAN_POINT('Ctrl Pts',(2.22854166560395,3.24111528942705,4.97195097889498));
#13168=CARTESIAN_POINT('Ctrl Pts',(2.13308377454302,3.17549798305983,4.96607684019571));
#13169=CARTESIAN_POINT('Ctrl Pts',(2.04065064124075,3.10574486231773,4.96020270149644));
#13170=CARTESIAN_POINT('Ctrl Pts',(1.95160232958478,3.03218261839848,4.95432856279716));
#13171=CARTESIAN_POINT('Ctrl Pts',(1.92908346513302,3.01357992769296,4.95284308900569));
#13172=CARTESIAN_POINT('Ctrl Pts',(1.90678087325711,2.99473382365849,4.95135761521422));
#13173=CARTESIAN_POINT('Ctrl Pts',(1.88469998808044,2.97564994631302,4.94987214142275));
#13174=CARTESIAN_POINT('Ctrl Pts',(1.79739029480277,2.90019067625882,4.94399845202725));
#13175=CARTESIAN_POINT('Ctrl Pts',(1.7132591214716,2.82075979155518,4.93812476263176));
#13176=CARTESIAN_POINT('Ctrl Pts',(1.63268938607396,2.73765540053927,4.93225107323626));
#13177=CARTESIAN_POINT('Ctrl Pts',(1.5522236737737,2.65465830509925,4.92638496732557));
#13178=CARTESIAN_POINT('Ctrl Pts',(1.47531054014492,2.56799742922099,4.92051886141487));
#13179=CARTESIAN_POINT('Ctrl Pts',(1.40229958516729,2.47801080237423,4.91465275550418));
#13180=CARTESIAN_POINT('Ctrl Pts',(1.32936339247731,2.38811632068681,4.90879265641119));
#13181=CARTESIAN_POINT('Ctrl Pts',(1.26032168925582,2.29490318082625,4.90293255731821));
#13182=CARTESIAN_POINT('Ctrl Pts',(1.19548648924436,2.19874540858966,4.89707245822522));
#13183=CARTESIAN_POINT('Ctrl Pts',(1.12831218320644,2.09911848341626,4.89100094013297));
#13184=CARTESIAN_POINT('Ctrl Pts',(1.06565394748279,1.99633076737082,4.88492942204071));
#13185=CARTESIAN_POINT('Ctrl Pts',(1.00781257590287,1.89083503667377,4.87885790394846));
#13186=CARTESIAN_POINT('Ctrl Pts',(0.952049490965552,1.78912985177413,4.87300454034678));
#13187=CARTESIAN_POINT('Ctrl Pts',(0.900763295417265,1.68490829873013,4.86715117674511));
#13188=CARTESIAN_POINT('Ctrl Pts',(0.854178336007027,1.57860387901811,4.86129781314343));
#13189=CARTESIAN_POINT('Ctrl Pts',(0.807600371171798,1.47231542055725,4.85544532840462));
#13190=CARTESIAN_POINT('Ctrl Pts',(0.765722404711504,1.3639450955676,4.84959284366581));
#13191=CARTESIAN_POINT('Ctrl Pts',(0.728721341374304,1.2539480059799,4.84374035892699));
#13192=CARTESIAN_POINT('Ctrl Pts',(0.691716885536518,1.14394083113633,4.83788733759393));
#13193=CARTESIAN_POINT('Ctrl Pts',(0.659590353436437,1.03230698679914,4.83203431626086));
#13194=CARTESIAN_POINT('Ctrl Pts',(0.632469088573365,0.919517735039361,
4.8261812949278));
#13195=CARTESIAN_POINT('Ctrl Pts',(0.60533877824483,0.806690865886492,4.82032632149911));
#13196=CARTESIAN_POINT('Ctrl Pts',(0.583217151127083,0.69270822453654,4.81447134807043));
#13197=CARTESIAN_POINT('Ctrl Pts',(0.566180509705361,0.578051585796435,
4.80861637464174));
#13198=CARTESIAN_POINT('Ctrl Pts',(0.549124559439059,0.463264998484746,
4.80275476535279));
#13199=CARTESIAN_POINT('Ctrl Pts',(0.537165158581018,0.347803297992415,
4.79689315606384));
#13200=CARTESIAN_POINT('Ctrl Pts',(0.53032677442703,0.232153807888215,4.79103154677488));
#13201=CARTESIAN_POINT('Ctrl Pts',(0.523483779100426,0.11642633448417,4.78516598495977));
#13202=CARTESIAN_POINT('Ctrl Pts',(0.521768682541085,0.000511231401446904,
4.77930042314466));
#13203=CARTESIAN_POINT('Ctrl Pts',(0.525153839506122,-0.115105489513525,
4.77343486132955));
#13204=CARTESIAN_POINT('Ctrl Pts',(0.528543946400855,-0.230891270429573,
4.76756072262453));
#13205=CARTESIAN_POINT('Ctrl Pts',(0.537049160528772,-0.346377387971861,
4.76168658391951));
#13206=CARTESIAN_POINT('Ctrl Pts',(0.550590154771058,-0.461084175223764,
4.75581244521449));
#13207=CARTESIAN_POINT('Ctrl Pts',(0.554014451045886,-0.490091648180038,
4.75432697148003));
#13208=CARTESIAN_POINT('Ctrl Pts',(0.557760532846793,-0.519049342278175,
4.75284149774556));
#13209=CARTESIAN_POINT('Ctrl Pts',(0.561826606712647,-0.547949633675161,
4.7513560240111));
#13210=CARTESIAN_POINT('Ctrl Pts',(0.577904208319941,-0.662223841853587,
4.74548233462701));
#13211=CARTESIAN_POINT('Ctrl Pts',(0.599042294759102,-0.775980164860141,
4.73960864524293));
#13212=CARTESIAN_POINT('Ctrl Pts',(0.62519794673883,-0.888735226342029,
4.73373495585884));
#13213=CARTESIAN_POINT('Ctrl Pts',(0.651319829314674,-1.00134471044683,
4.72786884995955));
#13214=CARTESIAN_POINT('Ctrl Pts',(0.682446302012626,-1.11295510504555,
4.72200274406025));
#13215=CARTESIAN_POINT('Ctrl Pts',(0.718482837491725,-1.2230893895427,4.71613663816096));
#13216=CARTESIAN_POINT('Ctrl Pts',(0.754482472017684,-1.3331108979359,4.71027653907936));
#13217=CARTESIAN_POINT('Ctrl Pts',(0.795382040814186,-1.4416589124362,4.70441643999776));
#13218=CARTESIAN_POINT('Ctrl Pts',(0.841036392686699,-1.54826848250744,
4.69855634091616));
#13219=CARTESIAN_POINT('Ctrl Pts',(0.888337849491357,-1.65872428281689,
4.69248482281963));
#13220=CARTESIAN_POINT('Ctrl Pts',(0.940743548349913,-1.76709868859664,
4.6864133047231));
#13221=CARTESIAN_POINT('Ctrl Pts',(0.998036081046421,-1.87289348613337,
4.68034178662657));
#13222=CARTESIAN_POINT('Ctrl Pts',(1.05327004717428,-1.97488699189445,4.67448842303615));
#13223=CARTESIAN_POINT('Ctrl Pts',(1.11304550150352,-2.0744826794852,4.66863505944574));
#13224=CARTESIAN_POINT('Ctrl Pts',(1.17711978984902,-2.17125702329979,4.66278169585532));
#13225=CARTESIAN_POINT('Ctrl Pts',(1.24118445765626,-2.2680168367731,4.65692921112771));
#13226=CARTESIAN_POINT('Ctrl Pts',(1.30954644805187,-2.36195580438726,4.65107672640009));
#13227=CARTESIAN_POINT('Ctrl Pts',(1.38191923705951,-2.45267855661029,4.64522424167247));
#13228=CARTESIAN_POINT('Ctrl Pts',(1.45429866168086,-2.54340962689245,4.63937122035053));
#13229=CARTESIAN_POINT('Ctrl Pts',(1.53068935828223,-2.63092357259591,4.63351819902859));
#13230=CARTESIAN_POINT('Ctrl Pts',(1.61076435577023,-2.71485791032929,4.62766517770664));
#13231=CARTESIAN_POINT('Ctrl Pts',(1.69086605981718,-2.79882024178618,4.62181020428899));
#13232=CARTESIAN_POINT('Ctrl Pts',(1.77465422310562,-2.87920029255102,4.61595523087134));
#13233=CARTESIAN_POINT('Ctrl Pts',(1.86176537078853,-2.955672770343,4.61010025745369));
#13234=CARTESIAN_POINT('Ctrl Pts',(1.94897524777021,-3.03223191986768,4.60423864817558));
#13235=CARTESIAN_POINT('Ctrl Pts',(2.03951531555244,-3.10487438422178,4.59837703889748));
#13236=CARTESIAN_POINT('Ctrl Pts',(2.13298933627094,-3.17331542060439,4.59251542961937));
#13237=CARTESIAN_POINT('Ctrl Pts',(2.22652638720913,-3.24180260728122,4.58664986781502));
#13238=CARTESIAN_POINT('Ctrl Pts',(2.32300098752248,-3.30608249623343,4.58078430601067));
#13239=CARTESIAN_POINT('Ctrl Pts',(2.42198975089452,-3.3659148463325,4.57491874420632));
#13240=CARTESIAN_POINT('Ctrl Pts',(2.52112326011971,-3.42583468600379,4.56904460551183));
#13241=CARTESIAN_POINT('Ctrl Pts',(2.62277790813312,-3.4812938105796,4.56317046681735));
#13242=CARTESIAN_POINT('Ctrl Pts',(2.72650762307617,-3.53209884726416,4.55729632812286));
#13243=CARTESIAN_POINT('Ctrl Pts',(2.75273917566813,-3.54494661217376,4.55581085428172));
#13244=CARTESIAN_POINT('Ctrl Pts',(2.77910334170824,-3.55749699254563,4.55432538044058));
#13245=CARTESIAN_POINT('Ctrl Pts',(2.80559274256743,-3.56974736248086,4.55283990659944));
#13246=CARTESIAN_POINT('Ctrl Pts',(2.91033407718839,-3.6181863627979,4.54696621721354));
#13247=CARTESIAN_POINT('Ctrl Pts',(3.01738356579454,-3.66209224752273,4.54109252782763));
#13248=CARTESIAN_POINT('Ctrl Pts',(3.12631175648758,-3.70123903915398,4.53521883844173));
#13249=CARTESIAN_POINT('Ctrl Pts',(3.23509931065145,-3.74033528859897,4.52935273254072));
#13250=CARTESIAN_POINT('Ctrl Pts',(3.34576035796865,-3.77468452576842,4.52348662663971));
#13251=CARTESIAN_POINT('Ctrl Pts',(3.45784281011898,-3.80410758532656,4.51762052073871));
#13252=CARTESIAN_POINT('Ctrl Pts',(3.56981049126493,-3.83350051604621,4.51176042165547));
#13253=CARTESIAN_POINT('Ctrl Pts',(3.68319628490271,-3.85797719849322,4.50590032257224));
#13254=CARTESIAN_POINT('Ctrl Pts',(3.79753080160516,-3.87740755024715,4.50004022348901));
#13255=CARTESIAN_POINT('Ctrl Pts',(3.91599024696327,-3.89753890478704,4.49396870539313));
#13256=CARTESIAN_POINT('Ctrl Pts',(4.03546773832967,-3.91225278090741,4.48789718729724));
#13257=CARTESIAN_POINT('Ctrl Pts',(4.15542676375039,-3.92146178204524,4.48182566920136));
#13258=CARTESIAN_POINT('Ctrl Pts',(4.27107556538731,-3.93033989640244,4.47597230560955));
#13259=CARTESIAN_POINT('Ctrl Pts',(4.38717144554922,-3.93410188254922,4.47011894201775));
#13260=CARTESIAN_POINT('Ctrl Pts',(4.50322696720433,-3.93272204744195,4.46426557842595));
#13261=CARTESIAN_POINT('Ctrl Pts',(4.61926506351249,-3.93134241951228,4.45841309369704));
#13262=CARTESIAN_POINT('Ctrl Pts',(4.73526240035798,-3.924822510319,4.45256060896812));
#13263=CARTESIAN_POINT('Ctrl Pts',(4.85073141824768,-3.91318875462368,4.44670812423921));
#13264=CARTESIAN_POINT('Ctrl Pts',(4.96621102309533,-3.90155393226923,4.44085510291606));
#13265=CARTESIAN_POINT('Ctrl Pts',(5.08116180160703,-3.88480437275884,4.43500208159291));
#13266=CARTESIAN_POINT('Ctrl Pts',(5.19510190200478,-3.86301832677358,4.42914906026976));
#13267=CARTESIAN_POINT('Ctrl Pts',(5.30908000362576,-3.84122501472138,4.423294086851));
#13268=CARTESIAN_POINT('Ctrl Pts',(5.42204635128827,-3.81439195360396,4.41743911343223));
#13269=CARTESIAN_POINT('Ctrl Pts',(5.53353055616425,-3.78264823014779,4.41158414001347));
#13270=CARTESIAN_POINT('Ctrl Pts',(5.64514111406658,-3.75086852925848,4.4057225307344));
#13271=CARTESIAN_POINT('Ctrl Pts',(5.75526577879248,-3.71416717062201,4.39986092145532));
#13272=CARTESIAN_POINT('Ctrl Pts',(5.86345047441672,-3.6727227542441,4.39399931217625));
#13273=CARTESIAN_POINT('Ctrl Pts',(5.97170811977554,-3.63125039159192,4.388133750371));
#13274=CARTESIAN_POINT('Ctrl Pts',(6.07802281329685,-3.5850287670336,4.38226818856575));
#13275=CARTESIAN_POINT('Ctrl Pts',(6.18196315672575,-3.53428341841217,4.37640262676049));
#13276=CARTESIAN_POINT('Ctrl Pts',(6.2860554864301,-3.48346386764478,4.37052848806524));
#13277=CARTESIAN_POINT('Ctrl Pts',(6.38776617555163,-3.42810758808792,4.36465434936999));
#13278=CARTESIAN_POINT('Ctrl Pts',(6.48669091161503,-3.36848458819265,4.35878021067474));
#13279=CARTESIAN_POINT('Ctrl Pts',(6.51170736323199,-3.3534069043747,4.35729473684576));
#13280=CARTESIAN_POINT('Ctrl Pts',(6.53654581130273,-3.33805656945364,4.35580926301677));
#13281=CARTESIAN_POINT('Ctrl Pts',(6.56120004923896,-3.32243836022448,4.35432378918779));
#13282=CARTESIAN_POINT('Ctrl Pts',(6.65867343535823,-3.2606899605123,4.34845079629802));
#13283=CARTESIAN_POINT('Ctrl Pts',(6.75358948814569,-3.19454559946926,4.34257780340824));
#13284=CARTESIAN_POINT('Ctrl Pts',(6.84552565595133,-3.12424355679538,4.33670481051846));
#13285=CARTESIAN_POINT('Ctrl Pts',(6.93735750783295,-3.05402128275573,4.33083848145528));
#13286=CARTESIAN_POINT('Ctrl Pts',(7.02621586872288,-2.97965095039595,4.3249721523921));
#13287=CARTESIAN_POINT('Ctrl Pts',(7.11170505525854,-2.90141535374102,4.31910582332892));
#13288=CARTESIAN_POINT('Ctrl Pts',(7.19709978829401,-2.82326619639196,4.3132459757324));
#13289=CARTESIAN_POINT('Ctrl Pts',(7.27913245113307,-2.74126054982594,4.30738612813589));
#13290=CARTESIAN_POINT('Ctrl Pts',(7.35743931745999,-2.6557222809413,4.30152628053938));
#13291=CARTESIAN_POINT('Ctrl Pts',(7.38606210988018,-2.62445626010418,4.29938438405908));
#13292=CARTESIAN_POINT('Ctrl Pts',(7.41418743616012,-2.59271864890061,4.29724248757878));
#13293=CARTESIAN_POINT('Ctrl Pts',(7.44179868886595,-2.56052656361313,4.29510059109848));
#13294=CARTESIAN_POINT('',(8.38744148431105,-0.00176345638553475,6.65416354772551));
#13295=CARTESIAN_POINT('Ctrl Pts',(8.38378142039597,-0.00176130459896508,
6.65416352203495));
#13296=CARTESIAN_POINT('Ctrl Pts',(8.38067961832936,0.766306874467471,6.61544270826197));
#13297=CARTESIAN_POINT('Ctrl Pts',(7.79186236069236,2.85135882026889,6.51054985535175));
#13298=CARTESIAN_POINT('Ctrl Pts',(4.40556007854754,4.64877272666142,6.33948496330435));
#13299=CARTESIAN_POINT('Ctrl Pts',(0.522470636039735,2.4773646541884,6.14096884589269));
#13300=CARTESIAN_POINT('Ctrl Pts',(0.242062159932001,-1.96276684409906,
5.94245272848103));
#13301=CARTESIAN_POINT('Ctrl Pts',(3.82112739871976,-4.60543380238081,5.74393661106939));
#13302=CARTESIAN_POINT('Ctrl Pts',(7.58197580057618,-3.18195140949412,5.56450687558735));
#13303=CARTESIAN_POINT('Ctrl Pts',(8.37950088367395,-0.928416374988517,
5.45124917924254));
#13304=CARTESIAN_POINT('Ctrl Pts',(8.38734236653861,0.00344942131385295,
5.40416352203495));
#13305=CARTESIAN_POINT('',(8.39081119622603,-0.00254965045452874,7.90416352203496));
#13306=CARTESIAN_POINT('Ctrl Pts',(8.38946828034982,-0.00254878017787342,
7.90416352203496));
#13307=CARTESIAN_POINT('Ctrl Pts',(8.38954213717047,0.111418998272305,7.89837421661825));
#13308=CARTESIAN_POINT('Ctrl Pts',(8.38465808761385,0.225581875715186,7.89258491120154));
#13309=CARTESIAN_POINT('Ctrl Pts',(8.37479171694471,0.339465636360686,7.88679560578483));
#13310=CARTESIAN_POINT('Ctrl Pts',(8.36493650012569,0.453220652360487,7.88101284512981));
#13311=CARTESIAN_POINT('Ctrl Pts',(8.35011019437028,0.566696758242774,7.8752300844748));
#13312=CARTESIAN_POINT('Ctrl Pts',(8.33034040981158,0.679418959991637,7.86944732381978));
#13313=CARTESIAN_POINT('Ctrl Pts',(8.31034793917893,0.793410860177514,7.86359942637671));
#13314=CARTESIAN_POINT('Ctrl Pts',(8.28529991712303,0.906631325987264,7.85775152893363));
#13315=CARTESIAN_POINT('Ctrl Pts',(8.25527900904773,1.01859330557622,7.85190363149055));
#13316=CARTESIAN_POINT('Ctrl Pts',(8.2256318969392,1.12916122552193,7.84612854731724));
#13317=CARTESIAN_POINT('Ctrl Pts',(8.19113515060747,1.23850139940321,7.84035346314393));
#13318=CARTESIAN_POINT('Ctrl Pts',(8.15191972961016,1.34615515081744,7.83457837897062));
#13319=CARTESIAN_POINT('Ctrl Pts',(8.11271233818502,1.45378685953663,7.82880447727741));
#13320=CARTESIAN_POINT('Ctrl Pts',(8.06878833770282,1.55973243241917,7.8230305755842));
#13321=CARTESIAN_POINT('Ctrl Pts',(8.02032802247892,1.66355000675945,7.81725667389099));
#13322=CARTESIAN_POINT('Ctrl Pts',(7.97186515694209,1.76737304468989,7.81148246833563));
#13323=CARTESIAN_POINT('Ctrl Pts',(7.91886568300501,1.86906747635069,7.80570826278026));
#13324=CARTESIAN_POINT('Ctrl Pts',(7.86155696974341,1.96821382011043,7.79993405722489));
#13325=CARTESIAN_POINT('Ctrl Pts',(7.80296975279677,2.06957202588276,7.79403103455498));
#13326=CARTESIAN_POINT('Ctrl Pts',(7.73987896152691,2.16826669075738,7.78812801188507));
#13327=CARTESIAN_POINT('Ctrl Pts',(7.67257493907625,2.26387991551159,7.78222498921515));
#13328=CARTESIAN_POINT('Ctrl Pts',(7.60664614522057,2.35753946742498,7.77644258349022));
#13329=CARTESIAN_POINT('Ctrl Pts',(7.53667497002743,2.44824200393647,7.77066017776528));
#13330=CARTESIAN_POINT('Ctrl Pts',(7.46297497751559,2.53562841241665,7.76487777204034));
#13331=CARTESIAN_POINT('Ctrl Pts',(7.38696898944648,2.62574905007182,7.75891444089794));
#13332=CARTESIAN_POINT('Ctrl Pts',(7.30699734734518,2.71234227061884,7.75295110975554));
#13333=CARTESIAN_POINT('Ctrl Pts',(7.22344370650432,2.79505645048034,7.74698777861314));
#13334=CARTESIAN_POINT('Ctrl Pts',(7.13989006566346,2.87777063034184,7.74102444747074));
#13335=CARTESIAN_POINT('Ctrl Pts',(7.05275483757312,2.95660549722653,7.73506111632834));
#13336=CARTESIAN_POINT('Ctrl Pts',(6.96245617822768,3.03125680121655,7.72909778518594));
#13337=CARTESIAN_POINT('Ctrl Pts',(6.87351490283744,3.10478593481108,7.72322409579537));
#13338=CARTESIAN_POINT('Ctrl Pts',(6.78118658365038,3.17451972307124,7.71735040640481));
#13339=CARTESIAN_POINT('Ctrl Pts',(6.68582891585312,3.24013021947958,7.71147671701425));
#13340=CARTESIAN_POINT('Ctrl Pts',(6.59059436376342,3.30565600657324,7.70561061110849));
#13341=CARTESIAN_POINT('Ctrl Pts',(6.49233857835877,3.36706885657886,7.69974450520274));
#13342=CARTESIAN_POINT('Ctrl Pts',(6.39145307221303,3.42408032197598,7.69387839929699));
#13343=CARTESIAN_POINT('Ctrl Pts',(6.29067087154033,3.48103340835884,7.68801830020895));
#13344=CARTESIAN_POINT('Ctrl Pts',(6.18726466387726,3.53359387279993,7.68215820112091));
#13345=CARTESIAN_POINT('Ctrl Pts',(6.08165519858878,3.58151632205766,7.67629810203288));
#13346=CARTESIAN_POINT('Ctrl Pts',(5.97223558472645,3.631167703956,7.67022658393877));
#13347=CARTESIAN_POINT('Ctrl Pts',(5.86045110676504,3.67583983813407,7.66415506584466));
#13348=CARTESIAN_POINT('Ctrl Pts',(5.74679829771543,3.71531150478264,7.65808354775055));
#13349=CARTESIAN_POINT('Ctrl Pts',(5.63722912492401,3.75336492290356,7.6522301841538));
#13350=CARTESIAN_POINT('Ctrl Pts',(5.52592399542495,3.78658500868859,7.64637682055705));
#13351=CARTESIAN_POINT('Ctrl Pts',(5.41334770981636,3.814822713833,7.6405234569603));
#13352=CARTESIAN_POINT('Ctrl Pts',(5.30078832715837,3.84305617918096,7.6346709722264));
#13353=CARTESIAN_POINT('Ctrl Pts',(5.18695856851517,3.86630865087859,7.6288184874925));
#13354=CARTESIAN_POINT('Ctrl Pts',(5.07233663553888,3.88448145655614,7.62296600275861));
#13355=CARTESIAN_POINT('Ctrl Pts',(4.95770419327007,3.90265592843602,7.61711298143043));
#13356=CARTESIAN_POINT('Ctrl Pts',(4.84227984035374,3.91574974375605,7.61125996010225));
#13357=CARTESIAN_POINT('Ctrl Pts',(4.72654946229429,3.92371579007219,7.60540693877406));
#13358=CARTESIAN_POINT('Ctrl Pts',(4.61078048591883,3.93168449321862,7.59955196535024));
#13359=CARTESIAN_POINT('Ctrl Pts',(4.49470569339517,3.93452199832943,7.59369699192642));
#13360=CARTESIAN_POINT('Ctrl Pts',(4.37881283913662,3.93223327184222,7.58784201850259));
#13361=CARTESIAN_POINT('Ctrl Pts',(4.26278863521375,3.92994195137751,7.58198040921844));
#13362=CARTESIAN_POINT('Ctrl Pts',(4.14694719442151,3.92251281121624,7.57611879993429));
#13363=CARTESIAN_POINT('Ctrl Pts',(4.03177311316667,3.91000285338591,7.57025719065014));
#13364=CARTESIAN_POINT('Ctrl Pts',(3.91652136918324,3.89748445999917,7.56439162883981));
#13365=CARTESIAN_POINT('Ctrl Pts',(3.80193828813998,3.87987848954146,7.55852606702948));
#13366=CARTESIAN_POINT('Ctrl Pts',(3.6884984975159,3.85729311100017,7.55266050521916));
#13367=CARTESIAN_POINT('Ctrl Pts',(3.5748928300947,3.83467470709597,7.54678636651883));
#13368=CARTESIAN_POINT('Ctrl Pts',(3.4624341892126,3.80706246196692,7.54091222781849));
#13369=CARTESIAN_POINT('Ctrl Pts',(3.35158234214481,3.77461444899679,7.53503808911816));
#13370=CARTESIAN_POINT('Ctrl Pts',(3.3235497196911,3.76640887623436,7.53355261533687));
#13371=CARTESIAN_POINT('Ctrl Pts',(3.29561975116823,3.75789429531127,7.53206714155557));
#13372=CARTESIAN_POINT('Ctrl Pts',(3.26779965546345,3.74907374385225,7.53058166777428));
#13373=CARTESIAN_POINT('Ctrl Pts',(3.15779663619547,3.71419653485921,7.52470797838371));
#13374=CARTESIAN_POINT('Ctrl Pts',(3.04914672673835,3.67441567358155,7.51883428899315));
#13375=CARTESIAN_POINT('Ctrl Pts',(2.94231941308688,3.62985395116528,7.51296059960258));
#13376=CARTESIAN_POINT('Ctrl Pts',(2.83563002353313,3.58534976211896,7.50709449369682));
#13377=CARTESIAN_POINT('Ctrl Pts',(2.73075892797452,3.53607714469623,7.50122838779105));
#13378=CARTESIAN_POINT('Ctrl Pts',(2.62816075381596,3.48220871984091,7.49536228188529));
#13379=CARTESIAN_POINT('Ctrl Pts',(2.52566763888122,3.42839545556665,7.48950218279727));
#13380=CARTESIAN_POINT('Ctrl Pts',(2.42544317948749,3.3699959354944,7.48364208370925));
#13381=CARTESIAN_POINT('Ctrl Pts',(2.32792167373385,3.30723068860702,7.47778198462123));
#13382=CARTESIAN_POINT('Ctrl Pts',(2.22688181453445,3.24220101480218,7.47171046652713));
#13383=CARTESIAN_POINT('Ctrl Pts',(2.12874404094721,3.1724848295905,7.46563894843301));
#13384=CARTESIAN_POINT('Ctrl Pts',(2.03396342098152,3.09837944819477,7.45956743033891));
#13385=CARTESIAN_POINT('Ctrl Pts',(1.94258834443801,3.02693673237616,7.45371406674216));
#13386=CARTESIAN_POINT('Ctrl Pts',(1.85433367634259,2.95141508308456,7.44786070314541));
#13387=CARTESIAN_POINT('Ctrl Pts',(1.76957663598028,2.87212427540636,7.44200733954866));
#13388=CARTESIAN_POINT('Ctrl Pts',(1.68483232160248,2.79284537297621,7.43615485481476));
#13389=CARTESIAN_POINT('Ctrl Pts',(1.60358489237179,2.70979871960467,7.43030237008087));
#13390=CARTESIAN_POINT('Ctrl Pts',(1.5261765011186,2.62333266066245,7.42444988534698));
#13391=CARTESIAN_POINT('Ctrl Pts',(1.44876101255519,2.53685867394349,7.4185968640188));
#13392=CARTESIAN_POINT('Ctrl Pts',(1.37518553727407,2.44696496624988,7.41274384269063));
#13393=CARTESIAN_POINT('Ctrl Pts',(1.30575306738485,2.35403429087981,7.40689082136246));
#13394=CARTESIAN_POINT('Ctrl Pts',(1.23629744042602,2.26107262133479,7.40103584793864));
#13395=CARTESIAN_POINT('Ctrl Pts',(1.17098781359953,2.16507230082266,7.39518087451482));
#13396=CARTESIAN_POINT('Ctrl Pts',(1.11008442987535,2.06644588555749,7.389325901091));
#13397=CARTESIAN_POINT('Ctrl Pts',(1.04911201998847,1.96770768991868,7.38346429180684));
#13398=CARTESIAN_POINT('Ctrl Pts',(0.992556037941512,1.86633781064936,7.37760268252269));
#13399=CARTESIAN_POINT('Ctrl Pts',(0.94063128880457,1.76277435925413,7.37174107323854));
#13400=CARTESIAN_POINT('Ctrl Pts',(0.888671526427721,1.6591410742626,7.36587551142817));
#13401=CARTESIAN_POINT('Ctrl Pts',(0.84134938352646,1.55331164806864,7.3600099496178));
#13402=CARTESIAN_POINT('Ctrl Pts',(0.798831264922408,1.44574355330421,7.35414438780743));
#13403=CARTESIAN_POINT('Ctrl Pts',(0.756250974400965,1.33801816760309,7.34827024910711));
#13404=CARTESIAN_POINT('Ctrl Pts',(0.718488861844663,1.22854942847929,7.34239611040679));
#13405=CARTESIAN_POINT('Ctrl Pts',(0.685661341161439,1.11780937506681,7.33652197170647));
#13406=CARTESIAN_POINT('Ctrl Pts',(0.677359797093927,1.08980502340366,7.33503649792519));
#13407=CARTESIAN_POINT('Ctrl Pts',(0.669373564680903,1.06171941638128,7.3335510241439));
#13408=CARTESIAN_POINT('Ctrl Pts',(0.661704004809934,1.0335602668125,7.33206555036262));
#13409=CARTESIAN_POINT('Ctrl Pts',(0.63137791423059,0.922216599792919,7.32619186097206));
#13410=CARTESIAN_POINT('Ctrl Pts',(0.605905934843882,0.809351645023374,
7.3203181715815));
#13411=CARTESIAN_POINT('Ctrl Pts',(0.585439397109298,0.69542648151754,7.31444448219094));
#13412=CARTESIAN_POINT('Ctrl Pts',(0.564999283597626,0.581648406100308,
7.30857837628518));
#13413=CARTESIAN_POINT('Ctrl Pts',(0.549551832338061,0.466813247020311,
7.30271227037941));
#13414=CARTESIAN_POINT('Ctrl Pts',(0.539198446437092,0.351396610708885,
7.29684616447365));
#13415=CARTESIAN_POINT('Ctrl Pts',(0.528855662271394,0.236098159562734,
7.2909860653856));
#13416=CARTESIAN_POINT('Ctrl Pts',(0.523596604588073,0.120219824582288,
7.28512596629756));
#13417=CARTESIAN_POINT('Ctrl Pts',(0.523471398282406,0.00424610072730045,
7.27926586720951));
#13418=CARTESIAN_POINT('Ctrl Pts',(0.523341674818871,-0.115911690505769,
7.27319434911541));
#13419=CARTESIAN_POINT('Ctrl Pts',(0.528723311878636,-0.23617143883278,
7.2671228310213));
#13420=CARTESIAN_POINT('Ctrl Pts',(0.539613169842923,-0.355989569624379,
7.2610513129272));
#13421=CARTESIAN_POINT('Ctrl Pts',(0.550111746507598,-0.471502539220414,
7.25519794933045));
#13422=CARTESIAN_POINT('Ctrl Pts',(0.565729486075797,-0.586604633741501,
7.24934458573369));
#13423=CARTESIAN_POINT('Ctrl Pts',(0.586410576273707,-0.700810940841733,
7.24349122213694));
#13424=CARTESIAN_POINT('Ctrl Pts',(0.607088561275496,-0.815000100249152,
7.23763873740305));
#13425=CARTESIAN_POINT('Ctrl Pts',(0.632828311656819,-0.928293333247116,
7.23178625266915));
#13426=CARTESIAN_POINT('Ctrl Pts',(0.663522594372679,-1.04021428478872,
7.22593376793525));
#13427=CARTESIAN_POINT('Ctrl Pts',(0.694219691342193,-1.15214549797904,
7.22008074660708));
#13428=CARTESIAN_POINT('Ctrl Pts',(0.729872114404692,-1.26270378114022,
7.21422772527889));
#13429=CARTESIAN_POINT('Ctrl Pts',(0.770322487864552,-1.37142703342161,
7.20837470395072));
#13430=CARTESIAN_POINT('Ctrl Pts',(0.810786352305245,-1.48018654700758,
7.20251973052688));
#13431=CARTESIAN_POINT('Ctrl Pts',(0.856051205102927,-1.58710942573772,
7.19666475710303));
#13432=CARTESIAN_POINT('Ctrl Pts',(0.905911452222711,-1.69175333475471,
7.19080978367919));
#13433=CARTESIAN_POINT('Ctrl Pts',(0.955828209528095,-1.79651584420114,
7.18494817439504));
#13434=CARTESIAN_POINT('Ctrl Pts',(1.01035057877626,-1.89899385540313,7.1790865651109));
#13435=CARTESIAN_POINT('Ctrl Pts',(1.06922685930345,-1.99876936156115,7.17322495582675));
#13436=CARTESIAN_POINT('Ctrl Pts',(1.12814284053891,-2.09861214707559,7.16735939401642));
#13437=CARTESIAN_POINT('Ctrl Pts',(1.19141835408643,-2.19574845358574,7.16149383220609));
#13438=CARTESIAN_POINT('Ctrl Pts',(1.25875919173999,-2.28979044954935,7.15562827039576));
#13439=CARTESIAN_POINT('Ctrl Pts',(1.32619849821487,-2.38396995797673,7.14975413169542));
#13440=CARTESIAN_POINT('Ctrl Pts',(1.39771473835196,-2.47504580212225,7.14387999299507));
#13441=CARTESIAN_POINT('Ctrl Pts',(1.47297436304945,-2.56266426156141,7.13800585429473));
#13442=CARTESIAN_POINT('Ctrl Pts',(1.49200629351248,-2.58482153957106,7.13652038051348));
#13443=CARTESIAN_POINT('Ctrl Pts',(1.51127743693832,-2.60675790802619,7.13503490673223));
#13444=CARTESIAN_POINT('Ctrl Pts',(1.53078204993991,-2.62846804217311,7.13354943295097));
#13445=CARTESIAN_POINT('Ctrl Pts',(1.60790494493833,-2.71431175494393,7.12767574356041));
#13446=CARTESIAN_POINT('Ctrl Pts',(1.68893764981593,-2.79690122454661,7.12180205416984));
#13447=CARTESIAN_POINT('Ctrl Pts',(1.77357475394073,-2.87585933148987,7.11592836477927));
#13448=CARTESIAN_POINT('Ctrl Pts',(1.85810258361284,-2.95471549609932,7.11006225887352));
#13449=CARTESIAN_POINT('Ctrl Pts',(1.94622525867404,-3.02994934254741,7.10419615296776));
#13450=CARTESIAN_POINT('Ctrl Pts',(2.03759809489637,-3.10121783023809,7.098330047062));
#13451=CARTESIAN_POINT('Ctrl Pts',(2.12887736649824,-3.17241333990514,7.09246994797397));
#13452=CARTESIAN_POINT('Ctrl Pts',(2.22339985551396,-3.23965131485787,7.08660984888595));
#13453=CARTESIAN_POINT('Ctrl Pts',(2.32078561020942,-3.30262698542774,7.08074974979792));
#13454=CARTESIAN_POINT('Ctrl Pts',(2.42168482076202,-3.36787467452139,7.07467823170381));
#13455=CARTESIAN_POINT('Ctrl Pts',(2.52565746761902,-3.42854639602888,7.0686067136097));
#13456=CARTESIAN_POINT('Ctrl Pts',(2.63224507873663,-3.48435011121998,7.0625351955156));
#13457=CARTESIAN_POINT('Ctrl Pts',(2.73500291180405,-3.53814875432703,7.05668183191885));
#13458=CARTESIAN_POINT('Ctrl Pts',(2.84019063022018,-3.58742298538917,7.0508284683221));
#13459=CARTESIAN_POINT('Ctrl Pts',(2.94737050197106,-3.63195682830333,7.04497510472535));
#13460=CARTESIAN_POINT('Ctrl Pts',(3.05453428102504,-3.6764839846109,7.03912261999144));
#13461=CARTESIAN_POINT('Ctrl Pts',(3.16368923724138,-3.71627200952159,7.03327013525753));
#13462=CARTESIAN_POINT('Ctrl Pts',(3.27437695368253,-3.75115277520304,7.02741765052361));
#13463=CARTESIAN_POINT('Ctrl Pts',(3.3850748187013,-3.78603673898243,7.02156462919542));
#13464=CARTESIAN_POINT('Ctrl Pts',(3.49730532924808,-3.81601242493366,7.01571160786723));
#13465=CARTESIAN_POINT('Ctrl Pts',(3.61059486349046,-3.84096156782253,7.00985858653904));
#13466=CARTESIAN_POINT('Ctrl Pts',(3.72392218197992,-3.86591903173227,7.00400361311522));
#13467=CARTESIAN_POINT('Ctrl Pts',(3.83830882323813,-3.88584653022775,6.99814863969141));
#13468=CARTESIAN_POINT('Ctrl Pts',(3.95327163533168,-3.9006770316566,6.99229366626759));
#13469=CARTESIAN_POINT('Ctrl Pts',(4.06836474300635,-3.91552434155392,6.98643205698344));
#13470=CARTESIAN_POINT('Ctrl Pts',(4.18403491491749,-3.92526307136835,6.98057044769929));
#13471=CARTESIAN_POINT('Ctrl Pts',(4.29979444734751,-3.92987812168109,6.97470883841514));
#13472=CARTESIAN_POINT('Ctrl Pts',(4.4156320372802,-3.93449628395615,6.96884327660481));
#13473=CARTESIAN_POINT('Ctrl Pts',(4.53155869559722,-3.93398388900966,6.96297771479449));
#13474=CARTESIAN_POINT('Ctrl Pts',(4.64708903134349,-3.92837791513816,6.95711215298416));
#13475=CARTESIAN_POINT('Ctrl Pts',(4.7627883007767,-3.92276374395788,6.95123801428382));
#13476=CARTESIAN_POINT('Ctrl Pts',(4.8780896812728,-3.91204116750255,6.94536387558348));
#13477=CARTESIAN_POINT('Ctrl Pts',(4.9925151186429,-3.89629871449349,6.93948973688314));
#13478=CARTESIAN_POINT('Ctrl Pts',(5.02145144374442,-3.89231770512498,6.93800426310187));
#13479=CARTESIAN_POINT('Ctrl Pts',(5.05033181643606,-3.88801592605609,6.93651878932059));
#13480=CARTESIAN_POINT('Ctrl Pts',(5.07914864874074,-3.8833953169004,6.93503331553931));
#13481=CARTESIAN_POINT('Ctrl Pts',(5.1930928491103,-3.86512503618743,6.92915962614875));
#13482=CARTESIAN_POINT('Ctrl Pts',(5.30642202853069,-3.84180515537933,6.92328593675819));
#13483=CARTESIAN_POINT('Ctrl Pts',(5.41865372452572,-3.81348787336377,6.91741224736763));
#13484=CARTESIAN_POINT('Ctrl Pts',(5.53074051885709,-3.78520715161968,6.9115461414619));
#13485=CARTESIAN_POINT('Ctrl Pts',(5.64173225068844,-3.75194195995854,6.90568003555618));
#13486=CARTESIAN_POINT('Ctrl Pts',(5.75115380371673,-3.71379597367212,6.89981392965046));
#13487=CARTESIAN_POINT('Ctrl Pts',(5.8604633104693,-3.67568904838949,6.89395383056241));
#13488=CARTESIAN_POINT('Ctrl Pts',(5.96820544875217,-3.632711404855,6.88809373147437));
#13489=CARTESIAN_POINT('Ctrl Pts',(6.07391814277246,-3.5850171009564,6.88223363238633));
#13490=CARTESIAN_POINT('Ctrl Pts',(6.18344470962372,-3.53560209538128,6.87616211429222));
#13491=CARTESIAN_POINT('Ctrl Pts',(6.29079219405587,-3.48112378161116,6.87009059619811));
#13492=CARTESIAN_POINT('Ctrl Pts',(6.39546665157674,-3.42180910032891,6.864019078104));
#13493=CARTESIAN_POINT('Ctrl Pts',(6.496380072185,-3.36462564294833,6.85816571450725));
#13494=CARTESIAN_POINT('Ctrl Pts',(6.59480885780615,-3.30294760704014,6.8523123509105));
#13495=CARTESIAN_POINT('Ctrl Pts',(6.6903342233379,-3.23702573955104,6.84645898731376));
#13496=CARTESIAN_POINT('Ctrl Pts',(6.78584524605742,-3.17111377000855,6.84060650257986));
#13497=CARTESIAN_POINT('Ctrl Pts',(6.87845337555303,-3.10095947046721,6.83475401784597));
#13498=CARTESIAN_POINT('Ctrl Pts',(6.96776882050604,-3.02685690857993,6.82890153311207));
#13499=CARTESIAN_POINT('Ctrl Pts',(7.05709245448592,-2.95274755248287,6.82304851178392));
#13500=CARTESIAN_POINT('Ctrl Pts',(7.14312248580832,-2.87468947822836,6.81719549045577));
#13501=CARTESIAN_POINT('Ctrl Pts',(7.22550278036893,-2.7930165612505,6.81134246912762));
#13502=CARTESIAN_POINT('Ctrl Pts',(7.30791055034922,-2.71131640477706,6.80548749570378));
#13503=CARTESIAN_POINT('Ctrl Pts',(7.38666586986888,-2.62599929897716,6.79963252227995));
#13504=CARTESIAN_POINT('Ctrl Pts',(7.46145049044606,-2.53743490171557,6.79377754885611));
#13505=CARTESIAN_POINT('Ctrl Pts',(7.53631986978456,-2.4487701280858,6.78791593957197));
#13506=CARTESIAN_POINT('Ctrl Pts',(7.60720930120241,-2.35685103299911,6.78205433028784));
#13507=CARTESIAN_POINT('Ctrl Pts',(7.67384170771563,-2.26207925217795,6.7761927210037));
#13508=CARTESIAN_POINT('Ctrl Pts',(7.74051904495014,-2.16724356604867,6.77032715919335));
#13509=CARTESIAN_POINT('Ctrl Pts',(7.80293341950909,-2.06955171119052,6.76446159738301));
#13510=CARTESIAN_POINT('Ctrl Pts',(7.86085276949195,-1.96943161171825,6.75859603557266));
#13511=CARTESIAN_POINT('Ctrl Pts',(7.91885681177011,-1.86916511210453,6.75272189687233));
#13512=CARTESIAN_POINT('Ctrl Pts',(7.9723525216318,-1.76646364660131,6.746847758172));
#13513=CARTESIAN_POINT('Ctrl Pts',(8.0211551327337,-1.6617769201567,6.74097361947167));
#13514=CARTESIAN_POINT('Ctrl Pts',(8.03349651637322,-1.63530335606152,6.73948814569033));
#13515=CARTESIAN_POINT('Ctrl Pts',(8.04553802238277,-1.60870291690999,6.73800267190899));
#13516=CARTESIAN_POINT('Ctrl Pts',(8.05727716712034,-1.58198303042179,6.73651719812766));
#13517=CARTESIAN_POINT('Ctrl Pts',(8.1084003026791,-1.46561983620379,6.73004806607504));
#13518=CARTESIAN_POINT('Ctrl Pts',(8.153931540328,-1.34665702084391,6.72357893402242));
#13519=CARTESIAN_POINT('Ctrl Pts',(8.19362510200889,-1.22562394849566,6.7171098019698));
#13520=CARTESIAN_POINT('Ctrl Pts',(8.23315965443665,-1.10507572501514,6.71066658474599));
#13521=CARTESIAN_POINT('Ctrl Pts',(8.26690307392798,-0.98247403906862,6.70422336752219));
#13522=CARTESIAN_POINT('Ctrl Pts',(8.29465845219617,-0.858365623974744,
6.69778015029838));
#13523=CARTESIAN_POINT('Ctrl Pts',(8.32234009544139,-0.734586915676805,
6.6913540501452));
#13524=CARTESIAN_POINT('Ctrl Pts',(8.34406534138423,-0.609309719422338,
6.68492794999202));
#13525=CARTESIAN_POINT('Ctrl Pts',(8.3596866062786,-0.483096416073087,6.67850184983884));
#13526=CARTESIAN_POINT('Ctrl Pts',(8.37524543826056,-0.357387544609839,
6.67210143263455));
#13527=CARTESIAN_POINT('Ctrl Pts',(8.38474888011412,-0.230750293069467,
6.66570101543027));
#13528=CARTESIAN_POINT('Ctrl Pts',(8.3881002700853,-0.103756403703388,6.65930059822598));
#13529=CARTESIAN_POINT('Ctrl Pts',(8.38899688933635,-0.0697808989274935,
6.6575882528023));
#13530=CARTESIAN_POINT('Ctrl Pts',(8.38945344844305,-0.0357799447000208,
6.65587590737861));
#13531=CARTESIAN_POINT('Ctrl Pts',(8.38946871033935,-0.00176464821109916,
6.65416356195493));
#13532=CARTESIAN_POINT('',(8.38972787904154,0.00332410110871984,9.15416352203496));
#13533=CARTESIAN_POINT('Ctrl Pts',(8.39162089400544,0.00332570094577824,
9.15416352203496));
#13534=CARTESIAN_POINT('Ctrl Pts',(8.39372334105807,0.236557087994407,9.14234588371248));
#13535=CARTESIAN_POINT('Ctrl Pts',(8.26865424024228,1.77349980320093,9.06435620625279));
#13536=CARTESIAN_POINT('Ctrl Pts',(6.24434514927126,4.29152407052596,8.92019448965587));
#13537=CARTESIAN_POINT('Ctrl Pts',(1.81949236073018,3.82884228416074,8.72167837224421));
#13538=CARTESIAN_POINT('Ctrl Pts',(-0.190467284909431,-0.140220433735275,
8.52316225483256));
#13539=CARTESIAN_POINT('Ctrl Pts',(2.05514902234277,-3.9808719456923,8.3246461374209));
#13540=CARTESIAN_POINT('Ctrl Pts',(6.49984858445665,-4.17591665399795,8.12613002000926));
#13541=CARTESIAN_POINT('Ctrl Pts',(8.31678720259861,-1.61356007833625,7.98596914821393));
#13542=CARTESIAN_POINT('Ctrl Pts',(8.39494635335579,-0.156602103613678,
7.91198031555583));
#13543=CARTESIAN_POINT('Ctrl Pts',(8.3937869499332,-0.00255157889176684,
7.90416352203496));
#13544=CARTESIAN_POINT('',(8.38946907025241,0.000531890299595265,10.4041635220091));
#13545=CARTESIAN_POINT('Ctrl Pts',(8.38946907025241,0.000531890299602342,
10.4041635220091));
#13546=CARTESIAN_POINT('Ctrl Pts',(8.38945241340615,0.123698971527209,10.3979671066763));
#13547=CARTESIAN_POINT('Ctrl Pts',(8.38364577828166,0.246730412162652,10.3917706913436));
#13548=CARTESIAN_POINT('Ctrl Pts',(8.37211282064582,0.369084409944182,10.3855742760109));
#13549=CARTESIAN_POINT('Ctrl Pts',(8.36036117144559,0.493758522654603,10.3792603623048));
#13550=CARTESIAN_POINT('Ctrl Pts',(8.34266391787132,0.617728875751,10.3729464485986));
#13551=CARTESIAN_POINT('Ctrl Pts',(8.3191423869568,0.74043509254254,10.3666325348925));
#13552=CARTESIAN_POINT('Ctrl Pts',(8.29595163295195,0.861415725088067,10.3604074120424));
#13553=CARTESIAN_POINT('Ctrl Pts',(8.26709952108454,0.981167248167593,10.3541822891922));
#13554=CARTESIAN_POINT('Ctrl Pts',(8.23275230602851,1.09916977525348,10.3479571663421));
#13555=CARTESIAN_POINT('Ctrl Pts',(8.19767023351702,1.21969696224706,10.341598857208));
#13556=CARTESIAN_POINT('Ctrl Pts',(8.15685541023361,1.3383991161203,10.3352405480739));
#13557=CARTESIAN_POINT('Ctrl Pts',(8.11053592485518,1.45474557395325,10.3288822389398));
#13558=CARTESIAN_POINT('Ctrl Pts',(8.06421643947676,1.57109203178621,10.3225239298057));
#13559=CARTESIAN_POINT('Ctrl Pts',(8.01239250780688,1.68508249127428,10.3161656206716));
#13560=CARTESIAN_POINT('Ctrl Pts',(7.95534068950908,1.79621453163031,10.3098073115375));
#13561=CARTESIAN_POINT('Ctrl Pts',(7.90263726588178,1.89887627276674,10.3039336221469));
#13562=CARTESIAN_POINT('Ctrl Pts',(7.84532387922023,1.99938744358075,10.2980599327564));
#13563=CARTESIAN_POINT('Ctrl Pts',(7.78359976553002,2.09730555138436,10.2921862433658));
#13564=CARTESIAN_POINT('Ctrl Pts',(7.72195534346928,2.19509723771183,10.28632013746));
#13565=CARTESIAN_POINT('Ctrl Pts',(7.65591173749817,2.29030217257148,10.2804540315543));
#13566=CARTESIAN_POINT('Ctrl Pts',(7.58571484446163,2.38250081000734,10.2745879256485));
#13567=CARTESIAN_POINT('Ctrl Pts',(7.51558983214928,2.47460503721305,10.2687278265605));
#13568=CARTESIAN_POINT('Ctrl Pts',(7.4413202409521,2.56370876344788,10.2628677274725));
#13569=CARTESIAN_POINT('Ctrl Pts',(7.3631958228677,2.64942046393477,10.2570076283844));
#13570=CARTESIAN_POINT('Ctrl Pts',(7.28225285400916,2.73822444703552,10.2509361102903));
#13571=CARTESIAN_POINT('Ctrl Pts',(7.19717190086365,2.8233866481401,10.2448645921962));
#13572=CARTESIAN_POINT('Ctrl Pts',(7.10832188785066,2.90450784549612,10.2387930741021));
#13573=CARTESIAN_POINT('Ctrl Pts',(7.02266432681241,2.98271429340066,10.2329397105053));
#13574=CARTESIAN_POINT('Ctrl Pts',(6.93350422654221,3.05716483048509,10.2270863469086));
#13575=CARTESIAN_POINT('Ctrl Pts',(6.84120983747266,3.12753907164982,10.2212329833118));
#13576=CARTESIAN_POINT('Ctrl Pts',(6.74892930609505,3.19790274635905,10.2153804985779));
#13577=CARTESIAN_POINT('Ctrl Pts',(6.65351575009993,3.26419109167856,10.209528013844));
#13578=CARTESIAN_POINT('Ctrl Pts',(6.55536961423406,3.32612472066983,10.2036755291101));
#13579=CARTESIAN_POINT('Ctrl Pts',(6.45721447968537,3.38806402814328,10.197822507782));
#13580=CARTESIAN_POINT('Ctrl Pts',(6.35632661662856,3.44564760508633,10.1919694864538));
#13581=CARTESIAN_POINT('Ctrl Pts',(6.25313387825276,3.49864040691955,10.1861164651256));
#13582=CARTESIAN_POINT('Ctrl Pts',(6.14990672310565,3.55165088287568,10.1802614917018));
#13583=CARTESIAN_POINT('Ctrl Pts',(6.04437353139222,3.60006735054361,10.174406518278));
#13584=CARTESIAN_POINT('Ctrl Pts',(5.93698442660608,3.64370187942111,10.1685515448541));
#13585=CARTESIAN_POINT('Ctrl Pts',(5.82947361006336,3.68738586243242,10.16268993557));
#13586=CARTESIAN_POINT('Ctrl Pts',(5.72010306507971,3.72627693362288,10.1568283262858));
#13587=CARTESIAN_POINT('Ctrl Pts',(5.60934054948644,3.76023622067773,10.1509667170017));
#13588=CARTESIAN_POINT('Ctrl Pts',(5.49850334591545,3.79421840672924,10.1451011551913));
#13589=CARTESIAN_POINT('Ctrl Pts',(5.38627270172141,3.82326208351065,10.139235593381));
#13590=CARTESIAN_POINT('Ctrl Pts',(5.27312740818583,3.84727932672265,10.1333700315706));
#13591=CARTESIAN_POINT('Ctrl Pts',(5.15981666848041,3.87133168903483,10.1274958928703));
#13592=CARTESIAN_POINT('Ctrl Pts',(5.04558901620855,3.89034288170041,10.12162175417));
#13593=CARTESIAN_POINT('Ctrl Pts',(4.93092928357524,3.90427669871161,10.1157476154696));
#13594=CARTESIAN_POINT('Ctrl Pts',(4.90193370902624,3.90780033356249,10.1142621416884));
#13595=CARTESIAN_POINT('Ctrl Pts',(4.87291050496303,3.91099952969373,10.1127766679071));
#13596=CARTESIAN_POINT('Ctrl Pts',(4.8438675031252,3.91387422920997,10.1112911941258));
#13597=CARTESIAN_POINT('Ctrl Pts',(4.7290290092294,3.92524103504814,10.1054175047352));
#13598=CARTESIAN_POINT('Ctrl Pts',(4.61349855164524,3.93156820814743,10.0995438153446));
#13599=CARTESIAN_POINT('Ctrl Pts',(4.49775596818432,3.93278328859206,10.0936701259541));
#13600=CARTESIAN_POINT('Ctrl Pts',(4.38216281927222,3.93399680025369,10.0878040200483));
#13601=CARTESIAN_POINT('Ctrl Pts',(4.2663584984788,3.93011134058082,10.0819379141426));
#13602=CARTESIAN_POINT('Ctrl Pts',(4.15082885658152,3.92110609876882,10.0760718082368));
#13603=CARTESIAN_POINT('Ctrl Pts',(4.0354175155657,3.9121100782097,10.0702117091488));
#13604=CARTESIAN_POINT('Ctrl Pts',(3.92028070342867,3.89800473537621,10.0643516100607));
#13605=CARTESIAN_POINT('Ctrl Pts',(3.8059044988267,3.87882130184022,10.0584915109727));
#13606=CARTESIAN_POINT('Ctrl Pts',(3.6874018616966,3.85894577378668,10.0524199928786));
#13607=CARTESIAN_POINT('Ctrl Pts',(3.56971620191733,3.83361882040805,10.0463484747845));
#13608=CARTESIAN_POINT('Ctrl Pts',(3.45338298609684,3.80293402988006,10.0402769566904));
#13609=CARTESIAN_POINT('Ctrl Pts',(3.34122971569198,3.77335176839842,10.0344235930936));
#13610=CARTESIAN_POINT('Ctrl Pts',(3.23033380679234,3.73879018073694,10.0285702294969));
#13611=CARTESIAN_POINT('Ctrl Pts',(3.12116411357318,3.69938502681421,10.0227168659001));
#13612=CARTESIAN_POINT('Ctrl Pts',(3.01201081181605,3.65998578944272,10.0168643811662));
#13613=CARTESIAN_POINT('Ctrl Pts',(2.90458359888168,3.61574457207698,10.0110118964323));
#13614=CARTESIAN_POINT('Ctrl Pts',(2.79933433071275,3.56684641326345,10.0051594116984));
#13615=CARTESIAN_POINT('Ctrl Pts',(2.69407541259906,3.51794377114529,9.99930639037026));
#13616=CARTESIAN_POINT('Ctrl Pts',(2.59099521091513,3.46438351286954,9.99345336904209));
#13617=CARTESIAN_POINT('Ctrl Pts',(2.49052317874863,3.40639774692646,9.98760034771391));
#13618=CARTESIAN_POINT('Ctrl Pts',(2.39001763721911,3.34839264161062,9.98174537429009));
#13619=CARTESIAN_POINT('Ctrl Pts',(2.29212235254894,3.28595930008548,9.97589040086627));
#13620=CARTESIAN_POINT('Ctrl Pts',(2.1972392604409,3.21937408574227,9.97003542744246));
#13621=CARTESIAN_POINT('Ctrl Pts',(2.10224863053523,3.15271340561115,9.9641738181583));
#13622=CARTESIAN_POINT('Ctrl Pts',(2.01027734556785,3.08189169799394,9.95831220887415));
#13623=CARTESIAN_POINT('Ctrl Pts',(1.92169567700385,3.00722673946423,9.95245059959));
#13624=CARTESIAN_POINT('Ctrl Pts',(1.83305427717017,2.93251143380463,9.94658503777966));
#13625=CARTESIAN_POINT('Ctrl Pts',(1.74780734801486,2.85394799620934,9.94071947596932));
#13626=CARTESIAN_POINT('Ctrl Pts',(1.6662883303241,2.77189109415048,9.93485391415898));
#13627=CARTESIAN_POINT('Ctrl Pts',(1.58465011183569,2.6897142047751,9.92897977545866));
#13628=CARTESIAN_POINT('Ctrl Pts',(1.50675096073738,2.6040339605629,9.92310563675833));
#13629=CARTESIAN_POINT('Ctrl Pts',(1.43288413337119,2.51523814219915,9.917231498058));
#13630=CARTESIAN_POINT('Ctrl Pts',(1.41420441861529,2.49278312933758,9.91574602427672));
#13631=CARTESIAN_POINT('Ctrl Pts',(1.39578235403901,2.47012901786274,9.91426055049544));
#13632=CARTESIAN_POINT('Ctrl Pts',(1.37762223395277,2.44728235746125,9.91277507671416));
#13633=CARTESIAN_POINT('Ctrl Pts',(1.30581557803848,2.35694472343405,9.9069013873236));
#13634=CARTESIAN_POINT('Ctrl Pts',(1.23786864496497,2.26329359404981,9.90102769793303));
#13635=CARTESIAN_POINT('Ctrl Pts',(1.17410244800949,2.16669289957748,9.89515400854246));
#13636=CARTESIAN_POINT('Ctrl Pts',(1.11041857920489,2.07021692567701,9.88928790263671));
#13637=CARTESIAN_POINT('Ctrl Pts',(1.05090493774002,1.97079930153077,9.88342179673096));
#13638=CARTESIAN_POINT('Ctrl Pts',(0.995842395424703,1.8688370096245,9.87755569082521));
#13639=CARTESIAN_POINT('Ctrl Pts',(0.940836236451232,1.76697912580616,9.87169559173717));
#13640=CARTESIAN_POINT('Ctrl Pts',(0.890272305795063,1.6625821185592,9.86583549264913));
#13641=CARTESIAN_POINT('Ctrl Pts',(0.84438786718391,1.55607137452501,9.85997539356109));
#13642=CARTESIAN_POINT('Ctrl Pts',(0.796848022706831,1.44571796583597,9.85390387546698));
#13643=CARTESIAN_POINT('Ctrl Pts',(0.754331944901039,1.33309580010854,9.84783235737288));
#13644=CARTESIAN_POINT('Ctrl Pts',(0.717051272429055,1.21870556917548,9.84176083927877));
#13645=CARTESIAN_POINT('Ctrl Pts',(0.681110124312961,1.10842547065824,9.83590747568202));
#13646=CARTESIAN_POINT('Ctrl Pts',(0.650034770690332,0.996502602800106,
9.83005411208527));
#13647=CARTESIAN_POINT('Ctrl Pts',(0.623965301743936,0.883404544186814,
9.82420074848851));
#13648=CARTESIAN_POINT('Ctrl Pts',(0.597899747040573,0.770323466866426,
9.81834826375461));
#13649=CARTESIAN_POINT('Ctrl Pts',(0.576838675290042,0.656067952121766,
9.81249577902071));
#13650=CARTESIAN_POINT('Ctrl Pts',(0.560871552553867,0.541118009203235,
9.8066432942868));
#13651=CARTESIAN_POINT('Ctrl Pts',(0.544902965846919,0.426157526918307,
9.80079027295863));
#13652=CARTESIAN_POINT('Ctrl Pts',(0.534029313444819,0.310502899128489,
9.79493725163045));
#13653=CARTESIAN_POINT('Ctrl Pts',(0.528288363365169,0.194640826853502,
9.78908423030227));
#13654=CARTESIAN_POINT('Ctrl Pts',(0.522545498567798,0.0787401123398783,
9.78322925687845));
#13655=CARTESIAN_POINT('Ctrl Pts',(0.521938760476017,-0.0373677718176726,
9.77737428345463));
#13656=CARTESIAN_POINT('Ctrl Pts',(0.526453811930776,-0.153195256671141,
9.7715193100308));
#13657=CARTESIAN_POINT('Ctrl Pts',(0.530973980616423,-0.26915401710119,
9.76565770074665));
#13658=CARTESIAN_POINT('Ctrl Pts',(0.540627508959133,-0.384831330861955,
9.75979609146249));
#13659=CARTESIAN_POINT('Ctrl Pts',(0.555348094493326,-0.499743786232803,
9.75393448217834));
#13660=CARTESIAN_POINT('Ctrl Pts',(0.570078606226456,-0.614733727916248,
9.74806892036799));
#13661=CARTESIAN_POINT('Ctrl Pts',(0.589882908261818,-0.728957378173498,
9.74220335855765));
#13662=CARTESIAN_POINT('Ctrl Pts',(0.614643732160975,-0.84194227548548,
9.73633779674731));
#13663=CARTESIAN_POINT('Ctrl Pts',(0.639440762457654,-0.95509238442866,
9.73046365804698));
#13664=CARTESIAN_POINT('Ctrl Pts',(0.66920867330973,-1.0669997276802,9.72458951934664));
#13665=CARTESIAN_POINT('Ctrl Pts',(0.703780586616563,-1.17720766003696,
9.71871538064631));
#13666=CARTESIAN_POINT('Ctrl Pts',(0.712523259101106,-1.20507744697188,
9.71722990686504));
#13667=CARTESIAN_POINT('Ctrl Pts',(0.721572910325626,-1.23283866169091,
9.71574443308376));
#13668=CARTESIAN_POINT('Ctrl Pts',(0.730926364523589,-1.2604841450039,9.71425895930249));
#13669=CARTESIAN_POINT('Ctrl Pts',(0.767910716169708,-1.36979673205834,
9.70838526991192));
#13670=CARTESIAN_POINT('Ctrl Pts',(0.809771816427867,-1.47766224106937,
9.70251158052135));
#13671=CARTESIAN_POINT('Ctrl Pts',(0.856377876187989,-1.58361363200093,
9.69663789113078));
#13672=CARTESIAN_POINT('Ctrl Pts',(0.902923763146497,-1.68942822973307,
9.69077178522503));
#13673=CARTESIAN_POINT('Ctrl Pts',(0.954202261794194,-1.79333324928329,
9.68490567931928));
#13674=CARTESIAN_POINT('Ctrl Pts',(1.01003204791259,-1.89487746388452,9.67903957341353));
#13675=CARTESIAN_POINT('Ctrl Pts',(1.06580466504125,-1.99631769850363,9.67317947432549));
#13676=CARTESIAN_POINT('Ctrl Pts',(1.12611910173288,-2.09540157676892,9.66731937523745));
#13677=CARTESIAN_POINT('Ctrl Pts',(1.19074652517804,-2.19169911796397,9.66145927614942));
#13678=CARTESIAN_POINT('Ctrl Pts',(1.25770555862236,-2.2914708547555,9.65538775805531));
#13679=CARTESIAN_POINT('Ctrl Pts',(1.32929447810303,-2.3882509957593,9.6493162399612));
#13680=CARTESIAN_POINT('Ctrl Pts',(1.4052072796758,-2.48159026954186,9.6432447218671));
#13681=CARTESIAN_POINT('Ctrl Pts',(1.47839247362007,-2.57157578862252,9.63739135827035));
#13682=CARTESIAN_POINT('Ctrl Pts',(1.55559589300616,-2.65836310329154,9.6315379946736));
#13683=CARTESIAN_POINT('Ctrl Pts',(1.63650057209977,-2.74158101587053,9.62568463107685));
#13684=CARTESIAN_POINT('Ctrl Pts',(1.71739310362806,-2.82478643355997,9.61983214634295));
#13685=CARTESIAN_POINT('Ctrl Pts',(1.80198550194642,-2.90442321865073,9.61397966160904));
#13686=CARTESIAN_POINT('Ctrl Pts',(1.88992291191788,-2.98015597452923,9.60812717687514));
#13687=CARTESIAN_POINT('Ctrl Pts',(1.97786838456911,-3.05589567408459,9.60227415554697));
#13688=CARTESIAN_POINT('Ctrl Pts',(2.06915916547981,-3.12773036324282,9.5964211342188));
#13689=CARTESIAN_POINT('Ctrl Pts',(2.16340675036543,-3.19536445999055,9.59056811289063));
#13690=CARTESIAN_POINT('Ctrl Pts',(2.25768576864082,-3.26302111401577,9.58471313946681));
#13691=CARTESIAN_POINT('Ctrl Pts',(2.35492321633055,-3.3264741491004,9.57885816604298));
#13692=CARTESIAN_POINT('Ctrl Pts',(2.45470161311127,-3.38547129710772,9.57300319261916));
#13693=CARTESIAN_POINT('Ctrl Pts',(2.55459309588865,-3.44453531080437,9.56714158333501));
#13694=CARTESIAN_POINT('Ctrl Pts',(2.65703091991477,-3.49913314718241,9.56127997405085));
#13695=CARTESIAN_POINT('Ctrl Pts',(2.76157292733018,-3.54905845863246,9.5554183647667));
#13696=CARTESIAN_POINT('Ctrl Pts',(2.86618542818888,-3.59901743508664,9.54955280295636));
#13697=CARTESIAN_POINT('Ctrl Pts',(2.97290455832861,-3.64429745186445,9.54368724114602));
#13698=CARTESIAN_POINT('Ctrl Pts',(3.08126973229157,-3.68474092467186,9.53782167933568));
#13699=CARTESIAN_POINT('Ctrl Pts',(3.18979336271725,-3.72524353575596,9.53194754063535));
#13700=CARTESIAN_POINT('Ctrl Pts',(3.29996744900717,-3.76089536180044,9.52607340193502));
#13701=CARTESIAN_POINT('Ctrl Pts',(3.41131780240822,-3.79158908007503,9.52019926323468));
#13702=CARTESIAN_POINT('Ctrl Pts',(3.43947648897517,-3.79935102034795,9.5187137894534));
#13703=CARTESIAN_POINT('Ctrl Pts',(3.46771035755175,-3.80679614594589,9.51722831567212));
#13704=CARTESIAN_POINT('Ctrl Pts',(3.49601167060103,-3.8139232444253,9.51574284189084));
#13705=CARTESIAN_POINT('Ctrl Pts',(3.60791746408699,-3.84210439662843,9.50986915250028));
#13706=CARTESIAN_POINT('Ctrl Pts',(3.72125099834294,-3.86540310393352,9.50399546310971));
#13707=CARTESIAN_POINT('Ctrl Pts',(3.8355483718316,-3.88367692291837,9.49812177371915));
#13708=CARTESIAN_POINT('Ctrl Pts',(3.94969817667328,-3.90192714868616,9.49225566781339));
#13709=CARTESIAN_POINT('Ctrl Pts',(4.06480894179248,-3.91516532321931,9.48638956190764));
#13710=CARTESIAN_POINT('Ctrl Pts',(4.18040320021251,-3.92329920035946,9.48052345600189));
#13711=CARTESIAN_POINT('Ctrl Pts',(4.29587909158459,-3.93142474851305,9.47466335691385));
#13712=CARTESIAN_POINT('Ctrl Pts',(4.41183708180411,-3.93445636685655,9.46880325782581));
#13713=CARTESIAN_POINT('Ctrl Pts',(4.52779180225849,-3.93235324875952,9.46294315873777));
#13714=CARTESIAN_POINT('Ctrl Pts',(4.64792990449177,-3.93017425495952,9.45687164064366));
#13715=CARTESIAN_POINT('Ctrl Pts',(4.76806405056415,-3.92248295906189,9.45080012254955));
#13716=CARTESIAN_POINT('Ctrl Pts',(4.88765082651595,-3.90929294426513,9.44472860445545));
#13717=CARTESIAN_POINT('Ctrl Pts',(5.0029407540364,-3.89657685724121,9.4388752408587));
#13718=CARTESIAN_POINT('Ctrl Pts',(5.11772152352217,-3.87875044681698,9.43302187726195));
#13719=CARTESIAN_POINT('Ctrl Pts',(5.23150938451202,-3.85587883199438,9.4271685136652));
#13720=CARTESIAN_POINT('Ctrl Pts',(5.34528016063744,-3.83301065126777,9.4213160289313));
#13721=CARTESIAN_POINT('Ctrl Pts',(5.45805791976276,-3.80509885377081,9.41546354419739));
#13722=CARTESIAN_POINT('Ctrl Pts',(5.56936845513688,-3.77225980536554,9.40961105946349));
#13723=CARTESIAN_POINT('Ctrl Pts',(5.6806891961926,-3.73941774606044,9.40375803813532));
#13724=CARTESIAN_POINT('Ctrl Pts',(5.79054204979292,-3.70164765469671,9.39790501680714));
#13725=CARTESIAN_POINT('Ctrl Pts',(5.89846802418478,-3.6591157566526,9.39205199547897));
#13726=CARTESIAN_POINT('Ctrl Pts',(6.0064299939734,-3.61656967339911,9.38619702205515));
#13727=CARTESIAN_POINT('Ctrl Pts',(6.11246342250275,-3.56925877688499,9.38034204863132));
#13728=CARTESIAN_POINT('Ctrl Pts',(6.21613000682399,-3.51739712214577,9.3744870752075));
#13729=CARTESIAN_POINT('Ctrl Pts',(6.31991408390305,-3.46547668888231,9.36862546592334));
#13730=CARTESIAN_POINT('Ctrl Pts',(6.4213255929435,-3.40899538788358,9.36276385663919));
#13731=CARTESIAN_POINT('Ctrl Pts',(6.51995144044893,-3.348212904867,9.35690224735504));
#13732=CARTESIAN_POINT('Ctrl Pts',(6.6186437920876,-3.28738943577575,9.3510366855447));
#13733=CARTESIAN_POINT('Ctrl Pts',(6.71454640096287,-3.22225924102633,9.34517112373436));
#13734=CARTESIAN_POINT('Ctrl Pts',(6.80727715999856,-3.15312392624864,9.33930556192402));
#13735=CARTESIAN_POINT('Ctrl Pts',(6.90014351414779,-3.08388751868411,9.33343142322368));
#13736=CARTESIAN_POINT('Ctrl Pts',(6.98982844338462,-3.01063456339955,9.32755728452334));
#13737=CARTESIAN_POINT('Ctrl Pts',(7.07598470134355,-2.93370534425244,9.32168314582301));
#13738=CARTESIAN_POINT('Ctrl Pts',(7.09777221246983,-2.91425120060912,9.32019767204173));
#13739=CARTESIAN_POINT('Ctrl Pts',(7.11933425862108,-2.89456213268461,9.31871219826045));
#13740=CARTESIAN_POINT('Ctrl Pts',(7.14066562637913,-2.87464398511472,9.31722672447918));
#13741=CARTESIAN_POINT('Ctrl Pts',(7.22376073689112,-2.79705399218563,9.31144014719928));
#13742=CARTESIAN_POINT('Ctrl Pts',(7.30364702188168,-2.71571004166237,9.30565356991938));
#13743=CARTESIAN_POINT('Ctrl Pts',(7.37995847202851,-2.63091218553458,9.29986699263949));
#13744=CARTESIAN_POINT('Ctrl Pts',(7.4600205031988,-2.54194665562505,9.29379601469763));
#13745=CARTESIAN_POINT('Ctrl Pts',(7.53614695790885,-2.44917930042223,9.28772503675578));
#13746=CARTESIAN_POINT('Ctrl Pts',(7.60795436220654,-2.35300439465982,9.28165405881392));
#13747=CARTESIAN_POINT('Ctrl Pts',(7.67622775464223,-2.26156275089337,9.27588186493577));
#13748=CARTESIAN_POINT('Ctrl Pts',(7.74059676747692,-2.1670413478874,9.27010967105763));
#13749=CARTESIAN_POINT('Ctrl Pts',(7.80077050348256,-2.06981573195683,9.26433747717948));
#13750=CARTESIAN_POINT('Ctrl Pts',(7.860907062838,-1.97265018413826,9.25856884948896));
#13751=CARTESIAN_POINT('Ctrl Pts',(7.91685327154823,-1.87278410434854,9.25280022179843));
#13752=CARTESIAN_POINT('Ctrl Pts',(7.96836070555525,-1.770623165585,9.24703159410791));
#13753=CARTESIAN_POINT('Ctrl Pts',(8.01984963901964,-1.6684989211907,9.24126503840456));
#13754=CARTESIAN_POINT('Ctrl Pts',(8.06690277522152,-1.56408183666917,9.23549848270121));
#13755=CARTESIAN_POINT('Ctrl Pts',(8.10931738031529,-1.45780262258862,9.22973192699786));
#13756=CARTESIAN_POINT('Ctrl Pts',(8.15172771930584,-1.35153409817726,9.22396595130042));
#13757=CARTESIAN_POINT('Ctrl Pts',(8.18950029855435,-1.24340421331412,9.21819997560299));
#13758=CARTESIAN_POINT('Ctrl Pts',(8.22248066516845,-1.13386328005343,9.21243399990555));
#13759=CARTESIAN_POINT('Ctrl Pts',(8.25547959033317,-1.02426070645439,9.20666477960647));
#13760=CARTESIAN_POINT('Ctrl Pts',(8.28368079446724,-0.913245907583533,
9.20089555930738));
#13761=CARTESIAN_POINT('Ctrl Pts',(8.30697991638799,-0.801283658117368,
9.19512633900829));
#13762=CARTESIAN_POINT('Ctrl Pts',(8.33028668955545,-0.689284641137116,
9.18935522414305));
#13763=CARTESIAN_POINT('Ctrl Pts',(8.34868810447865,-0.576337974560135,
9.18358410927781));
#13764=CARTESIAN_POINT('Ctrl Pts',(8.36213133903415,-0.462916324140246,
9.17781299441257));
#13765=CARTESIAN_POINT('Ctrl Pts',(8.37558884384286,-0.349374274447022,
9.17203575339739));
#13766=CARTESIAN_POINT('Ctrl Pts',(8.38407763076053,-0.235356659269688,
9.16625851238221));
#13767=CARTESIAN_POINT('Ctrl Pts',(8.38759692383704,-0.121338705876156,
9.16048127136704));
#13768=CARTESIAN_POINT('Ctrl Pts',(8.38887977444717,-0.0797769496096529,
9.15837535492301));
#13769=CARTESIAN_POINT('Ctrl Pts',(8.38950280738372,-0.0382151267219463,
9.15626943847898));
#13770=CARTESIAN_POINT('Ctrl Pts',(8.38946770166849,0.00332388122593439,
9.15416352203496));
#13771=CARTESIAN_POINT('',(8.38946746815912,-0.0035895640966767,11.654163522035));
#13772=CARTESIAN_POINT('Ctrl Pts',(8.38946746815912,-0.0035895640966767,
11.654163522035));
#13773=CARTESIAN_POINT('Ctrl Pts',(8.38957177719058,0.110699312995978,11.6483796262953));
#13774=CARTESIAN_POINT('Ctrl Pts',(8.38469020710796,0.225131832695754,11.6425957305555));
#13775=CARTESIAN_POINT('Ctrl Pts',(8.37481197693192,0.339231701831254,11.6368118348158));
#13776=CARTESIAN_POINT('Ctrl Pts',(8.36494112420078,0.453246356765222,11.6310322587134));
#13777=CARTESIAN_POINT('Ctrl Pts',(8.35008106722861,0.566928433243951,11.625252682611));
#13778=CARTESIAN_POINT('Ctrl Pts',(8.33027309159042,0.679802679396528,11.6194731065086));
#13779=CARTESIAN_POINT('Ctrl Pts',(8.31047288488467,0.792632654877085,11.6136957972273));
#13780=CARTESIAN_POINT('Ctrl Pts',(8.28572868845862,0.904655011542767,11.607918487946));
#13781=CARTESIAN_POINT('Ctrl Pts',(8.2561334371495,1.01540138479756,11.6021411786646));
#13782=CARTESIAN_POINT('Ctrl Pts',(8.22654219053135,1.12613277237115,11.5963646511418));
#13783=CARTESIAN_POINT('Ctrl Pts',(8.19210130352364,1.23558810919518,11.5905881236189));
#13784=CARTESIAN_POINT('Ctrl Pts',(8.1529542431634,1.3433118150093,11.584811596096));
#13785=CARTESIAN_POINT('Ctrl Pts',(8.11380242285544,1.45104861910472,11.5790343661968));
#13786=CARTESIAN_POINT('Ctrl Pts',(8.06994343806426,1.55705297462456,11.5732571362976));
#13787=CARTESIAN_POINT('Ctrl Pts',(8.02156948115232,1.66088780977071,11.5674799063984));
#13788=CARTESIAN_POINT('Ctrl Pts',(7.97314712098685,1.76482654263728,11.5616968957705));
#13789=CARTESIAN_POINT('Ctrl Pts',(7.92020094699321,1.86659103422067,11.5559138851425));
#13790=CARTESIAN_POINT('Ctrl Pts',(7.862969864933,1.96576742797205,11.5501308745146));
#13791=CARTESIAN_POINT('Ctrl Pts',(7.80570950282026,2.06499456145984,11.5443449052346));
#13792=CARTESIAN_POINT('Ctrl Pts',(7.74416009704854,2.16163060308781,11.5385589359547));
#13793=CARTESIAN_POINT('Ctrl Pts',(7.67860370651661,2.25529102724241,11.5327729666747));
#13794=CARTESIAN_POINT('Ctrl Pts',(7.61294154446378,2.34910256718346,11.5269776620613));
#13795=CARTESIAN_POINT('Ctrl Pts',(7.54325974405533,2.43992856386017,11.5211823574478));
#13796=CARTESIAN_POINT('Ctrl Pts',(7.46988061977961,2.52741766432378,11.5153870528343));
#13797=CARTESIAN_POINT('Ctrl Pts',(7.40875340098826,2.60029895636267,11.510559373892));
#13798=CARTESIAN_POINT('Ctrl Pts',(7.34506123463426,2.67086518116762,11.5057316949497));
#13799=CARTESIAN_POINT('Ctrl Pts',(7.27900868446959,2.73893397678818,11.5009040160074));
#13800=CARTESIAN_POINT('Ctrl Pts',(7.19864456586121,2.82175119960764,11.4950303266169));
#13801=CARTESIAN_POINT('Ctrl Pts',(7.11449855412747,2.90116636477368,11.4891566372263));
#13802=CARTESIAN_POINT('Ctrl Pts',(7.02689032355886,2.97681436529812,11.4832829478357));
#13803=CARTESIAN_POINT('Ctrl Pts',(6.93939520344638,3.05236469714703,11.47741684193));
#13804=CARTESIAN_POINT('Ctrl Pts',(6.84844706380809,3.1241572692394,11.4715507360242));
#13805=CARTESIAN_POINT('Ctrl Pts',(6.7544035142015,3.19186253723538,11.4656846301185));
#13806=CARTESIAN_POINT('Ctrl Pts',(6.66045626399169,3.25949847589943,11.4598245310304));
#13807=CARTESIAN_POINT('Ctrl Pts',(6.56342024182953,3.32305519551627,11.4539644319424));
#13808=CARTESIAN_POINT('Ctrl Pts',(6.46368682834724,3.38224274941515,11.4481043328544));
#13809=CARTESIAN_POINT('Ctrl Pts',(6.36035526083478,3.4435656552303,11.4420328147602));
#13810=CARTESIAN_POINT('Ctrl Pts',(6.25412833768368,3.50019788883429,11.4359612966661));
#13811=CARTESIAN_POINT('Ctrl Pts',(6.14547541273053,3.55186524189217,11.429889778572));
#13812=CARTESIAN_POINT('Ctrl Pts',(6.04072647420424,3.60167614566315,11.4240364149753));
#13813=CARTESIAN_POINT('Ctrl Pts',(5.9337232750384,3.64687262031137,11.4181830513785));
#13814=CARTESIAN_POINT('Ctrl Pts',(5.82491152198139,3.68725566712431,11.4123296877818));
#13815=CARTESIAN_POINT('Ctrl Pts',(5.71611610664293,3.72763265055867,11.4064772030479));
#13816=CARTESIAN_POINT('Ctrl Pts',(5.60551306457982,3.76319749948607,11.400624718314));
#13817=CARTESIAN_POINT('Ctrl Pts',(5.49356693383226,3.79379982286339,11.3947722335801));
#13818=CARTESIAN_POINT('Ctrl Pts',(5.38161053912773,3.82440495206284,11.3889192122519));
#13819=CARTESIAN_POINT('Ctrl Pts',(5.26831120948605,3.8500465422721,11.3830661909238));
#13820=CARTESIAN_POINT('Ctrl Pts',(5.15414676086497,3.87062461241163,11.3772131695956));
#13821=CARTESIAN_POINT('Ctrl Pts',(5.03994423619526,3.891209545735,11.3713581961718));
#13822=CARTESIAN_POINT('Ctrl Pts',(4.92487642518261,3.90672752767297,11.3655032227479));
#13823=CARTESIAN_POINT('Ctrl Pts',(4.80942869842444,3.91713013905202,11.3596482493241));
#13824=CARTESIAN_POINT('Ctrl Pts',(4.69385012649667,3.92754454045489,11.35378664004));
#13825=CARTESIAN_POINT('Ctrl Pts',(4.5778911911083,3.93283196250982,11.3479250307558));
#13826=CARTESIAN_POINT('Ctrl Pts',(4.4620398160126,3.93299605481526,11.3420634214716));
#13827=CARTESIAN_POINT('Ctrl Pts',(4.34611032148418,3.93316025776935,11.3361978596613));
#13828=CARTESIAN_POINT('Ctrl Pts',(4.23028894341342,3.92819426955622,11.330332297851));
#13829=CARTESIAN_POINT('Ctrl Pts',(4.1150592936417,3.91815369018068,11.3244667360406));
#13830=CARTESIAN_POINT('Ctrl Pts',(3.99966114985995,3.90809842901547,11.3185925973403));
#13831=CARTESIAN_POINT('Ctrl Pts',(3.88485686922435,3.89295382146551,11.31271845864));
#13832=CARTESIAN_POINT('Ctrl Pts',(3.771120751629,3.87282669801552,11.3068443199397));
#13833=CARTESIAN_POINT('Ctrl Pts',(3.74235874424487,3.86773687707272,11.3053588461584));
#13834=CARTESIAN_POINT('Ctrl Pts',(3.71366497212237,3.86232867299291,11.3038733723771));
#13835=CARTESIAN_POINT('Ctrl Pts',(3.68504694311492,3.85660431549219,11.3023878985958));
#13836=CARTESIAN_POINT('Ctrl Pts',(3.57188882785466,3.83396972015761,11.2965142092052));
#13837=CARTESIAN_POINT('Ctrl Pts',(3.45953928810432,3.80631288254159,11.2906405198146));
#13838=CARTESIAN_POINT('Ctrl Pts',(3.34847842460446,3.77370449948814,11.2847668304241));
#13839=CARTESIAN_POINT('Ctrl Pts',(3.23756095111315,3.74113821692065,11.2789007245183));
#13840=CARTESIAN_POINT('Ctrl Pts',(3.12792923790653,3.70363321764498,11.2730346186126));
#13841=CARTESIAN_POINT('Ctrl Pts',(3.02005406722172,3.66131135465759,11.2671685127068));
#13842=CARTESIAN_POINT('Ctrl Pts',(2.91228935933741,3.61903282871874,11.2613084136188));
#13843=CARTESIAN_POINT('Ctrl Pts',(2.80627799857622,3.57194740002713,11.2554483145307));
#13844=CARTESIAN_POINT('Ctrl Pts',(2.70247580056403,3.52022676595133,11.2495882154427));
#13845=CARTESIAN_POINT('Ctrl Pts',(2.59492865605821,3.46664016939171,11.2435166973486));
#13846=CARTESIAN_POINT('Ctrl Pts',(2.48975352039065,3.40807772474979,11.2374451792545));
#13847=CARTESIAN_POINT('Ctrl Pts',(2.38743525415579,3.3447851827912,11.2313736611604));
#13848=CARTESIAN_POINT('Ctrl Pts',(2.28879336499758,3.2837667924474,11.2255202975636));
#13849=CARTESIAN_POINT('Ctrl Pts',(2.19280696070861,3.21835260328323,11.2196669339669));
#13850=CARTESIAN_POINT('Ctrl Pts',(2.09988488333601,3.14880926708216,11.2138135703701));
#13851=CARTESIAN_POINT('Ctrl Pts',(2.00697675790056,3.07927637257896,11.2079610856362));
#13852=CARTESIAN_POINT('Ctrl Pts',(1.91713237521333,3.00561581126974,11.2021086009023));
#13853=CARTESIAN_POINT('Ctrl Pts',(1.83072994053781,2.92813640970017,11.1962561161684));
#13854=CARTESIAN_POINT('Ctrl Pts',(1.74431958391904,2.85064990430968,11.1904030948403));
#13855=CARTESIAN_POINT('Ctrl Pts',(1.66135211026155,2.76934413845836,11.1845500735121));
#13856=CARTESIAN_POINT('Ctrl Pts',(1.58217056302627,2.68456642395089,11.1786970521839));
#13857=CARTESIAN_POINT('Ctrl Pts',(1.50296260721615,2.59976043443874,11.1728420787601));
#13858=CARTESIAN_POINT('Ctrl Pts',(1.4275433704603,2.51148049548473,11.1669871053363));
#13859=CARTESIAN_POINT('Ctrl Pts',(1.35621666378742,2.42010821931617,11.1611321319125));
#13860=CARTESIAN_POINT('Ctrl Pts',(1.28480911745379,2.32863238440851,11.1552705226283));
#13861=CARTESIAN_POINT('Ctrl Pts',(1.21750361344906,2.23405754283284,11.1494089133442));
#13862=CARTESIAN_POINT('Ctrl Pts',(1.15456159309431,2.13679567922992,11.14354730406));
#13863=CARTESIAN_POINT('Ctrl Pts',(1.09157713047297,2.03946823123806,11.1376817422496));
#13864=CARTESIAN_POINT('Ctrl Pts',(1.03296221870713,1.93945050892894,11.1318161804393));
#13865=CARTESIAN_POINT('Ctrl Pts',(0.978932307255291,1.83717903641928,11.1259506186289));
#13866=CARTESIAN_POINT('Ctrl Pts',(0.924823390821317,1.73475801793329,11.1200764799286));
#13867=CARTESIAN_POINT('Ctrl Pts',(0.875313030951348,1.63007704422919,11.1142023412283));
#13868=CARTESIAN_POINT('Ctrl Pts',(0.830568579634417,1.52359258705176,11.108328202528));
#13869=CARTESIAN_POINT('Ctrl Pts',(0.819253438354853,1.49666440620301,11.1068427287467));
#13870=CARTESIAN_POINT('Ctrl Pts',(0.80824282790806,1.46962096545336,11.1053572549654));
#13871=CARTESIAN_POINT('Ctrl Pts',(0.797538944724832,1.44246978246123,11.1038717811841));
#13872=CARTESIAN_POINT('Ctrl Pts',(0.755214882272451,1.33511170082453,11.0979980917935));
#13873=CARTESIAN_POINT('Ctrl Pts',(0.717549385894021,1.22571046622653,11.0921244024029));
#13874=CARTESIAN_POINT('Ctrl Pts',(0.684743315654432,1.1147078365185,11.0862507130124));
#13875=CARTESIAN_POINT('Ctrl Pts',(0.651979601133517,1.00384852163365,11.0803846071066));
#13876=CARTESIAN_POINT('Ctrl Pts',(0.624062951896819,0.891392315905969,
11.0745185012009));
#13877=CARTESIAN_POINT('Ctrl Pts',(0.601146189443547,0.777800879011969,
11.0686523952951));
#13878=CARTESIAN_POINT('Ctrl Pts',(0.578252893463033,0.664325758302029,
11.0627922962071));
#13879=CARTESIAN_POINT('Ctrl Pts',(0.56034938173798,0.549718121237769,11.056932197119));
#13880=CARTESIAN_POINT('Ctrl Pts',(0.547538477608263,0.43445407204298,11.051072098031));
#13881=CARTESIAN_POINT('Ctrl Pts',(0.534265385283906,0.315031558912717,
11.0450005799369));
#13882=CARTESIAN_POINT('Ctrl Pts',(0.526459425701012,0.194904808852119,
11.0389290618428));
#13883=CARTESIAN_POINT('Ctrl Pts',(0.524176940102534,0.0746144778509115,
11.0328575437487));
#13884=CARTESIAN_POINT('Ctrl Pts',(0.521976466035727,-0.0413537254237361,
11.0270041801519));
#13885=CARTESIAN_POINT('Ctrl Pts',(0.524909379816371,-0.157473508273641,
11.0211508165552));
#13886=CARTESIAN_POINT('Ctrl Pts',(0.532973249020587,-0.273256763050374,
11.0152974529584));
#13887=CARTESIAN_POINT('Ctrl Pts',(0.541035907461977,-0.389022633361006,
11.0094449682245));
#13888=CARTESIAN_POINT('Ctrl Pts',(0.554227960794191,-0.504451664032298,
11.0035924834906));
#13889=CARTESIAN_POINT('Ctrl Pts',(0.572494928317955,-0.61905862840584,
10.9977399987567));
#13890=CARTESIAN_POINT('Ctrl Pts',(0.590763570677339,-0.733676100698993,
10.9918869774286));
#13891=CARTESIAN_POINT('Ctrl Pts',(0.614107987171045,-0.847470948843617,
10.9860339561004));
#13892=CARTESIAN_POINT('Ctrl Pts',(0.642422296087036,-0.95996662969496,
10.9801809347722));
#13893=CARTESIAN_POINT('Ctrl Pts',(0.670746048371866,-1.07249983002843,
10.9743259613484));
#13894=CARTESIAN_POINT('Ctrl Pts',(0.704042888267363,-1.18373260104292,
10.9684709879246));
#13895=CARTESIAN_POINT('Ctrl Pts',(0.742156842872519,-1.29320277232904,
10.9626160145008));
#13896=CARTESIAN_POINT('Ctrl Pts',(0.780313994749741,-1.4027970139936,10.9567544052167));
#13897=CARTESIAN_POINT('Ctrl Pts',(0.823299022409682,-1.51062427828903,
10.9508927959325));
#13898=CARTESIAN_POINT('Ctrl Pts',(0.870907461752496,-1.61624153322949,
10.9450311866484));
#13899=CARTESIAN_POINT('Ctrl Pts',(0.918548003815678,-1.7219300066608,10.939165624838));
#13900=CARTESIAN_POINT('Ctrl Pts',(0.9708179795764,-1.82540513551408,10.9333000630277));
#13901=CARTESIAN_POINT('Ctrl Pts',(1.02746737159447,-1.92624923204322,10.9274345012173));
#13902=CARTESIAN_POINT('Ctrl Pts',(1.08419959891766,-2.02724078737479,10.921560362517));
#13903=CARTESIAN_POINT('Ctrl Pts',(1.14532380559521,-2.12559328275801,10.9156862238167));
#13904=CARTESIAN_POINT('Ctrl Pts',(1.2105471379429,-2.22091863332889,10.9098120851164));
#13905=CARTESIAN_POINT('Ctrl Pts',(1.22704105391523,-2.24502485829095,10.908326611335));
#13906=CARTESIAN_POINT('Ctrl Pts',(1.2437969127476,-2.26893766709304,10.9068411375537));
#13907=CARTESIAN_POINT('Ctrl Pts',(1.26080958799867,-2.29265113866297,10.9053556637724));
#13908=CARTESIAN_POINT('Ctrl Pts',(1.32807914965896,-2.38641621760626,10.8994819743818));
#13909=CARTESIAN_POINT('Ctrl Pts',(1.39959104176202,-2.47737427957364,10.8936082849913));
#13910=CARTESIAN_POINT('Ctrl Pts',(1.47508293987044,-2.56511705914367,10.8877345956007));
#13911=CARTESIAN_POINT('Ctrl Pts',(1.55047737084619,-2.65274655454214,10.881868489695));
#13912=CARTESIAN_POINT('Ctrl Pts',(1.62984132191935,-2.7371687126603,10.8760023837892));
#13913=CARTESIAN_POINT('Ctrl Pts',(1.71286970282923,-2.81800484629168,10.8701362778835));
#13914=CARTESIAN_POINT('Ctrl Pts',(1.79581306373443,-2.89875820475167,10.8642761787955));
#13915=CARTESIAN_POINT('Ctrl Pts',(1.88241309652198,-2.97593255623304,10.8584160797075));
#13916=CARTESIAN_POINT('Ctrl Pts',(1.97232546858703,-3.04918339684846,10.8525559806195));
#13917=CARTESIAN_POINT('Ctrl Pts',(2.06548167391382,-3.12507696068184,10.8464844625253));
#13918=CARTESIAN_POINT('Ctrl Pts',(2.16219343971655,-3.19675822350879,10.8404129444312));
#13919=CARTESIAN_POINT('Ctrl Pts',(2.26203699164811,-3.26388674658653,10.8343414263371));
#13920=CARTESIAN_POINT('Ctrl Pts',(2.35829308496563,-3.3286032881822,10.8284880627404));
#13921=CARTESIAN_POINT('Ctrl Pts',(2.45745941016552,-3.38908837641634,10.8226346991436));
#13922=CARTESIAN_POINT('Ctrl Pts',(2.55912448792039,-3.44507944747522,10.8167813355469));
#13923=CARTESIAN_POINT('Ctrl Pts',(2.66077430100596,-3.50106211166319,10.810928850813));
#13924=CARTESIAN_POINT('Ctrl Pts',(2.76492175885539,-3.55255190110082,10.8050763660791));
#13925=CARTESIAN_POINT('Ctrl Pts',(2.87112958719468,-3.59933155036072,10.7992238813452));
#13926=CARTESIAN_POINT('Ctrl Pts',(2.97734715336553,-3.64611548868623,10.793370860017));
#13927=CARTESIAN_POINT('Ctrl Pts',(3.08562508744303,-3.68818826180115,10.7875178386889));
#13928=CARTESIAN_POINT('Ctrl Pts',(3.19550554699996,-3.72538050436778,10.7816648173607));
#13929=CARTESIAN_POINT('Ctrl Pts',(3.30542265381301,-3.76258515126585,10.7758098439369));
#13930=CARTESIAN_POINT('Ctrl Pts',(3.41694295775744,-3.79490589851757,10.7699548705131));
#13931=CARTESIAN_POINT('Ctrl Pts',(3.52959353901836,-3.82222326440095,10.7640998970892));
#13932=CARTESIAN_POINT('Ctrl Pts',(3.64237179524336,-3.84957159100969,10.758238287805));
#13933=CARTESIAN_POINT('Ctrl Pts',(3.75628248389902,-3.87190512047532,10.7523766785209));
#13934=CARTESIAN_POINT('Ctrl Pts',(3.87084247979791,-3.88915549373222,10.7465150692367));
#13935=CARTESIAN_POINT('Ctrl Pts',(3.98547972434332,-3.90641749904248,10.7406495074264));
#13936=CARTESIAN_POINT('Ctrl Pts',(4.10076673810925,-3.91858947974171,10.734783945616));
#13937=CARTESIAN_POINT('Ctrl Pts',(4.21621699797274,-3.92565509494703,10.7289183838057));
#13938=CARTESIAN_POINT('Ctrl Pts',(4.3318360744321,-3.93273104181473,10.7230442451054));
#13939=CARTESIAN_POINT('Ctrl Pts',(4.44761846188777,-3.93468571446805,10.717170106405));
#13940=CARTESIAN_POINT('Ctrl Pts',(4.56307929081561,-3.9315548156601,10.7112959677047));
#13941=CARTESIAN_POINT('Ctrl Pts',(4.59227744953982,-3.93076306246386,10.7098104939234));
#13942=CARTESIAN_POINT('Ctrl Pts',(4.62145508086281,-3.9296463438869,10.7083250201421));
#13943=CARTESIAN_POINT('Ctrl Pts',(4.65060443016853,-3.92820575784858,10.7068395463608));
#13944=CARTESIAN_POINT('Ctrl Pts',(4.76586343097591,-3.92250955840301,10.7009658569702));
#13945=CARTESIAN_POINT('Ctrl Pts',(4.88106348107307,-3.91172678479573,10.6950921675796));
#13946=CARTESIAN_POINT('Ctrl Pts',(4.99571930325014,-3.89585654574203,10.6892184781891));
#13947=CARTESIAN_POINT('Ctrl Pts',(5.11022709398941,-3.88000679665789,10.6833523722833));
#13948=CARTESIAN_POINT('Ctrl Pts',(5.22419164864235,-3.85908270064155,10.6774862663775));
#13949=CARTESIAN_POINT('Ctrl Pts',(5.33712936104568,-3.83313533749687,10.6716201604718));
#13950=CARTESIAN_POINT('Ctrl Pts',(5.44995142667033,-3.80721454412148,10.6657600613837));
#13951=CARTESIAN_POINT('Ctrl Pts',(5.56174834125169,-3.77628080694555,10.6598999622957));
#13952=CARTESIAN_POINT('Ctrl Pts',(5.67204394948978,-3.74043671252507,10.6540398632076));
#13953=CARTESIAN_POINT('Ctrl Pts',(5.78631877164823,-3.70329944495148,10.6479683451135));
#13954=CARTESIAN_POINT('Ctrl Pts',(5.89898146736717,-3.66089088356993,10.6418968270194));
#13955=CARTESIAN_POINT('Ctrl Pts',(6.00951623119543,-3.61338257420939,10.6358253089253));
#13956=CARTESIAN_POINT('Ctrl Pts',(6.11607939262224,-3.56758127637184,10.6299719453285));
#13957=CARTESIAN_POINT('Ctrl Pts',(6.22066449496693,-3.51704057673367,10.6241185817318));
#13958=CARTESIAN_POINT('Ctrl Pts',(6.32282783693948,-3.46196390626197,10.618265218135));
#13959=CARTESIAN_POINT('Ctrl Pts',(6.42497583942988,-3.40689550536707,10.6124127334011));
#13960=CARTESIAN_POINT('Ctrl Pts',(6.52470244099266,-3.34729268384366,10.6065602486672));
#13961=CARTESIAN_POINT('Ctrl Pts',(6.62158802124141,-3.28340510504094,10.6007077639333));
#13962=CARTESIAN_POINT('Ctrl Pts',(6.71848248459706,-3.21951166860502,10.5948547426052));
#13963=CARTESIAN_POINT('Ctrl Pts',(6.81253506389509,-3.1513329213804,10.589001721277));
#13964=CARTESIAN_POINT('Ctrl Pts',(6.90335523937891,-3.07916177739106,10.5831486999488));
#13965=CARTESIAN_POINT('Ctrl Pts',(6.99420570514549,-3.00696656293117,10.577293726525));
#13966=CARTESIAN_POINT('Ctrl Pts',(7.08182130012722,-2.9307765608921,10.5714387531012));
#13967=CARTESIAN_POINT('Ctrl Pts',(7.16584524856595,-2.85092439732749,10.5655837796773));
#13968=CARTESIAN_POINT('Ctrl Pts',(7.24996442735755,-2.7709817315923,10.5597221703932));
#13969=CARTESIAN_POINT('Ctrl Pts',(7.3304835351489,-2.68736890477215,10.553860561109));
#13970=CARTESIAN_POINT('Ctrl Pts',(7.4070832225216,-2.60045483265358,10.5479989518248));
#13971=CARTESIAN_POINT('Ctrl Pts',(7.48373456162614,-2.5134821537378,10.5421333900145));
#13972=CARTESIAN_POINT('Ctrl Pts',(7.55646095918195,-2.42320411789421,10.5362678282041));
#13973=CARTESIAN_POINT('Ctrl Pts',(7.62498493500465,-2.3300206957729,10.5304022663938));
#13974=CARTESIAN_POINT('Ctrl Pts',(7.6936091096864,-2.23670101663399,10.5245281276935));
#13975=CARTESIAN_POINT('Ctrl Pts',(7.75801836990249,-2.14046781452328,10.5186539889932));
#13976=CARTESIAN_POINT('Ctrl Pts',(7.81797986457587,-2.04174788390877,10.5127798502928));
#13977=CARTESIAN_POINT('Ctrl Pts',(7.83314314769978,-2.01678322507173,10.5112943765116));
#13978=CARTESIAN_POINT('Ctrl Pts',(7.84802223176479,-1.99165964874738,10.5098089027303));
#13979=CARTESIAN_POINT('Ctrl Pts',(7.86261383551002,-1.96638426639298,10.5083234289491));
#13980=CARTESIAN_POINT('Ctrl Pts',(7.92264529898111,-1.86239856207853,10.5022120263511));
#13981=CARTESIAN_POINT('Ctrl Pts',(7.97799354213095,-1.75551901299705,10.4961006237532));
#13982=CARTESIAN_POINT('Ctrl Pts',(8.02838127406931,-1.64618725094005,10.4899892211553));
#13983=CARTESIAN_POINT('Ctrl Pts',(8.07868495492499,-1.53703786369172,10.483888012904));
#13984=CARTESIAN_POINT('Ctrl Pts',(8.12404444964126,-1.4254447391088,10.4777868046527));
#13985=CARTESIAN_POINT('Ctrl Pts',(8.16422736076993,-1.31187565180693,10.4716855964014));
#13986=CARTESIAN_POINT('Ctrl Pts',(8.20432760106104,-1.19854021735164,10.4655969405506));
#13987=CARTESIAN_POINT('Ctrl Pts',(8.23927236440555,-1.08323726646985,10.4595082846999));
#13988=CARTESIAN_POINT('Ctrl Pts',(8.26887690552271,-0.96645526114898,10.4534196288492));
#13989=CARTESIAN_POINT('Ctrl Pts',(8.29844538206055,-0.849815520958192,
10.4473383902663));
#13990=CARTESIAN_POINT('Ctrl Pts',(8.32268649854621,-0.731700666397014,
10.4412571516834));
#13991=CARTESIAN_POINT('Ctrl Pts',(8.34146469134731,-0.612615951088222,
10.4351759131006));
#13992=CARTESIAN_POINT('Ctrl Pts',(8.36021580031284,-0.493702991969284,
10.4291034455037));
#13993=CARTESIAN_POINT('Ctrl Pts',(8.37351963251434,-0.373823320362487,
10.4230309779068));
#13994=CARTESIAN_POINT('Ctrl Pts',(8.38129141016021,-0.253493357861161,
10.41695851031));
#13995=CARTESIAN_POINT('Ctrl Pts',(8.38674991623802,-0.168979638917392,
10.4126935142183));
#13996=CARTESIAN_POINT('Ctrl Pts',(8.38948053515783,-0.0842440801685602,
10.4084285181267));
#13997=CARTESIAN_POINT('Ctrl Pts',(8.38946907025248,0.000531889783886232,
10.404163522035));
#13998=CARTESIAN_POINT('',(8.39098612953365,0.00160391675724327,12.904163522035));
#13999=CARTESIAN_POINT('Ctrl Pts',(8.39513361690685,0.00160560749195398,
12.904163522035));
#14000=CARTESIAN_POINT('Ctrl Pts',(8.39559657037226,0.0911727952049497,
12.8996146273196));
#14001=CARTESIAN_POINT('Ctrl Pts',(8.35221472178778,1.48320304232387,12.8288936934674));
#14002=CARTESIAN_POINT('Ctrl Pts',(6.70306870781759,4.07019284841877,12.6920007204769));
#14003=CARTESIAN_POINT('Ctrl Pts',(2.2541571275096,4.09432552951761,12.4934846030659));
#14004=CARTESIAN_POINT('Ctrl Pts',(-0.177919035112619,0.368952773014312,
12.2949684856539));
#14005=CARTESIAN_POINT('Ctrl Pts',(1.63408930668588,-3.69429991478975,12.0964523682425));
#14006=CARTESIAN_POINT('Ctrl Pts',(6.03077938153972,-4.37438301366497,11.8979362508306));
#14007=CARTESIAN_POINT('Ctrl Pts',(8.22530950611016,-1.90438093581909,11.7505066354283));
#14008=CARTESIAN_POINT('Ctrl Pts',(8.39241825399927,-0.301695760422687,
11.669249059163));
#14009=CARTESIAN_POINT('Ctrl Pts',(8.38967060075818,-0.00358974949148719,
11.654163522035));
#14010=CARTESIAN_POINT('',(8.38946824069671,0.0026092511641729,14.1541635219886));
#14011=CARTESIAN_POINT('Ctrl Pts',(8.38946824069672,0.0026092511641433,
14.1541635219886));
#14012=CARTESIAN_POINT('Ctrl Pts',(8.38938088713637,0.134279778690723,14.1475286566465));
#14013=CARTESIAN_POINT('Ctrl Pts',(8.38267733111356,0.265695130310272,14.1408937913045));
#14014=CARTESIAN_POINT('Ctrl Pts',(8.36945840043487,0.396237029246539,14.1342589259624));
#14015=CARTESIAN_POINT('Ctrl Pts',(8.35618100728446,0.527356267020553,14.1275947170496));
#14016=CARTESIAN_POINT('Ctrl Pts',(8.33633059839447,0.6575941279414,14.1209305081367));
#14017=CARTESIAN_POINT('Ctrl Pts',(8.31005900525452,0.786342094794398,14.1142662992239));
#14018=CARTESIAN_POINT('Ctrl Pts',(8.28363708409889,0.915826767117691,14.1075639572106));
#14019=CARTESIAN_POINT('Ctrl Pts',(8.2507203850698,1.04380426791905,14.1008616151973));
#14020=CARTESIAN_POINT('Ctrl Pts',(8.21151184783421,1.16967645468195,14.0941592731839));
#14021=CARTESIAN_POINT('Ctrl Pts',(8.18704777476732,1.24821410467266,14.0899773629089));
#14022=CARTESIAN_POINT('Ctrl Pts',(8.16013517678839,1.32593255787288,14.0857954526339));
#14023=CARTESIAN_POINT('Ctrl Pts',(8.13083256144065,1.40269105612251,14.0816135423589));
#14024=CARTESIAN_POINT('Ctrl Pts',(8.089675661946,1.51050197198552,14.0757398529683));
#14025=CARTESIAN_POINT('Ctrl Pts',(8.0437012121607,1.61667951064595,14.0698661635778));
#14026=CARTESIAN_POINT('Ctrl Pts',(7.99305884784686,1.72076204032031,14.0639924741872));
#14027=CARTESIAN_POINT('Ctrl Pts',(7.94248186758305,1.82471018967061,14.0581263682814));
#14028=CARTESIAN_POINT('Ctrl Pts',(7.88724913706096,1.92656834099077,14.0522602623757));
#14029=CARTESIAN_POINT('Ctrl Pts',(7.82755918302191,2.02589256725915,14.0463941564699));
#14030=CARTESIAN_POINT('Ctrl Pts',(7.7679303507354,2.12511508678516,14.0405340573819));
#14031=CARTESIAN_POINT('Ctrl Pts',(7.7038535849314,2.22180849033266,14.0346739582939));
#14032=CARTESIAN_POINT('Ctrl Pts',(7.63557406957853,2.31555190655232,14.0288138592059));
#14033=CARTESIAN_POINT('Ctrl Pts',(7.56483118508216,2.41267737136631,14.0227423411117));
#14034=CARTESIAN_POINT('Ctrl Pts',(7.48957677189747,2.50663556622635,14.0166708230176));
#14035=CARTESIAN_POINT('Ctrl Pts',(7.41013386930994,2.59698930827036,14.0105993049235));
#14036=CARTESIAN_POINT('Ctrl Pts',(7.33354541370155,2.68409656815383,14.0047459413268));
#14037=CARTESIAN_POINT('Ctrl Pts',(7.25306457641055,2.76785360237372,13.99889257773));
#14038=CARTESIAN_POINT('Ctrl Pts',(7.16902235077852,2.84790166533635,13.9930392141333));
#14039=CARTESIAN_POINT('Ctrl Pts',(7.08499274380386,2.9279377093517,13.9871867293994));
#14040=CARTESIAN_POINT('Ctrl Pts',(6.99740311081283,3.00426560454971,13.9813342446655));
#14041=CARTESIAN_POINT('Ctrl Pts',(6.90662093107597,3.07656383570151,13.9754817599316));
#14042=CARTESIAN_POINT('Ctrl Pts',(6.8158304278321,3.14886869563041,13.9696287386034));
#14043=CARTESIAN_POINT('Ctrl Pts',(6.72184711915271,3.2171428996569,13.9637757172752));
#14044=CARTESIAN_POINT('Ctrl Pts',(6.62507057891049,3.28110601057586,13.957922695947));
#14045=CARTESIAN_POINT('Ctrl Pts',(6.5282617618232,3.34509045442754,13.9520677225232));
#14046=CARTESIAN_POINT('Ctrl Pts',(6.4286582052149,3.40476071842588,13.9462127490994));
#14047=CARTESIAN_POINT('Ctrl Pts',(6.32668677345772,3.45988076053863,13.9403577756756));
#14048=CARTESIAN_POINT('Ctrl Pts',(6.22459977018035,3.51506327413923,13.9344961663914));
#14049=CARTESIAN_POINT('Ctrl Pts',(6.12013989893483,3.56568507604074,13.9286345571073));
#14050=CARTESIAN_POINT('Ctrl Pts',(6.01375691911479,3.61155695895883,13.9227729478231));
#14051=CARTESIAN_POINT('Ctrl Pts',(5.90730220447011,3.65745977362448,13.9169073860128));
#14052=CARTESIAN_POINT('Ctrl Pts',(5.79892218439194,3.69860614533675,13.9110418242024));
#14053=CARTESIAN_POINT('Ctrl Pts',(5.68908315875057,3.73485630212193,13.9051762623921));
#14054=CARTESIAN_POINT('Ctrl Pts',(5.57908352151408,3.7711594655272,13.8993021236917));
#14055=CARTESIAN_POINT('Ctrl Pts',(5.46762101708138,3.80255201393773,13.8934279849914));
#14056=CARTESIAN_POINT('Ctrl Pts',(5.35517360749481,3.82894492247999,13.8875538462911));
#14057=CARTESIAN_POINT('Ctrl Pts',(5.32673749332848,3.83561925818277,13.8860683725098));
#14058=CARTESIAN_POINT('Ctrl Pts',(5.29823842487211,3.84197412459091,13.8845828987285));
#14059=CARTESIAN_POINT('Ctrl Pts',(5.26968418053246,3.84800860743686,13.8830974249473));
#14060=CARTESIAN_POINT('Ctrl Pts',(5.15677827525878,3.87186946470474,13.8772237355567));
#14061=CARTESIAN_POINT('Ctrl Pts',(5.04263326983356,3.89079662734252,13.8713500461661));
#14062=CARTESIAN_POINT('Ctrl Pts',(4.92771819603679,3.90466558047488,13.8654763567756));
#14063=CARTESIAN_POINT('Ctrl Pts',(4.81295148839609,3.91851662748582,13.8596102508698));
#14064=CARTESIAN_POINT('Ctrl Pts',(4.69741709600489,3.92732240320996,13.8537441449641));
#14065=CARTESIAN_POINT('Ctrl Pts',(4.58159567745767,3.93100907416529,13.8478780390583));
#14066=CARTESIAN_POINT('Ctrl Pts',(4.46589285856744,3.93469197001655,13.8420179399703));
#14067=CARTESIAN_POINT('Ctrl Pts',(4.34990400861627,3.9332661746028,13.8361578408822));
#14068=CARTESIAN_POINT('Ctrl Pts',(4.23411570566302,3.92670955957549,13.8302977417942));
#14069=CARTESIAN_POINT('Ctrl Pts',(4.11415002489481,3.91991639683605,13.8242262237001));
#14070=CARTESIAN_POINT('Ctrl Pts',(3.99440008331198,3.90761515397094,13.818154705606));
#14071=CARTESIAN_POINT('Ctrl Pts',(3.87540837177331,3.88984028243916,13.8120831875119));
#14072=CARTESIAN_POINT('Ctrl Pts',(3.76069212752601,3.87270407624683,13.8062298239151));
#14073=CARTESIAN_POINT('Ctrl Pts',(3.64668100706311,3.85048088198604,13.8003764603183));
#14074=CARTESIAN_POINT('Ctrl Pts',(3.53385590176067,3.82325435656072,13.7945230967216));
#14075=CARTESIAN_POINT('Ctrl Pts',(3.42104773676812,3.79603191910658,13.7886706119877));
#14076=CARTESIAN_POINT('Ctrl Pts',(3.30942563436249,3.76380774111252,13.7828181272538));
#14077=CARTESIAN_POINT('Ctrl Pts',(3.19945898032121,3.72671632182976,13.7769656425199));
#14078=CARTESIAN_POINT('Ctrl Pts',(3.08948224381425,3.68962150176186,13.7711126211917));
#14079=CARTESIAN_POINT('Ctrl Pts',(2.98116164889807,3.64765868533161,13.7652595998635));
#14080=CARTESIAN_POINT('Ctrl Pts',(2.87494946195351,3.60101160992363,13.7594065785354));
#14081=CARTESIAN_POINT('Ctrl Pts',(2.76870185119335,3.55434897681511,13.7535516051115));
#14082=CARTESIAN_POINT('Ctrl Pts',(2.66456442474308,3.50299914422549,13.7476966316877));
#14083=CARTESIAN_POINT('Ctrl Pts',(2.56296693781071,3.44719284900569,13.7418416582639));
#14084=CARTESIAN_POINT('Ctrl Pts',(2.46125430317672,3.39132330451836,13.7359800489797));
#14085=CARTESIAN_POINT('Ctrl Pts',(2.36208771607841,3.33098741526799,13.7301184396956));
#14086=CARTESIAN_POINT('Ctrl Pts',(2.2658699877265,3.266460546534,13.7242568304114));
#14087=CARTESIAN_POINT('Ctrl Pts',(2.16958737905366,3.20189016685848,13.7183912686011));
#14088=CARTESIAN_POINT('Ctrl Pts',(2.07625792033225,3.13312342495535,13.7125257067907));
#14089=CARTESIAN_POINT('Ctrl Pts',(1.98625184864325,3.06047638454844,13.7066601449804));
#14090=CARTESIAN_POINT('Ctrl Pts',(1.89611416600202,2.9877231163506,13.70078600628));
#14091=CARTESIAN_POINT('Ctrl Pts',(1.80930987745507,2.91107849827482,13.6949118675797));
#14092=CARTESIAN_POINT('Ctrl Pts',(1.72617289907127,2.83089590434527,13.6890377288794));
#14093=CARTESIAN_POINT('Ctrl Pts',(1.70514891445961,2.81061903533139,13.6875522550981));
#14094=CARTESIAN_POINT('Ctrl Pts',(1.68435925428379,2.79011607799048,13.6860667813168));
#14095=CARTESIAN_POINT('Ctrl Pts',(1.66380890355829,2.76939307294563,13.6845813075356));
#14096=CARTESIAN_POINT('Ctrl Pts',(1.58255107285719,2.68745255241415,13.678707618145));
#14097=CARTESIAN_POINT('Ctrl Pts',(1.50476733649224,2.60179620351846,13.6728339287545));
#14098=CARTESIAN_POINT('Ctrl Pts',(1.43081659187915,2.51275065664571,13.6669602393639));
#14099=CARTESIAN_POINT('Ctrl Pts',(1.35696132462476,2.4238200759395,13.6610941334581));
#14100=CARTESIAN_POINT('Ctrl Pts',(1.28692946921923,2.33150931416306,13.6552280275524));
#14101=CARTESIAN_POINT('Ctrl Pts',(1.22104363811249,2.23618224667236,13.6493619216466));
#14102=CARTESIAN_POINT('Ctrl Pts',(1.15522527325745,2.14095279288434,13.6435018225586));
#14103=CARTESIAN_POINT('Ctrl Pts',(1.09354472160275,2.04271351482773,13.6376417234706));
#14104=CARTESIAN_POINT('Ctrl Pts',(1.03628435636688,1.94186129187543,13.6317816243825));
#14105=CARTESIAN_POINT('Ctrl Pts',(0.97695816778506,1.8373705507997,13.6257101062884));
#14106=CARTESIAN_POINT('Ctrl Pts',(0.922377416420168,1.73007511443088,13.6196385881943));
#14107=CARTESIAN_POINT('Ctrl Pts',(0.872807241895047,1.62044951855822,13.6135670701002));
#14108=CARTESIAN_POINT('Ctrl Pts',(0.825018163356123,1.51476285795587,13.6077137065035));
#14109=CARTESIAN_POINT('Ctrl Pts',(0.78188597511973,1.40691101378852,13.6018603429067));
#14110=CARTESIAN_POINT('Ctrl Pts',(0.743601075421737,1.29734343405639,13.59600697931));
#14111=CARTESIAN_POINT('Ctrl Pts',(0.705321924072611,1.18779230552768,13.5901544945761));
#14112=CARTESIAN_POINT('Ctrl Pts',(0.671888750357873,1.07652634357975,13.5843020098422));
#14113=CARTESIAN_POINT('Ctrl Pts',(0.643442991995572,0.964012890088044,
13.5784495251083));
#14114=CARTESIAN_POINT('Ctrl Pts',(0.614994625539152,0.851489120623304,
13.5725965037801));
#14115=CARTESIAN_POINT('Ctrl Pts',(0.591534684734126,0.73771803280579,13.5667434824519));
#14116=CARTESIAN_POINT('Ctrl Pts',(0.573153951520933,0.623179275408091,
13.5608904611238));
#14117=CARTESIAN_POINT('Ctrl Pts',(0.554767087978247,0.508602317122839,
13.5550354876999));
#14118=CARTESIAN_POINT('Ctrl Pts',(0.541462865925302,0.393257587853534,
13.5491805142761));
#14119=CARTESIAN_POINT('Ctrl Pts',(0.533280369761308,0.277631298915275,
13.5433255408523));
#14120=CARTESIAN_POINT('Ctrl Pts',(0.525088599788914,0.161873962430134,
13.5374639315682));
#14121=CARTESIAN_POINT('Ctrl Pts',(0.522030170953809,0.0458348416930943,
13.531602322284));
#14122=CARTESIAN_POINT('Ctrl Pts',(0.524092059439312,-0.0699982997375622,
13.5257407129999));
#14123=CARTESIAN_POINT('Ctrl Pts',(0.526155338271362,-0.18590954830616,
13.5198751511895));
#14124=CARTESIAN_POINT('Ctrl Pts',(0.533345783889082,-0.30161412967183,
13.5140095893792));
#14125=CARTESIAN_POINT('Ctrl Pts',(0.545598514508058,-0.41662958955932,
13.5081440275688));
#14126=CARTESIAN_POINT('Ctrl Pts',(0.557869161624378,-0.53181323025855,
13.5022698888685));
#14127=CARTESIAN_POINT('Ctrl Pts',(0.5752168052218,-0.646305331522023,13.4963957501682));
#14128=CARTESIAN_POINT('Ctrl Pts',(0.597525521411622,-0.759633733637311,
13.4905216114679));
#14129=CARTESIAN_POINT('Ctrl Pts',(0.603167031543545,-0.788292636432428,
13.4890361376866));
#14130=CARTESIAN_POINT('Ctrl Pts',(0.609125554976182,-0.81687719919773,
13.4875506639053));
#14131=CARTESIAN_POINT('Ctrl Pts',(0.615398718150294,-0.845379958307195,
13.486065190124));
#14132=CARTESIAN_POINT('Ctrl Pts',(0.640203337689973,-0.958082286609295,
13.4801915007334));
#14133=CARTESIAN_POINT('Ctrl Pts',(0.670013736544737,-1.06987969207632,
13.4743178113428));
#14134=CARTESIAN_POINT('Ctrl Pts',(0.704750006339644,-1.18029352095403,
13.4684441219523));
#14135=CARTESIAN_POINT('Ctrl Pts',(0.739441428346902,-1.29056479520569,
13.4625780160465));
#14136=CARTESIAN_POINT('Ctrl Pts',(0.779045950960212,-1.39945565478475,
13.4567119101408));
#14137=CARTESIAN_POINT('Ctrl Pts',(0.823432698140038,-1.50649774562664,
13.450845804235));
#14138=CARTESIAN_POINT('Ctrl Pts',(0.867773993856243,-1.61343022673123,
13.444985705147));
#14139=CARTESIAN_POINT('Ctrl Pts',(0.916887616414743,-1.71851732529578,
13.4391256060589));
#14140=CARTESIAN_POINT('Ctrl Pts',(0.970593142171489,-1.82130660880617,
13.4332655069709));
#14141=CARTESIAN_POINT('Ctrl Pts',(1.0262362407756,-1.92780429516568,13.4271939888768));
#14142=CARTESIAN_POINT('Ctrl Pts',(1.08680869349269,-2.03183480538726,13.4211224707827));
#14143=CARTESIAN_POINT('Ctrl Pts',(1.15205547888658,-2.13291809020055,13.4150509526886));
#14144=CARTESIAN_POINT('Ctrl Pts',(1.21495789513734,-2.23036937180675,13.4091975890918));
#14145=CARTESIAN_POINT('Ctrl Pts',(1.28220427665314,-2.32508119855183,13.4033442254951));
#14146=CARTESIAN_POINT('Ctrl Pts',(1.35352016544701,-2.41664992726846,13.3974908618983));
#14147=CARTESIAN_POINT('Ctrl Pts',(1.42482534640019,-2.50820490724864,13.3916383771644));
#14148=CARTESIAN_POINT('Ctrl Pts',(1.50019856589792,-2.59661740170161,13.3857858924305));
#14149=CARTESIAN_POINT('Ctrl Pts',(1.57932378762712,-2.68151520892743,13.3799334076966));
#14150=CARTESIAN_POINT('Ctrl Pts',(1.65845626407677,-2.7664208001423,13.3740803863684));
#14151=CARTESIAN_POINT('Ctrl Pts',(1.7413411449168,-2.84781076127939,13.3682273650402));
#14152=CARTESIAN_POINT('Ctrl Pts',(1.82762459127304,-2.92534878540021,13.3623743437121));
#14153=CARTESIAN_POINT('Ctrl Pts',(1.91393681482496,-3.00291266994949,13.3565193702882));
#14154=CARTESIAN_POINT('Ctrl Pts',(2.00364955065226,-3.07662178692314,13.3506643968644));
#14155=CARTESIAN_POINT('Ctrl Pts',(2.09637541959603,-3.14617971361553,13.3448094234406));
#14156=CARTESIAN_POINT('Ctrl Pts',(2.18920638140203,-3.21581647528342,13.3389478141564));
#14157=CARTESIAN_POINT('Ctrl Pts',(2.28505696177989,-3.28129240803428,13.3330862048723));
#14158=CARTESIAN_POINT('Ctrl Pts',(2.38351022884912,-3.34235403461939,13.3272245955881));
#14159=CARTESIAN_POINT('Ctrl Pts',(2.48202988367942,-3.40345683550777,13.3213590337778));
#14160=CARTESIAN_POINT('Ctrl Pts',(2.58315536031639,-3.46013920165589,13.3154934719674));
#14161=CARTESIAN_POINT('Ctrl Pts',(2.68644607561417,-3.51219411068511,13.3096279101571));
#14162=CARTESIAN_POINT('Ctrl Pts',(2.7898878272714,-3.5643251367586,13.3037537714568));
#14163=CARTESIAN_POINT('Ctrl Pts',(2.89550076099386,-3.61181503274344,13.2978796327564));
#14164=CARTESIAN_POINT('Ctrl Pts',(3.00282527382747,-3.65450524812213,13.2920054940561));
#14165=CARTESIAN_POINT('Ctrl Pts',(3.02996589103708,-3.66530090666834,13.2905200202748));
#14166=CARTESIAN_POINT('Ctrl Pts',(3.0572158956617,-3.67578987601307,13.2890345464936));
#14167=CARTESIAN_POINT('Ctrl Pts',(3.08456772922879,-3.68597010457415,13.2875490727123));
#14168=CARTESIAN_POINT('Ctrl Pts',(3.19271920026875,-3.72622359221341,13.2816753833217));
#14169=CARTESIAN_POINT('Ctrl Pts',(3.30282393812599,-3.7617801169372,13.2758016939311));
#14170=CARTESIAN_POINT('Ctrl Pts',(3.41443640720468,-3.79244734362739,13.2699280045406));
#14171=CARTESIAN_POINT('Ctrl Pts',(3.52590477410022,-3.82307497604686,13.2640618986348));
#14172=CARTESIAN_POINT('Ctrl Pts',(3.63887660628105,-3.84882575554979,13.2581957927291));
#14173=CARTESIAN_POINT('Ctrl Pts',(3.75288739300566,-3.86955575910631,13.2523296868233));
#14174=CARTESIAN_POINT('Ctrl Pts',(3.86678143413708,-3.89026453540327,13.2464695877353));
#14175=CARTESIAN_POINT('Ctrl Pts',(3.98171190960985,-3.90596268857882,13.2406094886472));
#14176=CARTESIAN_POINT('Ctrl Pts',(4.09720082745859,-3.91655656206789,13.2347493895592));
#14177=CARTESIAN_POINT('Ctrl Pts',(4.21685632199092,-3.92753263834395,13.2286778714651));
#14178=CARTESIAN_POINT('Ctrl Pts',(4.33711087880189,-3.93302906002751,13.222606353371));
#14179=CARTESIAN_POINT('Ctrl Pts',(4.45742285917651,-3.93299988435739,13.2165348352769));
#14180=CARTESIAN_POINT('Ctrl Pts',(4.57341193394532,-3.93297175699242,13.2106814716801));
#14181=CARTESIAN_POINT('Ctrl Pts',(4.68945392818294,-3.92780827699206,13.2048281080834));
#14182=CARTESIAN_POINT('Ctrl Pts',(4.80506087108329,-3.91752125475641,13.1989747444867));
#14183=CARTESIAN_POINT('Ctrl Pts',(4.92065045599021,-3.90723577708254,13.1931222597527));
#14184=CARTESIAN_POINT('Ctrl Pts',(5.03580470803506,-3.89182832340444,13.1872697750188));
#14185=CARTESIAN_POINT('Ctrl Pts',(5.15003953691746,-3.87136268743445,13.1814172902849));
#14186=CARTESIAN_POINT('Ctrl Pts',(5.26428483959988,-3.85089517504043,13.1755642689568));
#14187=CARTESIAN_POINT('Ctrl Pts',(5.37761014484924,-3.82536863128895,13.1697112476286));
#14188=CARTESIAN_POINT('Ctrl Pts',(5.48954103188702,-3.79489807457262,13.1638582263004));
#14189=CARTESIAN_POINT('Ctrl Pts',(5.6015092500373,-3.76441735533717,13.1580032528766));
#14190=CARTESIAN_POINT('Ctrl Pts',(5.71208172679141,-3.72898945278671,13.1521482794528));
#14191=CARTESIAN_POINT('Ctrl Pts',(5.8207993738973,-3.68877919110033,13.146293306029));
#14192=CARTESIAN_POINT('Ctrl Pts',(5.92964023849185,-3.64852335624717,13.1404316967448));
#14193=CARTESIAN_POINT('Ctrl Pts',(6.03662168984397,-3.6034744872829,13.1345700874607));
#14194=CARTESIAN_POINT('Ctrl Pts',(6.1413047062946,-3.55384552291111,13.1287084781765));
#14195=CARTESIAN_POINT('Ctrl Pts',(6.24605831127208,-3.50418309336414,13.1228429163662));
#14196=CARTESIAN_POINT('Ctrl Pts',(6.34851003103466,-3.44993461158913,13.1169773545558));
#14197=CARTESIAN_POINT('Ctrl Pts',(6.44824705873924,-3.39135807426041,13.1111117927455));
#14198=CARTESIAN_POINT('Ctrl Pts',(6.54812992644033,-3.33269588366734,13.1052376540452));
#14199=CARTESIAN_POINT('Ctrl Pts',(6.64528983455571,-3.26969323098426,13.0993635153448));
#14200=CARTESIAN_POINT('Ctrl Pts',(6.73934439670868,-3.20265037243659,13.0934893766445));
#14201=CARTESIAN_POINT('Ctrl Pts',(6.76312926002483,-3.18569632799282,13.0920039028632));
#14202=CARTESIAN_POINT('Ctrl Pts',(6.7867157099564,-3.1684841053128,13.090518429082));
#14203=CARTESIAN_POINT('Ctrl Pts',(6.81009792502291,-3.15101894365809,13.0890329553007));
#14204=CARTESIAN_POINT('Ctrl Pts',(6.90165114175847,-3.08263398843694,13.0832165729492));
#14205=CARTESIAN_POINT('Ctrl Pts',(6.9903885444588,-3.01013059775906,13.0774001905977));
#14206=CARTESIAN_POINT('Ctrl Pts',(7.07591125866037,-2.93377091982475,13.0715838082462));
#14207=CARTESIAN_POINT('Ctrl Pts',(7.1613231584205,-2.85751018350073,13.0657749623623));
#14208=CARTESIAN_POINT('Ctrl Pts',(7.24352833801147,-2.77740337089531,13.0599661164783));
#14209=CARTESIAN_POINT('Ctrl Pts',(7.3221579331218,-2.69375510159333,13.0541572705944));
#14210=CARTESIAN_POINT('Ctrl Pts',(7.40070768285688,-2.61019177394015,13.0483543233734));
#14211=CARTESIAN_POINT('Ctrl Pts',(7.47568878007658,-2.52309444557788,13.0425513761524));
#14212=CARTESIAN_POINT('Ctrl Pts',(7.54676702953445,-2.43280655728062,13.0367484289314));
#14213=CARTESIAN_POINT('Ctrl Pts',(7.61779426447069,-2.34258347071195,13.0309496466213));
#14214=CARTESIAN_POINT('Ctrl Pts',(7.68492396188114,-2.24917470849623,13.0251508643112));
#14215=CARTESIAN_POINT('Ctrl Pts',(7.74786078546853,-2.15295838644457,13.0193520820012));
#14216=CARTESIAN_POINT('Ctrl Pts',(7.81077427599178,-2.05677773542754,13.0135554495193));
#14217=CARTESIAN_POINT('Ctrl Pts',(7.86949775114576,-1.95779194581923,13.0077588170374));
#14218=CARTESIAN_POINT('Ctrl Pts',(7.92377838368981,-1.85640926908902,13.0019621845556));
#14219=CARTESIAN_POINT('Ctrl Pts',(7.97805265201111,-1.75503847913882,12.9961662317095));
#14220=CARTESIAN_POINT('Ctrl Pts',(8.02788491442897,-1.65127173294077,12.9903702788634));
#14221=CARTESIAN_POINT('Ctrl Pts',(8.07306802915816,-1.54554237424597,12.9845743260173));
#14222=CARTESIAN_POINT('Ctrl Pts',(8.11825730016423,-1.4397986097447,12.9787775834628));
#14223=CARTESIAN_POINT('Ctrl Pts',(8.15879599961505,-1.33209208974856,12.9729808409082));
#14224=CARTESIAN_POINT('Ctrl Pts',(8.19452523344622,-1.22287586847292,12.9671840983536));
#14225=CARTESIAN_POINT('Ctrl Pts',(8.23028873158198,-1.1135549089348,12.9613817967278));
#14226=CARTESIAN_POINT('Ctrl Pts',(8.261233424001,-1.00272175917822,12.9555794951021));
#14227=CARTESIAN_POINT('Ctrl Pts',(8.28725040532625,-0.890844340165236,
12.9497771934764));
#14228=CARTESIAN_POINT('Ctrl Pts',(8.31328093909956,-0.77890864333394,12.9439718693866));
#14229=CARTESIAN_POINT('Ctrl Pts',(8.33437857391976,-0.665928008763961,
12.9381665452968));
#14230=CARTESIAN_POINT('Ctrl Pts',(8.35048593506992,-0.552378436056247,
12.932361221207));
#14231=CARTESIAN_POINT('Ctrl Pts',(8.36661712325321,-0.438660893598316,
12.9265473095125));
#14232=CARTESIAN_POINT('Ctrl Pts',(8.37774325755507,-0.32437315207909,12.9207333978181));
#14233=CARTESIAN_POINT('Ctrl Pts',(8.38385899917048,-0.209994354059066,
12.9149194861236));
#14234=CARTESIAN_POINT('Ctrl Pts',(8.38763045292072,-0.139459270357369,
12.9113341647608));
#14235=CARTESIAN_POINT('Ctrl Pts',(8.38949751602963,-0.0688895527329186,
12.9077488433979));
#14236=CARTESIAN_POINT('Ctrl Pts',(8.38946877942379,0.00160329820526994,
12.904163522035));
#14237=CARTESIAN_POINT('',(8.38838636610598,-0.00299497982686102,15.4041639340473));
#14238=CARTESIAN_POINT('Ctrl Pts',(8.38946797146284,-0.00298763865733172,
15.404163522035));
#14239=CARTESIAN_POINT('Ctrl Pts',(8.38955615194013,0.113095247154287,15.3983099575575));
#14240=CARTESIAN_POINT('Ctrl Pts',(8.38450072803562,0.229234623628655,15.39245639308));
#14241=CARTESIAN_POINT('Ctrl Pts',(8.37431343004976,0.344941812805024,15.3866028286025));
#14242=CARTESIAN_POINT('Ctrl Pts',(8.36412752979414,0.460633126580709,15.380750067253));
#14243=CARTESIAN_POINT('Ctrl Pts',(8.34881119138193,0.575891960223374,15.3748973059036));
#14244=CARTESIAN_POINT('Ctrl Pts',(8.32842813354715,0.690233504465133,15.3690445445541));
#14245=CARTESIAN_POINT('Ctrl Pts',(8.30804296565823,0.804586885343549,15.3631911773267));
#14246=CARTESIAN_POINT('Ctrl Pts',(8.2825901076265,0.918022381936844,15.3573378100994));
#14247=CARTESIAN_POINT('Ctrl Pts',(8.25218451169293,1.03006483322276,15.351484442872));
#14248=CARTESIAN_POINT('Ctrl Pts',(8.22176844884118,1.14214585435522,15.3456290606631));
#14249=CARTESIAN_POINT('Ctrl Pts',(8.18639636531697,1.25283247866569,15.3397736784541));
#14250=CARTESIAN_POINT('Ctrl Pts',(8.1462330339211,1.36166484783254,15.3339182962452));
#14251=CARTESIAN_POINT('Ctrl Pts',(8.10602142242775,1.4706280437314,15.3280558753168));
#14252=CARTESIAN_POINT('Ctrl Pts',(8.06100720769499,1.57773214729757,15.3221934543884));
#14253=CARTESIAN_POINT('Ctrl Pts',(8.01140333883864,1.68253725122022,15.3163310334599));
#14254=CARTESIAN_POINT('Ctrl Pts',(7.96176576425408,1.78741356999826,15.3104646290284));
#14255=CARTESIAN_POINT('Ctrl Pts',(7.90753251760593,1.8899874145095,15.3045982245968));
#14256=CARTESIAN_POINT('Ctrl Pts',(7.84896164638746,1.98984506052513,15.2987318201653));
#14257=CARTESIAN_POINT('Ctrl Pts',(7.79029697220462,2.08986263148325,15.2928560205153));
#14258=CARTESIAN_POINT('Ctrl Pts',(7.72728102728111,2.18715497353262,15.2869802208654));
#14259=CARTESIAN_POINT('Ctrl Pts',(7.66021429275203,2.2813385938439,15.2811044212155));
#14260=CARTESIAN_POINT('Ctrl Pts',(7.62827708711094,2.32618887127316,15.2783063630866));
#14261=CARTESIAN_POINT('Ctrl Pts',(7.59542187401625,2.37033469463769,15.2755083049577));
#14262=CARTESIAN_POINT('Ctrl Pts',(7.56168410033237,2.41373752515241,15.2727102468289));
#14263=CARTESIAN_POINT('Ctrl Pts',(7.49086169628585,2.50484883641669,15.2668365574383));
#14264=CARTESIAN_POINT('Ctrl Pts',(7.41590794136691,2.59299221037409,15.2609628680477));
#14265=CARTESIAN_POINT('Ctrl Pts',(7.33710065212917,2.67776976170523,15.2550891786572));
#14266=CARTESIAN_POINT('Ctrl Pts',(7.25839511050558,2.76243785725297,15.2492230727514));
#14267=CARTESIAN_POINT('Ctrl Pts',(7.17584620747278,2.84374847230016,15.2433569668457));
#14268=CARTESIAN_POINT('Ctrl Pts',(7.08977335741909,2.92133492099204,15.2374908609399));
#14269=CARTESIAN_POINT('Ctrl Pts',(7.00378864486722,2.99884192214898,15.2316307618519));
#14270=CARTESIAN_POINT('Ctrl Pts',(6.91428746790389,3.07263206734264,15.2257706627638));
#14271=CARTESIAN_POINT('Ctrl Pts',(6.82162714094363,3.14237433651276,15.2199105636758));
#14272=CARTESIAN_POINT('Ctrl Pts',(6.72562384077868,3.21463274764695,15.2138390455817));
#14273=CARTESIAN_POINT('Ctrl Pts',(6.62622944448929,3.28254536113956,15.2077675274876));
#14274=CARTESIAN_POINT('Ctrl Pts',(6.52388049339166,3.34578827127266,15.2016960093935));
#14275=CARTESIAN_POINT('Ctrl Pts',(6.4252090219022,3.40675881310222,15.1958426457967));
#14276=CARTESIAN_POINT('Ctrl Pts',(6.32379204225246,3.46338921298687,15.1899892822));
#14277=CARTESIAN_POINT('Ctrl Pts',(6.22005081781549,3.51543291025725,15.1841359186032));
#14278=CARTESIAN_POINT('Ctrl Pts',(6.11632516977435,3.56746879334157,15.1782834338693));
#14279=CARTESIAN_POINT('Ctrl Pts',(6.01027634002654,3.61491915795506,15.1724309491354));
#14280=CARTESIAN_POINT('Ctrl Pts',(5.90234962745504,3.65758369942617,15.1665784644015));
#14281=CARTESIAN_POINT('Ctrl Pts',(5.79441301945312,3.70025215266289,15.1607254430733));
#14282=CARTESIAN_POINT('Ctrl Pts',(5.68459857059121,3.73813375858043,15.1548724217452));
#14283=CARTESIAN_POINT('Ctrl Pts',(5.57337029236903,3.77107686747101,15.149019400417));
#14284=CARTESIAN_POINT('Ctrl Pts',(5.46210491736823,3.80403096352455,15.1431644269932));
#14285=CARTESIAN_POINT('Ctrl Pts',(5.34942517129391,3.83204317013544,15.1373094535694));
#14286=CARTESIAN_POINT('Ctrl Pts',(5.23580821534284,3.85501226366258,15.1314544801456));
#14287=CARTESIAN_POINT('Ctrl Pts',(5.12206248916535,3.87800738970705,15.1255928708614));
#14288=CARTESIAN_POINT('Ctrl Pts',(5.00737783818905,3.89594791252093,15.1197312615773));
#14289=CARTESIAN_POINT('Ctrl Pts',(4.89223965728508,3.90878408546992,15.1138696522931));
#14290=CARTESIAN_POINT('Ctrl Pts',(4.77702383786034,3.92162891394458,15.1080040904828));
#14291=CARTESIAN_POINT('Ctrl Pts',(4.66135429075987,3.92936251147385,15.1021385286724));
#14292=CARTESIAN_POINT('Ctrl Pts',(4.54571780771183,3.93198724174961,15.0962729668621));
#14293=CARTESIAN_POINT('Ctrl Pts',(4.42991223576386,3.93461581002479,15.0903988281617));
#14294=CARTESIAN_POINT('Ctrl Pts',(4.31414023581944,3.9321206108403,15.0845246894614));
#14295=CARTESIAN_POINT('Ctrl Pts',(4.19888494768118,3.9245559495656,15.0786505507611));
#14296=CARTESIAN_POINT('Ctrl Pts',(4.16973876686725,3.92264297022323,15.0771650769798));
#14297=CARTESIAN_POINT('Ctrl Pts',(4.14062558366268,3.92040605411133,15.0756796031985));
#14298=CARTESIAN_POINT('Ctrl Pts',(4.11155310477521,3.91784659627563,15.0741941294172));
#14299=CARTESIAN_POINT('Ctrl Pts',(3.99659805612459,3.90772628279425,15.0683204400266));
#14300=CARTESIAN_POINT('Ctrl Pts',(3.88189734388171,3.89252541571307,15.062446750636));
#14301=CARTESIAN_POINT('Ctrl Pts',(3.76793592119876,3.87226174904628,15.0565730612455));
#14302=CARTESIAN_POINT('Ctrl Pts',(3.65412163341873,3.85202424467685,15.0507069553397));
#14303=CARTESIAN_POINT('Ctrl Pts',(3.54104514007597,3.82673701144322,15.044840849434));
#14304=CARTESIAN_POINT('Ctrl Pts',(3.42918772774957,3.796469671873,15.0389747435282));
#14305=CARTESIAN_POINT('Ctrl Pts',(3.31744485598842,3.76623332567293,15.0331146444402));
#14306=CARTESIAN_POINT('Ctrl Pts',(3.20691897865755,3.73102712386475,15.0272545453522));
#14307=CARTESIAN_POINT('Ctrl Pts',(3.09808195805375,3.6909718714319,15.0213944462641));
#14308=CARTESIAN_POINT('Ctrl Pts',(2.98531834604353,3.64947151687194,15.01532292817));
#14309=CARTESIAN_POINT('Ctrl Pts',(2.87436819643208,3.60276569939355,15.0092514100759));
#14310=CARTESIAN_POINT('Ctrl Pts',(2.76574034293541,3.55104565572003,15.0031798919818));
#14311=CARTESIAN_POINT('Ctrl Pts',(2.66101557502815,3.50118395454936,14.9973265283851));
#14312=CARTESIAN_POINT('Ctrl Pts',(2.55844949636893,3.44666234909959,14.9914731647883));
#14313=CARTESIAN_POINT('Ctrl Pts',(2.4584776647042,3.38770116740492,14.9856198011916));
#14314=CARTESIAN_POINT('Ctrl Pts',(2.35852084347372,3.32874883853335,14.9797673164577));
#14315=CARTESIAN_POINT('Ctrl Pts',(2.26115785049878,3.26535846866724,14.9739148317238));
#14316=CARTESIAN_POINT('Ctrl Pts',(2.16679840412643,3.19779565888478,14.9680623469899));
#14317=CARTESIAN_POINT('Ctrl Pts',(2.0724303062598,3.13022665449983,14.9622093256617));
#14318=CARTESIAN_POINT('Ctrl Pts',(1.98106663836847,3.05848469024496,14.9563563043336));
#14319=CARTESIAN_POINT('Ctrl Pts',(1.89308637793914,2.98287746787567,14.9505032830054));
#14320=CARTESIAN_POINT('Ctrl Pts',(1.80507677439373,2.90724502903746,14.9446483095816));
#14321=CARTESIAN_POINT('Ctrl Pts',(1.72045313531597,2.82774503781808,14.9387933361578));
#14322=CARTESIAN_POINT('Ctrl Pts',(1.63955919334883,2.74472358221698,14.932938362734));
#14323=CARTESIAN_POINT('Ctrl Pts',(1.5585735684889,2.66160803245965,14.9270767534498));
#14324=CARTESIAN_POINT('Ctrl Pts',(1.48132636632456,2.57496334834026,14.9212151441657));
#14325=CARTESIAN_POINT('Ctrl Pts',(1.40812252651924,2.48517044285445,14.9153535348815));
#14326=CARTESIAN_POINT('Ctrl Pts',(1.33486932482731,2.39531698935324,14.9094879730712));
#14327=CARTESIAN_POINT('Ctrl Pts',(1.26566516051922,2.30231141801716,14.9036224112609));
#14328=CARTESIAN_POINT('Ctrl Pts',(1.20077194179187,2.20656406513521,14.8977568494505));
#14329=CARTESIAN_POINT('Ctrl Pts',(1.13578383326246,2.11067670613952,14.8918827107502));
#14330=CARTESIAN_POINT('Ctrl Pts',(1.07511946643912,2.01203991488976,14.8860085720499));
#14331=CARTESIAN_POINT('Ctrl Pts',(1.01899512277585,1.91108911701067,14.8801344333495));
#14332=CARTESIAN_POINT('Ctrl Pts',(1.00480219249987,1.88556030826061,14.8786489595682));
#14333=CARTESIAN_POINT('Ctrl Pts',(0.99089935715119,1.85988361845691,14.8771634857869));
#14334=CARTESIAN_POINT('Ctrl Pts',(0.977289622341522,1.83406627987411,14.8756780120056));
#14335=CARTESIAN_POINT('Ctrl Pts',(0.923475575964183,1.73198233222459,14.869804322615));
#14336=CARTESIAN_POINT('Ctrl Pts',(0.874068636830534,1.62735788902668,14.8639306332245));
#14337=CARTESIAN_POINT('Ctrl Pts',(0.829316783819315,1.52061008483964,14.8580569438339));
#14338=CARTESIAN_POINT('Ctrl Pts',(0.784622709654518,1.41400010209616,14.8521908379281));
#14339=CARTESIAN_POINT('Ctrl Pts',(0.744571927662193,1.30527258776266,14.8463247320224));
#14340=CARTESIAN_POINT('Ctrl Pts',(0.709366843518082,1.19486971376267,14.8404586261166));
#14341=CARTESIAN_POINT('Ctrl Pts',(0.674197808931618,1.08457989089911,14.8345985270285));
#14342=CARTESIAN_POINT('Ctrl Pts',(0.643864727267642,0.972618512011817,
14.8287384279405));
#14343=CARTESIAN_POINT('Ctrl Pts',(0.618521886189556,0.859447576222089,
14.8228783288524));
#14344=CARTESIAN_POINT('Ctrl Pts',(0.592264733221715,0.742193691253597,
14.8168068107583));
#14345=CARTESIAN_POINT('Ctrl Pts',(0.571364866806784,0.62364174201213,14.8107352926642));
#14346=CARTESIAN_POINT('Ctrl Pts',(0.555937432822474,0.504322976708725,
14.8046637745701));
#14347=CARTESIAN_POINT('Ctrl Pts',(0.541064318870497,0.389291429999682,
14.7988104109734));
#14348=CARTESIAN_POINT('Ctrl Pts',(0.53127720502416,0.273547668375362,14.7929570473766));
#14349=CARTESIAN_POINT('Ctrl Pts',(0.526627067904312,0.157577136350896,
14.7871036837799));
#14350=CARTESIAN_POINT('Ctrl Pts',(0.521977628986904,0.0416240169115701,
14.7812511990459));
#14351=CARTESIAN_POINT('Ctrl Pts',(0.52246364971071,-0.0745553925237044,
14.775398714312));
#14352=CARTESIAN_POINT('Ctrl Pts',(0.528084055618252,-0.190472817542138,
14.7695462295781));
#14353=CARTESIAN_POINT('Ctrl Pts',(0.533704976841559,-0.306400870632207,
14.7636932082499));
#14354=CARTESIAN_POINT('Ctrl Pts',(0.544461199054441,-0.422066478872169,
14.7578401869217));
#14355=CARTESIAN_POINT('Ctrl Pts',(0.560299605357159,-0.53698437645785,
14.7519871655936));
#14356=CARTESIAN_POINT('Ctrl Pts',(0.57614329407421,-0.65194060138138,14.7461321921697));
#14357=CARTESIAN_POINT('Ctrl Pts',(0.597072480948472,-0.766148210722537,
14.7402772187459));
#14358=CARTESIAN_POINT('Ctrl Pts',(0.622982686253195,-0.879130745647937,
14.7344222453221));
#14359=CARTESIAN_POINT('Ctrl Pts',(0.64892225744763,-0.992241331764786,
14.7285606360379));
#14360=CARTESIAN_POINT('Ctrl Pts',(0.679854022439804,-1.10412366925764,
14.7226990267538));
#14361=CARTESIAN_POINT('Ctrl Pts',(0.71562320774221,-1.21431501837661,14.7168374174696));
#14362=CARTESIAN_POINT('Ctrl Pts',(0.751416512468981,-1.32458067033161,
14.7109718556592));
#14363=CARTESIAN_POINT('Ctrl Pts',(0.792053588223949,-1.43315267745741,
14.7051062938489));
#14364=CARTESIAN_POINT('Ctrl Pts',(0.837331609128034,-1.53958850903595,
14.6992407320385));
#14365=CARTESIAN_POINT('Ctrl Pts',(0.882675837603703,-1.64617997590503,
14.6933665933382));
#14366=CARTESIAN_POINT('Ctrl Pts',(0.932674377079799,-1.75062866206402,
14.6874924546379));
#14367=CARTESIAN_POINT('Ctrl Pts',(0.987078584220269,-1.85251677613741,
14.6816183159376));
#14368=CARTESIAN_POINT('Ctrl Pts',(1.00083652005029,-1.87828261684978,14.6801328421563));
#14369=CARTESIAN_POINT('Ctrl Pts',(1.0148759847093,-1.903884856244,14.6786473683751));
#14370=CARTESIAN_POINT('Ctrl Pts',(1.02919253023092,-1.92931704799615,14.6771618945939));
#14371=CARTESIAN_POINT('Ctrl Pts',(1.08580136614753,-2.02987809239909,14.6712882052033));
#14372=CARTESIAN_POINT('Ctrl Pts',(1.14693413516208,-2.12811303680113,14.6654145158127));
#14373=CARTESIAN_POINT('Ctrl Pts',(1.21237474753979,-2.22358736999259,14.6595408264222));
#14374=CARTESIAN_POINT('Ctrl Pts',(1.27773086993911,-2.31893843685057,14.6536747205164));
#14375=CARTESIAN_POINT('Ctrl Pts',(1.34738354359932,-2.41153564287397,14.6478086146106));
#14376=CARTESIAN_POINT('Ctrl Pts',(1.42107093402517,-2.50096919937989,14.6419425087049));
#14377=CARTESIAN_POINT('Ctrl Pts',(1.49468286950171,-2.59031117706298,14.6360824096168));
#14378=CARTESIAN_POINT('Ctrl Pts',(1.57232104269608,-2.67649563197526,14.6302223105288));
#14379=CARTESIAN_POINT('Ctrl Pts',(1.65368087293102,-2.75914246086472,14.6243622114408));
#14380=CARTESIAN_POINT('Ctrl Pts',(1.73797598022944,-2.84477099879301,14.6182906933467));
#14381=CARTESIAN_POINT('Ctrl Pts',(1.82626609711616,-2.92660145977944,14.6122191752526));
#14382=CARTESIAN_POINT('Ctrl Pts',(1.91816723322607,-3.00424909113149,14.6061476571585));
#14383=CARTESIAN_POINT('Ctrl Pts',(2.00676628807001,-3.07910678103463,14.6002942935617));
#14384=CARTESIAN_POINT('Ctrl Pts',(2.09872099172641,-3.15007676361758,14.594440929965));
#14385=CARTESIAN_POINT('Ctrl Pts',(2.19365105627081,-3.21685303873709,14.5885875663682));
#14386=CARTESIAN_POINT('Ctrl Pts',(2.28856686738551,-3.28361928762363,14.5827350816343));
#14387=CARTESIAN_POINT('Ctrl Pts',(2.38645681327443,-3.3461928434337,14.5768825969004));
#14388=CARTESIAN_POINT('Ctrl Pts',(2.48691001064333,-3.40430991083921,14.5710301121665));
#14389=CARTESIAN_POINT('Ctrl Pts',(2.58737241822185,-3.46243230679959,14.5651770908383));
#14390=CARTESIAN_POINT('Ctrl Pts',(2.69039818684172,-3.51609719519131,14.5593240695102));
#14391=CARTESIAN_POINT('Ctrl Pts',(2.79555074866315,-3.56508614335424,14.553471048182));
#14392=CARTESIAN_POINT('Ctrl Pts',(2.90073838089458,-3.61409143027743,14.5476160747582));
#14393=CARTESIAN_POINT('Ctrl Pts',(3.00805384249685,-3.65841750156485,14.5417611013343));
#14394=CARTESIAN_POINT('Ctrl Pts',(3.11704012191982,-3.69789385948559,14.5359061279105));
#14395=CARTESIAN_POINT('Ctrl Pts',(3.22614992329152,-3.73741495878741,14.5300445186264));
#14396=CARTESIAN_POINT('Ctrl Pts',(3.33693393344473,-3.77207523320529,14.5241829093422));
#14397=CARTESIAN_POINT('Ctrl Pts',(3.44891940435672,-3.80175388449577,14.5183213000581));
#14398=CARTESIAN_POINT('Ctrl Pts',(3.56098038789436,-3.83145254831884,14.5124557382477));
#14399=CARTESIAN_POINT('Ctrl Pts',(3.67424404273518,-3.85616281236668,14.5065901764374));
#14400=CARTESIAN_POINT('Ctrl Pts',(3.78822855300604,-3.87581521270592,14.500724614627));
#14401=CARTESIAN_POINT('Ctrl Pts',(3.90237973658759,-3.89549634967455,14.4948504759267));
#14402=CARTESIAN_POINT('Ctrl Pts',(4.01725347098413,-3.91010481078321,14.4889763372263));
#14403=CARTESIAN_POINT('Ctrl Pts',(4.13236389090702,-3.91962304430006,14.483102198526));
#14404=CARTESIAN_POINT('Ctrl Pts',(4.16147343691287,-3.92203005017006,14.4816167247448));
#14405=CARTESIAN_POINT('Ctrl Pts',(4.19059812690308,-3.92411179532528,14.4801312509635));
#14406=CARTESIAN_POINT('Ctrl Pts',(4.2197301326962,-3.92586852281323,14.4786457771823));
#14407=CARTESIAN_POINT('Ctrl Pts',(4.33492055578855,-3.93281477237915,14.4727720877917));
#14408=CARTESIAN_POINT('Ctrl Pts',(4.45060880595631,-3.9346985245286,14.4668983984011));
#14409=CARTESIAN_POINT('Ctrl Pts',(4.56631261571985,-3.93146580850201,14.4610247090106));
#14410=CARTESIAN_POINT('Ctrl Pts',(4.68186704099442,-3.92823726621553,14.4551586031049));
#14411=CARTESIAN_POINT('Ctrl Pts',(4.79743657670266,-3.91990540403825,14.4492924971991));
#14412=CARTESIAN_POINT('Ctrl Pts',(4.91253493122844,-3.90646809320872,14.4434263912934));
#14413=CARTESIAN_POINT('Ctrl Pts',(5.02751542650641,-3.89304454201418,14.4375662922054));
#14414=CARTESIAN_POINT('Ctrl Pts',(5.14202529238277,-3.87452598854531,14.4317061931173));
#14415=CARTESIAN_POINT('Ctrl Pts',(5.25558000903006,-3.85096231674724,14.4258460940292));
#14416=CARTESIAN_POINT('Ctrl Pts',(5.3732315207939,-3.8265485214281,14.4197745759351));
#14417=CARTESIAN_POINT('Ctrl Pts',(5.48985721139359,-3.79671871456854,14.413703057841));
#14418=CARTESIAN_POINT('Ctrl Pts',(5.60492560529334,-3.76158698819158,14.4076315397469));
#14419=CARTESIAN_POINT('Ctrl Pts',(5.71585949983983,-3.72771757281993,14.4017781761502));
#14420=CARTESIAN_POINT('Ctrl Pts',(5.82534565255436,-3.68892081630443,14.3959248125534));
#14421=CARTESIAN_POINT('Ctrl Pts',(5.93292077141457,-3.64535039198415,14.3900714489567));
#14422=CARTESIAN_POINT('Ctrl Pts',(6.04047973823267,-3.60178650961647,14.3842189642228));
#14423=CARTESIAN_POINT('Ctrl Pts',(6.14612785890583,-3.55345053966587,14.3783664794888));
#14424=CARTESIAN_POINT('Ctrl Pts',(6.24942072040807,-3.50054474463248,14.3725139947549));
#14425=CARTESIAN_POINT('Ctrl Pts',(6.35272305247842,-3.44763409884825,14.3666609734268));
#14426=CARTESIAN_POINT('Ctrl Pts',(6.45366932836057,-3.39015298341744,14.3608079520986));
#14427=CARTESIAN_POINT('Ctrl Pts',(6.55183932979794,-3.32834983529911,14.3549549307705));
#14428=CARTESIAN_POINT('Ctrl Pts',(6.65004207282762,-3.26652607463672,14.3490999573466));
#14429=CARTESIAN_POINT('Ctrl Pts',(6.7454663507795,-3.20037763495626,14.3432449839228));
#14430=CARTESIAN_POINT('Ctrl Pts',(6.83772114276442,-3.13019611820804,14.3373900104989));
#14431=CARTESIAN_POINT('Ctrl Pts',(6.93008049370588,-3.05993505972544,14.3315284012148));
#14432=CARTESIAN_POINT('Ctrl Pts',(7.01926285985733,-2.98563205106495,14.3256667919306));
#14433=CARTESIAN_POINT('Ctrl Pts',(7.10491045230746,-2.90761886022311,14.3198051826465));
#14434=CARTESIAN_POINT('Ctrl Pts',(7.19061579755809,-2.82955306451384,14.3139396208361));
#14435=CARTESIAN_POINT('Ctrl Pts',(7.27278133088469,-2.74777239570804,14.3080740590258));
#14436=CARTESIAN_POINT('Ctrl Pts',(7.35108748423156,-2.66264407040588,14.3022084972154));
#14437=CARTESIAN_POINT('Ctrl Pts',(7.42950814038058,-2.57739126661291,14.2963343585151));
#14438=CARTESIAN_POINT('Ctrl Pts',(7.50405788886716,-2.48878135187014,14.2904602198148));
#14439=CARTESIAN_POINT('Ctrl Pts',(7.57445858863925,-2.39721308763156,14.2845860811144));
#14440=CARTESIAN_POINT('Ctrl Pts',(7.59226177631162,-2.37405696846868,14.2831006073331));
#14441=CARTESIAN_POINT('Ctrl Pts',(7.6097998545509,-2.35071179676985,14.2816151335519));
#14442=CARTESIAN_POINT('Ctrl Pts',(7.62706878386022,-2.32718428237573,14.2801296597706));
#14443=CARTESIAN_POINT('Ctrl Pts',(7.69575812185698,-2.23360063515049,14.2742210009985));
#14444=CARTESIAN_POINT('Ctrl Pts',(7.76041482388324,-2.13681774927419,14.2683123422264));
#14445=CARTESIAN_POINT('Ctrl Pts',(7.82072869435389,-2.03721536015154,14.2624036834543));
#14446=CARTESIAN_POINT('Ctrl Pts',(7.88096338697472,-1.93774372541336,14.256502781354));
#14447=CARTESIAN_POINT('Ctrl Pts',(7.93686637664349,-1.83546029194052,14.2506018792537));
#14448=CARTESIAN_POINT('Ctrl Pts',(7.98816869929241,-1.73077641082834,14.2447009771534));
#14449=CARTESIAN_POINT('Ctrl Pts',(8.03941558209937,-1.62620565632571,14.2388064518614));
#14450=CARTESIAN_POINT('Ctrl Pts',(8.08607150902556,-1.51923997635001,14.2329119265695));
#14451=CARTESIAN_POINT('Ctrl Pts',(8.12791203700415,-1.41031762592057,14.2270174012775));
#14452=CARTESIAN_POINT('Ctrl Pts',(8.17100632961496,-1.29813138286778,14.220946244674));
#14453=CARTESIAN_POINT('Ctrl Pts',(8.20899184575389,-1.1838697237963,14.2148750880704));
#14454=CARTESIAN_POINT('Ctrl Pts',(8.24167531083385,-1.06803697901315,14.2088039314669));
#14455=CARTESIAN_POINT('Ctrl Pts',(8.27336048026638,-0.955742271725851,
14.2029182144793));
#14456=CARTESIAN_POINT('Ctrl Pts',(8.3000626598224,-0.841971478732594,14.1970324974917));
#14457=CARTESIAN_POINT('Ctrl Pts',(8.32165562211637,-0.727201620817306,
14.1911467805041));
#14458=CARTESIAN_POINT('Ctrl Pts',(8.34426906941924,-0.607007730854899,
14.1849829040926));
#14459=CARTESIAN_POINT('Ctrl Pts',(8.36127840500552,-0.485718479075838,
14.1788190276811));
#14460=CARTESIAN_POINT('Ctrl Pts',(8.37259849858251,-0.363895015438149,
14.1726551512696));
#14461=CARTESIAN_POINT('Ctrl Pts',(8.3839185921595,-0.24207155180046,14.166491274858));
#14462=CARTESIAN_POINT('Ctrl Pts',(8.38954939326522,-0.119714386616567,
14.1603273984465));
#14463=CARTESIAN_POINT('Ctrl Pts',(8.38946824069733,0.00260925024367313,
14.154163522035));
#14464=CARTESIAN_POINT('',(8.39173482151485,-0.000977378064454105,16.6541631314135));
#14465=CARTESIAN_POINT('Ctrl Pts',(8.39563349011517,-0.000965124593257569,
16.6541624592986));
#14466=CARTESIAN_POINT('Ctrl Pts',(8.39142528971798,1.24797165481331,16.5907106232987));
#14467=CARTESIAN_POINT('Ctrl Pts',(7.07426780414926,3.80700714954901,16.4610867481615));
#14468=CARTESIAN_POINT('Ctrl Pts',(2.71525479979042,4.31066727228104,16.2652908338871));
#14469=CARTESIAN_POINT('Ctrl Pts',(-0.109747265587407,0.873697681739816,
16.0667747164755));
#14470=CARTESIAN_POINT('Ctrl Pts',(1.246904763689,-3.36338762624652,15.8682585990637));
#14471=CARTESIAN_POINT('Ctrl Pts',(5.54281476546621,-4.52034652453288,15.6697424816522));
#14472=CARTESIAN_POINT('Ctrl Pts',(8.11523183285779,-2.19602354770684,15.5150446046431));
#14473=CARTESIAN_POINT('Ctrl Pts',(8.38879516314435,-0.445889532599667,
15.4265187667713));
#14474=CARTESIAN_POINT('Ctrl Pts',(8.38567196030232,-0.00301340328699777,
15.4041649680368));
#14475=CARTESIAN_POINT('',(8.38946746866507,0.00358900970105028,17.9041634947166));
#14476=CARTESIAN_POINT('Ctrl Pts',(8.38946746866507,0.00358900970105028,
17.9041634947166));
#14477=CARTESIAN_POINT('Ctrl Pts',(8.38933295163775,0.150998822502151,17.8967107583277));
#14478=CARTESIAN_POINT('Ctrl Pts',(8.3809074565855,0.298039767866117,17.8892580219388));
#14479=CARTESIAN_POINT('Ctrl Pts',(8.36433627259726,0.443918021640171,17.8818052855499));
#14480=CARTESIAN_POINT('Ctrl Pts',(8.34741428627491,0.592884433264276,17.8741947790631));
#14481=CARTESIAN_POINT('Ctrl Pts',(8.32199808271087,0.740638646204888,17.8665842725763));
#14482=CARTESIAN_POINT('Ctrl Pts',(8.28829050128427,0.886359857120285,17.8589737660894));
#14483=CARTESIAN_POINT('Ctrl Pts',(8.28009079873932,0.921807982836407,17.8571224351198));
#14484=CARTESIAN_POINT('Ctrl Pts',(8.27140067079434,0.957135906655535,17.8552711041501));
#14485=CARTESIAN_POINT('Ctrl Pts',(8.26222345997328,0.992332000327834,17.8534197731804));
#14486=CARTESIAN_POINT('Ctrl Pts',(8.23310706386843,1.10399810724074,17.8475460837898));
#14487=CARTESIAN_POINT('Ctrl Pts',(8.19902335211134,1.21456763442564,17.8416723943993));
#14488=CARTESIAN_POINT('Ctrl Pts',(8.16007056424081,1.32356535166693,17.8357987050087));
#14489=CARTESIAN_POINT('Ctrl Pts',(8.12116806807887,1.43242234261535,17.829932599103));
#14490=CARTESIAN_POINT('Ctrl Pts',(8.07740913522595,1.53971117384617,17.8240664931972));
#14491=CARTESIAN_POINT('Ctrl Pts',(8.02894253953352,1.64496886543686,17.8182003872914));
#14492=CARTESIAN_POINT('Ctrl Pts',(7.98052557301757,1.75011877449243,17.8123402882034));
#14493=CARTESIAN_POINT('Ctrl Pts',(7.92741070397869,1.85324130788132,17.8064801891154));
#14494=CARTESIAN_POINT('Ctrl Pts',(7.8697956055742,1.95389129912452,17.8006200900273));
#14495=CARTESIAN_POINT('Ctrl Pts',(7.81010188586044,2.05817251243223,17.7945485719332));
#14496=CARTESIAN_POINT('Ctrl Pts',(7.74557724197532,2.15979898249109,17.7884770538391));
#14497=CARTESIAN_POINT('Ctrl Pts',(7.67649495084179,2.25830081254833,17.782405535745));
#14498=CARTESIAN_POINT('Ctrl Pts',(7.60989484163788,2.35326339313092,17.7765521721482));
#14499=CARTESIAN_POINT('Ctrl Pts',(7.53905922600384,2.44532164376663,17.7706988085515));
#14500=CARTESIAN_POINT('Ctrl Pts',(7.46427786749433,2.53408276415567,17.7648454449547));
#14501=CARTESIAN_POINT('Ctrl Pts',(7.38950773715418,2.62283055736116,17.7589929602208));
#14502=CARTESIAN_POINT('Ctrl Pts',(7.310793308055,2.7082818887986,17.7531404754869));
#14503=CARTESIAN_POINT('Ctrl Pts',(7.2284646833785,2.79007697388514,17.747287990753));
#14504=CARTESIAN_POINT('Ctrl Pts',(7.14612851027254,2.87187955848272,17.7414349694248));
#14505=CARTESIAN_POINT('Ctrl Pts',(7.06017777595217,2.95002493912375,17.7355819480967));
#14506=CARTESIAN_POINT('Ctrl Pts',(6.97097897915068,3.02419065188116,17.7297289267685));
#14507=CARTESIAN_POINT('Ctrl Pts',(6.88175043282775,3.09838110033613,17.7238739533447));
#14508=CARTESIAN_POINT('Ctrl Pts',(6.78927198745366,3.1685889776424,17.7180189799208));
#14509=CARTESIAN_POINT('Ctrl Pts',(6.69394212490612,3.23453296329529,17.712164006497));
#14510=CARTESIAN_POINT('Ctrl Pts',(6.59850421820409,3.3005516879857,17.7063023972128));
#14511=CARTESIAN_POINT('Ctrl Pts',(6.50020878398385,3.36229664032851,17.7004407879287));
#14512=CARTESIAN_POINT('Ctrl Pts',(6.39948218503442,3.41953054900074,17.6945791786445));
#14513=CARTESIAN_POINT('Ctrl Pts',(6.29868766539961,3.4768030509179,17.6887136168342));
#14514=CARTESIAN_POINT('Ctrl Pts',(6.19545908369862,3.52955826466197,17.6828480550239));
#14515=CARTESIAN_POINT('Ctrl Pts',(6.09024465169915,3.57760624817609,17.6769824932135));
#14516=CARTESIAN_POINT('Ctrl Pts',(5.98487637039453,3.62572448962667,17.6711083545132));
#14517=CARTESIAN_POINT('Ctrl Pts',(5.87751682509897,3.66912160962375,17.6652342158128));
#14518=CARTESIAN_POINT('Ctrl Pts',(5.76863137102735,3.7076568329352,17.6593600771125));
#14519=CARTESIAN_POINT('Ctrl Pts',(5.74109601726098,3.71740176181844,17.6578746033312));
#14520=CARTESIAN_POINT('Ctrl Pts',(5.71346314002777,3.72683602521232,17.6563891295499));
#14521=CARTESIAN_POINT('Ctrl Pts',(5.68574037104254,3.73595786345046,17.6549036557687));
#14522=CARTESIAN_POINT('Ctrl Pts',(5.57612218988211,3.77202638593598,17.6490299663781));
#14523=CARTESIAN_POINT('Ctrl Pts',(5.46473264421296,3.80332636779926,17.6431562769875));
#14524=CARTESIAN_POINT('Ctrl Pts',(5.35202433030282,3.82968273367584,17.637282587597));
#14525=CARTESIAN_POINT('Ctrl Pts',(5.23946153341441,3.85600507100801,17.6314164816912));
#14526=CARTESIAN_POINT('Ctrl Pts',(5.12558375292259,3.87739639218158,17.6255503757855));
#14527=CARTESIAN_POINT('Ctrl Pts',(5.01086068620922,3.89373072721203,17.6196842698797));
#14528=CARTESIAN_POINT('Ctrl Pts',(4.89625509445457,3.91004833609151,17.6138241707917));
#14529=CARTESIAN_POINT('Ctrl Pts',(4.78080634474241,3.92131920098427,17.6079640717036));
#14530=CARTESIAN_POINT('Ctrl Pts',(4.664995674457,3.92746809921336,17.6021039726156));
#14531=CARTESIAN_POINT('Ctrl Pts',(4.54500681939418,3.93383883566267,17.5960324545215));
#14532=CARTESIAN_POINT('Ctrl Pts',(4.42462987597543,3.93471094705703,17.5899609364274));
#14533=CARTESIAN_POINT('Ctrl Pts',(4.30440784814854,3.93005933464042,17.5838894183333));
#14534=CARTESIAN_POINT('Ctrl Pts',(4.18850549386054,3.92557485837541,17.5780360547365));
#14535=CARTESIAN_POINT('Ctrl Pts',(4.07274756249806,3.91595678793296,17.5721826911398));
#14536=CARTESIAN_POINT('Ctrl Pts',(3.95762121081433,3.90123567312347,17.566329327543));
#14537=CARTESIAN_POINT('Ctrl Pts',(3.8425121449649,3.88651676863982,17.5604768428091));
#14538=CARTESIAN_POINT('Ctrl Pts',(3.72803487993564,3.86669639568011,17.5546243580753));
#14539=CARTESIAN_POINT('Ctrl Pts',(3.61467069760924,3.84185689989403,17.5487718733414));
#14540=CARTESIAN_POINT('Ctrl Pts',(3.50129612130937,3.81701512665969,17.5429188520132));
#14541=CARTESIAN_POINT('Ctrl Pts',(3.38903523418058,3.78715340422412,17.537065830685));
#14542=CARTESIAN_POINT('Ctrl Pts',(3.27835768764028,3.75240489358708,17.5312128093568));
#14543=CARTESIAN_POINT('Ctrl Pts',(3.16764322800079,3.71764479365066,17.525357835933));
#14544=CARTESIAN_POINT('Ctrl Pts',(3.05851355296416,3.67799478834095,17.5195028625092));
#14545=CARTESIAN_POINT('Ctrl Pts',(2.95142107917391,3.63363721858553,17.5136478890854));
#14546=CARTESIAN_POINT('Ctrl Pts',(2.84420722982018,3.58922937522232,17.5077862798012));
#14547=CARTESIAN_POINT('Ctrl Pts',(2.73903557206171,3.54010347642444,17.5019246705171));
#14548=CARTESIAN_POINT('Ctrl Pts',(2.63633662217621,3.48648917114839,17.4960630612329));
#14549=CARTESIAN_POINT('Ctrl Pts',(2.53356842163459,3.43283871335255,17.4901974994226));
#14550=CARTESIAN_POINT('Ctrl Pts',(2.43327660559645,3.37469402921931,17.4843319376123));
#14551=CARTESIAN_POINT('Ctrl Pts',(2.33586376372488,3.31232878521873,17.4784663758019));
#14552=CARTESIAN_POINT('Ctrl Pts',(2.2383084803864,3.24987234793533,17.4725922371016));
#14553=CARTESIAN_POINT('Ctrl Pts',(2.14364090930449,3.18318327105191,17.4667180984013));
#14554=CARTESIAN_POINT('Ctrl Pts',(2.05223161849938,3.11257628061503,17.4608439597009));
#14555=CARTESIAN_POINT('Ctrl Pts',(2.02911570112263,3.09472092540131,17.4593584859197));
#14556=CARTESIAN_POINT('Ctrl Pts',(2.00620796999553,3.07661520573659,17.4578730121384));
#14557=CARTESIAN_POINT('Ctrl Pts',(1.98351404100473,3.05826458067885,17.4563875383571));
#14558=CARTESIAN_POINT('Ctrl Pts',(1.89378031993646,2.98570465194078,17.4505138489665));
#14559=CARTESIAN_POINT('Ctrl Pts',(1.80709336742514,2.90907116048081,17.444640159576));
#14560=CARTESIAN_POINT('Ctrl Pts',(1.72384565741476,2.82864951647413,17.4387664701854));
#14561=CARTESIAN_POINT('Ctrl Pts',(1.64070542801886,2.74833170436522,17.4329003642796));
#14562=CARTESIAN_POINT('Ctrl Pts',(1.56099590507748,2.6642357504569,17.4270342583739));
#14563=CARTESIAN_POINT('Ctrl Pts',(1.48507756957515,2.57668805561826,17.4211681524681));
#14564=CARTESIAN_POINT('Ctrl Pts',(1.40923697348118,2.48923000850377,17.4153080533801));
#14565=CARTESIAN_POINT('Ctrl Pts',(1.33718011201403,2.39832756122633,17.409447954292));
#14566=CARTESIAN_POINT('Ctrl Pts',(1.2692310787425,2.30434432240768,17.403587855204));
#14567=CARTESIAN_POINT('Ctrl Pts',(1.1988305993671,2.20697038274255,17.3975163371099));
#14568=CARTESIAN_POINT('Ctrl Pts',(1.13284027138534,2.10628947244678,17.3914448190158));
#14569=CARTESIAN_POINT('Ctrl Pts',(1.0715755530835,2.00274427572439,17.3853733009217));
#14570=CARTESIAN_POINT('Ctrl Pts',(1.01251212507178,1.90291954067149,17.3795199373249));
#14571=CARTESIAN_POINT('Ctrl Pts',(0.957840789573258,1.80043319510697,17.3736665737282));
#14572=CARTESIAN_POINT('Ctrl Pts',(0.90779996765182,1.69571116201616,17.3678132101314));
#14573=CARTESIAN_POINT('Ctrl Pts',(0.857766659191405,1.59100485258623,17.3619607253975));
#14574=CARTESIAN_POINT('Ctrl Pts',(0.812362659957376,1.48406389576237,17.3561082406636));
#14575=CARTESIAN_POINT('Ctrl Pts',(0.771779681740187,1.37533735684723,17.3502557559297));
#14576=CARTESIAN_POINT('Ctrl Pts',(0.731192982608776,1.26660084916827,17.3444027346015));
#14577=CARTESIAN_POINT('Ctrl Pts',(0.695428327675673,1.15607882103234,17.3385497132734));
#14578=CARTESIAN_POINT('Ctrl Pts',(0.664628423208093,1.04423811205542,17.3326966919452));
#14579=CARTESIAN_POINT('Ctrl Pts',(0.63381824637756,0.932360102042171,17.3268417185214));
#14580=CARTESIAN_POINT('Ctrl Pts',(0.607976222210408,0.819162934756042,
17.3209867450975));
#14581=CARTESIAN_POINT('Ctrl Pts',(0.587194387559713,0.705125628203866,
17.3151317716737));
#14582=CARTESIAN_POINT('Ctrl Pts',(0.566388999368772,0.590959075012283,
17.3092701623895));
#14583=CARTESIAN_POINT('Ctrl Pts',(0.550655321670228,0.475950888719086,
17.3034085531054));
#14584=CARTESIAN_POINT('Ctrl Pts',(0.540033765612626,0.36058733041429,17.2975469438212));
#14585=CARTESIAN_POINT('Ctrl Pts',(0.529405047361767,0.245145981614885,
17.2916813820109));
#14586=CARTESIAN_POINT('Ctrl Pts',(0.523895334361594,0.129349195304322,
17.2858158202005));
#14587=CARTESIAN_POINT('Ctrl Pts',(0.523492910215201,0.013683627931959,
17.2799502583902));
#14588=CARTESIAN_POINT('Ctrl Pts',(0.523089897626005,-0.102151070868716,
17.2740761196899));
#14589=CARTESIAN_POINT('Ctrl Pts',(0.527809061586433,-0.217853756583575,
17.2682019809895));
#14590=CARTESIAN_POINT('Ctrl Pts',(0.53758682377809,-0.332942422014075,
17.2623278422892));
#14591=CARTESIAN_POINT('Ctrl Pts',(0.540059460213178,-0.362046466664684,
17.2608423685079));
#14592=CARTESIAN_POINT('Ctrl Pts',(0.542855339607083,-0.391111295726141,
17.2593568947267));
#14593=CARTESIAN_POINT('Ctrl Pts',(0.545972919096128,-0.420129230717572,
17.2578714209454));
#14594=CARTESIAN_POINT('Ctrl Pts',(0.55830009295806,-0.534868608177082,
17.2519977315548));
#14595=CARTESIAN_POINT('Ctrl Pts',(0.57570199575384,-0.64925607920481,17.2461240421643));
#14596=CARTESIAN_POINT('Ctrl Pts',(0.598151558931453,-0.762807121295276,
17.2402503527737));
#14597=CARTESIAN_POINT('Ctrl Pts',(0.620572137613951,-0.876211558322706,
17.2343842468679));
#14598=CARTESIAN_POINT('Ctrl Pts',(0.648027337096813,-0.988781312398336,
17.2285181409622));
#14599=CARTESIAN_POINT('Ctrl Pts',(0.680438300338676,-1.10003652350658,
17.2226520350564));
#14600=CARTESIAN_POINT('Ctrl Pts',(0.712816075167087,-1.21117781069601,
17.2167919359684));
#14601=CARTESIAN_POINT('Ctrl Pts',(0.750139405009676,-1.32100683807485,
17.2109318368804));
#14602=CARTESIAN_POINT('Ctrl Pts',(0.792278440894378,-1.42905415158187,
17.2050717377923));
#14603=CARTESIAN_POINT('Ctrl Pts',(0.835937757059272,-1.54099956566485,
17.1990002196982));
#14604=CARTESIAN_POINT('Ctrl Pts',(0.884766731611055,-1.65103183515588,
17.1929287016041));
#14605=CARTESIAN_POINT('Ctrl Pts',(0.938564386476564,-1.75864589466417,
17.18685718351));
#14606=CARTESIAN_POINT('Ctrl Pts',(0.990429048608736,-1.86239329501131,
17.1810038199133));
#14607=CARTESIAN_POINT('Ctrl Pts',(1.04691127806465,-1.96389286992691,17.1751504563165));
#14608=CARTESIAN_POINT('Ctrl Pts',(1.1077824187438,-2.06271337541874,17.1692970927198));
#14609=CARTESIAN_POINT('Ctrl Pts',(1.16864441982601,-2.16151904334421,17.1634446079859));
#14610=CARTESIAN_POINT('Ctrl Pts',(1.23389380521009,-2.2576460900056,17.157592123252));
#14611=CARTESIAN_POINT('Ctrl Pts',(1.30325715058331,-2.35068997590938,17.1517396385181));
#14612=CARTESIAN_POINT('Ctrl Pts',(1.372626855644,-2.44374239268825,17.1458866171899));
#14613=CARTESIAN_POINT('Ctrl Pts',(1.44611102357843,-2.53371075550955,17.1400335958617));
#14614=CARTESIAN_POINT('Ctrl Pts',(1.52339472781864,-2.62022206898113,17.1341805745336));
#14615=CARTESIAN_POINT('Ctrl Pts',(1.60070420766672,-2.70676223564645,17.1283256011097));
#14616=CARTESIAN_POINT('Ctrl Pts',(1.68181546853385,-2.78984275234677,17.1224706276859));
#14617=CARTESIAN_POINT('Ctrl Pts',(1.76637588188335,-2.86912659957476,17.1166156542621));
#14618=CARTESIAN_POINT('Ctrl Pts',(1.85103213360002,-2.94850030485997,17.110754044978));
#14619=CARTESIAN_POINT('Ctrl Pts',(1.93914503871145,-3.02406846932883,17.1048924356938));
#14620=CARTESIAN_POINT('Ctrl Pts',(2.03032789547589,-3.09553352841438,17.0990308264096));
#14621=CARTESIAN_POINT('Ctrl Pts',(2.12157223751029,-3.1670467769141,17.0931652645993));
#14622=CARTESIAN_POINT('Ctrl Pts',(2.2158903179078,-3.23445117118716,17.087299702789));
#14623=CARTESIAN_POINT('Ctrl Pts',(2.31286684386495,-3.29749273552403,17.0814341409786));
#14624=CARTESIAN_POINT('Ctrl Pts',(2.40998517328808,-3.36062648208991,17.0755600022783));
#14625=CARTESIAN_POINT('Ctrl Pts',(2.50976935170389,-3.41938445795698,17.069685863578));
#14626=CARTESIAN_POINT('Ctrl Pts',(2.61177987826993,-3.47355878779839,17.0638117248776));
#14627=CARTESIAN_POINT('Ctrl Pts',(2.63757667510419,-3.48725859141274,17.0623262510964));
#14628=CARTESIAN_POINT('Ctrl Pts',(2.6635157518535,-3.50066551228837,17.0608407773151));
#14629=CARTESIAN_POINT('Ctrl Pts',(2.68958981982905,-3.51377668432824,17.0593553035338));
#14630=CARTESIAN_POINT('Ctrl Pts',(2.79268889728607,-3.56561937120618,17.0534816141432));
#14631=CARTESIAN_POINT('Ctrl Pts',(2.89824332382782,-3.61300695171493,17.0476079247527));
#14632=CARTESIAN_POINT('Ctrl Pts',(3.00583127727128,-3.65569950751262,17.0417342353621));
#14633=CARTESIAN_POINT('Ctrl Pts',(3.11328032455943,-3.69833694320999,17.0358681294563));
#14634=CARTESIAN_POINT('Ctrl Pts',(3.22275729703346,-3.73629125797427,17.0300020235506));
#14635=CARTESIAN_POINT('Ctrl Pts',(3.33381621540456,-3.76936857931771,17.0241359176448));
#14636=CARTESIAN_POINT('Ctrl Pts',(3.44476141085816,-3.80241202990551,17.0182758185568));
#14637=CARTESIAN_POINT('Ctrl Pts',(3.55728493650575,-3.83058830328186,17.0124157194687));
#14638=CARTESIAN_POINT('Ctrl Pts',(3.67092191405302,-3.85375201704537,17.0065556203807));
#14639=CARTESIAN_POINT('Ctrl Pts',(3.78865865450265,-3.87775142475656,17.0004841022866));
#14640=CARTESIAN_POINT('Ctrl Pts',(3.90759028551902,-3.89636959407866,16.9944125841925));
#14641=CARTESIAN_POINT('Ctrl Pts',(4.02718344456594,-3.90950160771162,16.9883410660984));
#14642=CARTESIAN_POINT('Ctrl Pts',(4.14247952583186,-3.9221617775999,16.9824877025016));
#14643=CARTESIAN_POINT('Ctrl Pts',(4.25838996891244,-3.92972320188552,16.9766343389049));
#14644=CARTESIAN_POINT('Ctrl Pts',(4.3744284394501,-3.9321442406143,16.9707809753081));
#14645=CARTESIAN_POINT('Ctrl Pts',(4.49044948720186,-3.93456491583226,16.9649284905742));
#14646=CARTESIAN_POINT('Ctrl Pts',(4.60659811124423,-3.93184673152901,16.9590760058403));
#14647=CARTESIAN_POINT('Ctrl Pts',(4.7223861479458,-3.92400014359312,16.9532235211064));
#14648=CARTESIAN_POINT('Ctrl Pts',(4.83818480085579,-3.91615283623047,16.9473704997782));
#14649=CARTESIAN_POINT('Ctrl Pts',(4.95362238848057,-3.90317621844511,16.94151747845));
#14650=CARTESIAN_POINT('Ctrl Pts',(5.06821475517741,-3.88513272115375,16.9356644571219));
#14651=CARTESIAN_POINT('Ctrl Pts',(5.1828453406414,-3.8670832060076,16.929809483698));
#14652=CARTESIAN_POINT('Ctrl Pts',(5.29662973674041,-3.84396351528701,16.9239545102742));
#14653=CARTESIAN_POINT('Ctrl Pts',(5.40909358005421,-3.81588726403817,16.9180995368504));
#14654=CARTESIAN_POINT('Ctrl Pts',(5.52168488668901,-3.78777919196479,16.9122379275662));
#14655=CARTESIAN_POINT('Ctrl Pts',(5.63295225219454,-3.75470344704765,16.9063763182821));
#14656=CARTESIAN_POINT('Ctrl Pts',(5.74243599603799,-3.71682366521299,16.9005147089979));
#14657=CARTESIAN_POINT('Ctrl Pts',(5.85199356557387,-3.67891834076328,16.8946491471876));
#14658=CARTESIAN_POINT('Ctrl Pts',(5.95976473546107,-3.63620268089117,16.8887835853773));
#14659=CARTESIAN_POINT('Ctrl Pts',(6.06531095373924,-3.58888797675063,16.8829180235669));
#14660=CARTESIAN_POINT('Ctrl Pts',(6.17101150647557,-3.54150408690788,16.8770438848666));
#14661=CARTESIAN_POINT('Ctrl Pts',(6.27448024684995,-3.48950791632331,16.8711697461663));
#14662=CARTESIAN_POINT('Ctrl Pts',(6.37530423800722,-3.43315608981188,16.8652956074659));
#14663=CARTESIAN_POINT('Ctrl Pts',(6.40080097940688,-3.41890563283761,16.8638101336846));
#14664=CARTESIAN_POINT('Ctrl Pts',(6.42612874043806,-3.40437684241596,16.8623246599034));
#14665=CARTESIAN_POINT('Ctrl Pts',(6.4512811614294,-3.38957428955087,16.8608391861221));
#14666=CARTESIAN_POINT('Ctrl Pts',(6.55073596849879,-3.3310437393569,16.8549654967315));
#14667=CARTESIAN_POINT('Ctrl Pts',(6.64777818281768,-3.26803478452412,16.849091807341));
#14668=CARTESIAN_POINT('Ctrl Pts',(6.74197752530337,-3.20077182352804,16.8432181179504));
#14669=CARTESIAN_POINT('Ctrl Pts',(6.8360552475882,-3.13359570533373,16.8373520120446));
#14670=CARTESIAN_POINT('Ctrl Pts',(6.92729706413442,-3.06217674129316,16.8314859061389));
#14671=CARTESIAN_POINT('Ctrl Pts',(7.01529829275506,-2.98678459118286,16.8256198002331));
#14672=CARTESIAN_POINT('Ctrl Pts',(7.10320940923867,-2.91146964167383,16.8197597011451));
#14673=CARTESIAN_POINT('Ctrl Pts',(7.18788622632745,-2.83218986585923,16.8138996020571));
#14674=CARTESIAN_POINT('Ctrl Pts',(7.26895456310386,-2.74925709143524,16.808039502969));
#14675=CARTESIAN_POINT('Ctrl Pts',(7.35294766052476,-2.66333229170989,16.8019679848749));
#14676=CARTESIAN_POINT('Ctrl Pts',(7.43306662264047,-2.57348619555301,16.7958964667808));
#14677=CARTESIAN_POINT('Ctrl Pts',(7.50893414571678,-2.48011011502297,16.7898249486867));
#14678=CARTESIAN_POINT('Ctrl Pts',(7.58207568805712,-2.3900891116907,16.78397158509));
#14679=CARTESIAN_POINT('Ctrl Pts',(7.65126576583956,-2.29678777681912,16.7781182214932));
#14680=CARTESIAN_POINT('Ctrl Pts',(7.71620574220309,-2.20059220757009,16.7722648578965));
#14681=CARTESIAN_POINT('Ctrl Pts',(7.78113596804769,-2.10441108176208,16.7664123731626));
#14682=CARTESIAN_POINT('Ctrl Pts',(7.84181713023146,-2.00533692797378,16.7605598884287));
#14683=CARTESIAN_POINT('Ctrl Pts',(7.89799337677209,-1.903785622172,16.7547074036948));
#14684=CARTESIAN_POINT('Ctrl Pts',(7.95417477392029,-1.80222500547895,16.7488543823666));
#14685=CARTESIAN_POINT('Ctrl Pts',(8.00585023434433,-1.69818714681336,16.7430013610384));
#14686=CARTESIAN_POINT('Ctrl Pts',(8.0528097538547,-1.59211273035481,16.7371483397103));
#14687=CARTESIAN_POINT('Ctrl Pts',(8.09978493527166,-1.48600293602997,16.7312933662864));
#14688=CARTESIAN_POINT('Ctrl Pts',(8.14204088106384,-1.37785561086735,16.7254383928626));
#14689=CARTESIAN_POINT('Ctrl Pts',(8.17941590592433,-1.26813095796855,16.7195834194388));
#14690=CARTESIAN_POINT('Ctrl Pts',(8.21683329057491,-1.15828194626918,16.7137218101547));
#14691=CARTESIAN_POINT('Ctrl Pts',(8.24935857967433,-1.04685242999379,16.7078602008705));
#14692=CARTESIAN_POINT('Ctrl Pts',(8.27688008058664,-0.934317390893255,
16.7019985915864));
#14693=CARTESIAN_POINT('Ctrl Pts',(8.30442013944912,-0.82170646858944,16.696133029776));
#14694=CARTESIAN_POINT('Ctrl Pts',(8.32694961146846,-0.707988943345037,
16.6902674679657));
#14695=CARTESIAN_POINT('Ctrl Pts',(8.34440830307059,-0.59364787675788,16.6844019061553));
#14696=CARTESIAN_POINT('Ctrl Pts',(8.36189252356189,-0.479139615487285,
16.678527767455));
#14697=CARTESIAN_POINT('Ctrl Pts',(8.37429112164412,-0.364006402400336,
16.6726536287547));
#14698=CARTESIAN_POINT('Ctrl Pts',(8.38159588416645,-0.248734350329785,
16.6667794900543));
#14699=CARTESIAN_POINT('Ctrl Pts',(8.38344313935722,-0.219583930191288,
16.665294016273));
#14700=CARTESIAN_POINT('Ctrl Pts',(8.38496490290308,-0.190424618373388,
16.6638085424917));
#14701=CARTESIAN_POINT('Ctrl Pts',(8.38616156821618,-0.161264236942553,
16.6623230687105));
#14702=CARTESIAN_POINT('Ctrl Pts',(8.38835261922407,-0.107872630763612,
16.6596032198186));
#14703=CARTESIAN_POINT('Ctrl Pts',(8.38945560312462,-0.0544360677886508,
16.6568833709268));
#14704=CARTESIAN_POINT('Ctrl Pts',(8.38946898299941,-0.000984499569211592,
16.654163522035));
#14705=CARTESIAN_POINT('',(8.38330870139309,-0.00111159115176508,19.154163522035));
#14706=CARTESIAN_POINT('Ctrl Pts',(8.38330870139309,-0.00111159115176508,
19.154163522035));
#14707=CARTESIAN_POINT('Ctrl Pts',(8.38147360828864,0.724094734411765,19.1176145072401));
#14708=CARTESIAN_POINT('Ctrl Pts',(7.84121757765765,2.76483039537692,19.0148934533079));
#14709=CARTESIAN_POINT('Ctrl Pts',(4.55780727041761,4.64794687683432,18.8460003602387));
#14710=CARTESIAN_POINT('Ctrl Pts',(0.605699254871401,2.60485146316644,18.6474842428269));
#14711=CARTESIAN_POINT('Ctrl Pts',(0.180053019792298,-1.82371737090629,
18.4489681254154));
#14712=CARTESIAN_POINT('Ctrl Pts',(3.67066729059547,-4.58216052750365,18.2504520080036));
#14713=CARTESIAN_POINT('Ctrl Pts',(7.52217034079766,-3.26685715566783,18.0688504735435));
#14714=CARTESIAN_POINT('Ctrl Pts',(8.37983385625592,-0.97047922611876,17.9534209782207));
#14715=CARTESIAN_POINT('Ctrl Pts',(8.38858227448227,0.00358766171095831,
17.904163522035));
#14716=CARTESIAN_POINT('',(8.39024757142292,-0.00302155333681673,20.4041631666841));
#14717=CARTESIAN_POINT('Ctrl Pts',(8.39265998963715,-0.00300172473988639,
20.404162067119));
#14718=CARTESIAN_POINT('Ctrl Pts',(8.38321720628087,1.10505925672828,20.3479791054527));
#14719=CARTESIAN_POINT('Ctrl Pts',(7.31619850019849,3.53408620393106,20.2256241046493));
#14720=CARTESIAN_POINT('Ctrl Pts',(3.19725112513313,4.47527090540738,20.0370970647086));
#14721=CARTESIAN_POINT('Ctrl Pts',(0.013229802472921,1.36795617003671,19.838580947297));
#14722=CARTESIAN_POINT('Ctrl Pts',(0.898242515440645,-2.99210680286265,
19.6400648298852));
#14723=CARTESIAN_POINT('Ctrl Pts',(5.04181145526696,-4.6120552824946,19.4415487124736));
#14724=CARTESIAN_POINT('Ctrl Pts',(7.98514998524053,-2.48773831511406,19.2795816098569));
#14725=CARTESIAN_POINT('Ctrl Pts',(8.38479604675681,-0.588892267483202,
19.1837865463773));
#14726=CARTESIAN_POINT('Ctrl Pts',(8.38330870139309,-0.00111159115176508,
19.154163522035));
#14727=CARTESIAN_POINT('',(8.39034187497082,0.00295420694097821,21.6541639142457));
#14728=CARTESIAN_POINT('Ctrl Pts',(8.38946799139497,0.0029612832834954,
21.654163522035));
#14729=CARTESIAN_POINT('Ctrl Pts',(8.38932489603607,0.193011958324324,21.6445176826906));
#14730=CARTESIAN_POINT('Ctrl Pts',(8.37540471230823,0.382553267708013,21.6348718433462));
#14731=CARTESIAN_POINT('Ctrl Pts',(8.34793638037932,0.570062675618605,21.6252260040018));
#14732=CARTESIAN_POINT('Ctrl Pts',(8.33120994712477,0.684243747994348,21.6193523132224));
#14733=CARTESIAN_POINT('Ctrl Pts',(8.30942604979843,0.797878198448378,21.6134786224429));
#14734=CARTESIAN_POINT('Ctrl Pts',(8.28263035283746,0.91048290201921,21.6076049316635));
#14735=CARTESIAN_POINT('Ctrl Pts',(8.25586925156278,1.02294222265772,21.601738824354));
#14736=CARTESIAN_POINT('Ctrl Pts',(8.22410931350316,1.13437404209587,21.5958727170445));
#14737=CARTESIAN_POINT('Ctrl Pts',(8.18744777420902,1.24430188418961,21.5900066097351));
#14738=CARTESIAN_POINT('Ctrl Pts',(8.15082377577351,1.35411716184502,21.5841465092303));
#14739=CARTESIAN_POINT('Ctrl Pts',(8.10930828957067,1.46243113584916,21.5782864087255));
#14740=CARTESIAN_POINT('Ctrl Pts',(8.06304910562404,1.56877968749157,21.5724263082207));
#14741=CARTESIAN_POINT('Ctrl Pts',(8.01512101159534,1.67896501607009,21.5663547906528));
#14742=CARTESIAN_POINT('Ctrl Pts',(7.96210058167485,1.78703999080972,21.5602832730848));
#14743=CARTESIAN_POINT('Ctrl Pts',(7.90420805046819,1.89250764127977,21.5542117555169));
#14744=CARTESIAN_POINT('Ctrl Pts',(7.84839562560396,1.99418578861201,21.5483583904798));
#14745=CARTESIAN_POINT('Ctrl Pts',(7.78805540381289,2.09344035878736,21.5425050254427));
#14746=CARTESIAN_POINT('Ctrl Pts',(7.7234324412104,2.18984921120542,21.5366516604057));
#14747=CARTESIAN_POINT('Ctrl Pts',(7.65881918145674,2.28624358826544,21.5307991742252));
#14748=CARTESIAN_POINT('Ctrl Pts',(7.58992468945802,2.3797927540567,21.5249466880447));
#14749=CARTESIAN_POINT('Ctrl Pts',(7.5170377304785,2.47010297279157,21.5190942018642));
#14750=CARTESIAN_POINT('Ctrl Pts',(7.44414408868623,2.56042147183186,21.5132411790847));
#14751=CARTESIAN_POINT('Ctrl Pts',(7.36725751171053,2.64750011194895,21.5073881563052));
#14752=CARTESIAN_POINT('Ctrl Pts',(7.28670702447934,2.73097827271423,21.5015351335258));
#14753=CARTESIAN_POINT('Ctrl Pts',(7.20612967206777,2.8144842750969,21.4956801586474));
#14754=CARTESIAN_POINT('Ctrl Pts',(7.12188626625766,2.8943871131849,21.4898251837691));
#14755=CARTESIAN_POINT('Ctrl Pts',(7.03434212388975,2.97036356440778,21.4839702088908));
#14756=CARTESIAN_POINT('Ctrl Pts',(6.9466987615445,3.04642612512427,21.4781085981547));
#14757=CARTESIAN_POINT('Ctrl Pts',(6.85574750811192,3.11855314599317,21.4722469874187));
#14758=CARTESIAN_POINT('Ctrl Pts',(6.76188621259502,3.18646213936795,21.4663853766826));
#14759=CARTESIAN_POINT('Ctrl Pts',(6.66796162572878,3.25441692426735,21.4605198134201));
#14760=CARTESIAN_POINT('Ctrl Pts',(6.57112343373736,3.31814779158435,21.4546542501576));
#14761=CARTESIAN_POINT('Ctrl Pts',(6.47179638086606,3.37741690883146,21.4487886868951));
#14762=CARTESIAN_POINT('Ctrl Pts',(6.37232408770054,3.43677269193423,21.4429145467534));
#14763=CARTESIAN_POINT('Ctrl Pts',(6.27035603288893,3.4916535093278,21.4370404066117));
#14764=CARTESIAN_POINT('Ctrl Pts',(6.16633937963864,3.5418685249559,21.43116626647));
#14765=CARTESIAN_POINT('Ctrl Pts',(6.14003551731337,3.5545669613742,21.4296808065101));
#14766=CARTESIAN_POINT('Ctrl Pts',(6.11360073532189,3.56696727036229,21.4281953465501));
#14767=CARTESIAN_POINT('Ctrl Pts',(6.08704242687941,3.57906686804649,21.4267098865902));
#14768=CARTESIAN_POINT('Ctrl Pts',(5.98202764443305,3.62691014922707,21.4208361971999));
#14769=CARTESIAN_POINT('Ctrl Pts',(5.87473049369302,3.67020727738114,21.4149625078096));
#14770=CARTESIAN_POINT('Ctrl Pts',(5.76558170321074,3.70873471798612,21.4090888184194));
#14771=CARTESIAN_POINT('Ctrl Pts',(5.65657383400523,3.74721241606903,21.4032227125103));
#14772=CARTESIAN_POINT('Ctrl Pts',(5.54571946528469,3.78093253680742,21.3973566066013));
#14773=CARTESIAN_POINT('Ctrl Pts',(5.43347169575851,3.80971848566684,21.3914905006923));
#14774=CARTESIAN_POINT('Ctrl Pts',(5.32133886645076,3.83847495809868,21.3856304015974));
#14775=CARTESIAN_POINT('Ctrl Pts',(5.2078158722244,3.86230720652487,21.3797703025026));
#14776=CARTESIAN_POINT('Ctrl Pts',(5.09337283381983,3.88108781680694,21.3739102034077));
#14777=CARTESIAN_POINT('Ctrl Pts',(4.97480095183767,3.90054598863602,21.3678386853149));
#14778=CARTESIAN_POINT('Ctrl Pts',(4.85524181200714,3.91458098684631,21.361767167222));
#14779=CARTESIAN_POINT('Ctrl Pts',(4.73523241404701,3.92310846373235,21.3556956491291));
#14780=CARTESIAN_POINT('Ctrl Pts',(4.61953504933254,3.93132954158249,21.3498422855167));
#14781=CARTESIAN_POINT('Ctrl Pts',(4.50341967334397,3.93443203427796,21.3439889219043));
#14782=CARTESIAN_POINT('Ctrl Pts',(4.38737386119142,3.93239301788551,21.338135558292));
#14783=CARTESIAN_POINT('Ctrl Pts',(4.27134547286255,3.93035430764338,21.3322830735392));
#14784=CARTESIAN_POINT('Ctrl Pts',(4.15538704057191,3.92317563055062,21.3264305887864));
#14785=CARTESIAN_POINT('Ctrl Pts',(4.03998596579679,3.91088619033394,21.3205781040336));
#14786=CARTESIAN_POINT('Ctrl Pts',(3.92457431022854,3.89859562333378,21.3147250826833));
#14787=CARTESIAN_POINT('Ctrl Pts',(3.80972052460738,3.88119340544641,21.308872061333));
#14788=CARTESIAN_POINT('Ctrl Pts',(3.69590600846696,3.85876052306165,21.3030190399827));
#14789=CARTESIAN_POINT('Ctrl Pts',(3.58205353292439,3.83632015886496,21.2971640665335));
#14790=CARTESIAN_POINT('Ctrl Pts',(3.46924142122266,3.80884587373843,21.2913090930843));
#14791=CARTESIAN_POINT('Ctrl Pts',(3.35793932137559,3.77646942418624,21.2854541196351));
#14792=CARTESIAN_POINT('Ctrl Pts',(3.24651107480554,3.74405628006119,21.2795925103209));
#14793=CARTESIAN_POINT('Ctrl Pts',(3.13659665287681,3.70672999757413,21.2737309010066));
#14794=CARTESIAN_POINT('Ctrl Pts',(3.02864910972258,3.66467175305062,21.2678692916924));
#14795=CARTESIAN_POINT('Ctrl Pts',(2.92062877669618,3.62258514832407,21.2620037298492));
#14796=CARTESIAN_POINT('Ctrl Pts',(2.81457834037405,3.57576039443417,21.2561381680059));
#14797=CARTESIAN_POINT('Ctrl Pts',(2.71092791097229,3.52442547597468,21.2502726061627));
#14798=CARTESIAN_POINT('Ctrl Pts',(2.60712591915362,3.47301549324041,21.2443984674257));
#14799=CARTESIAN_POINT('Ctrl Pts',(2.50573129849915,3.4170823828248,21.2385243286886));
#14800=CARTESIAN_POINT('Ctrl Pts',(2.40714682128416,3.35689844536181,21.2326501899515));
#14801=CARTESIAN_POINT('Ctrl Pts',(2.38221641974906,3.34167891213201,21.2311647163605));
#14802=CARTESIAN_POINT('Ctrl Pts',(2.35746556750933,3.32618774336432,21.2296792427695));
#14803=CARTESIAN_POINT('Ctrl Pts',(2.33290044391734,3.31042975102834,21.2281937691785));
#14804=CARTESIAN_POINT('Ctrl Pts',(2.2357678544058,3.24812130811069,21.2223200801654));
#14805=CARTESIAN_POINT('Ctrl Pts',(2.14121813868295,3.18143046089737,21.2164463911523));
#14806=CARTESIAN_POINT('Ctrl Pts',(2.04967263659629,3.11059797367248,21.2105727021392));
#14807=CARTESIAN_POINT('Ctrl Pts',(1.95824532845483,3.03985693792168,21.204706596617));
#14808=CARTESIAN_POINT('Ctrl Pts',(1.86981484420736,2.96498514660278,21.1988404910948));
#14809=CARTESIAN_POINT('Ctrl Pts',(1.78477520674591,2.88626760843867,21.1929743855726));
#14810=CARTESIAN_POINT('Ctrl Pts',(1.69982264887592,2.80763067611049,21.1871142868736));
#14811=CARTESIAN_POINT('Ctrl Pts',(1.61825433271175,2.72515610892687,21.1812541881747));
#14812=CARTESIAN_POINT('Ctrl Pts',(1.54043218228572,2.63916988052344,21.1753940894757));
#14813=CARTESIAN_POINT('Ctrl Pts',(1.4598023789505,2.55008145714075,21.1693225712378));
#14814=CARTESIAN_POINT('Ctrl Pts',(1.38319450904063,2.45722347877443,21.163251053));
#14815=CARTESIAN_POINT('Ctrl Pts',(1.31097056336446,2.36100146482477,21.1571795347621));
#14816=CARTESIAN_POINT('Ctrl Pts',(1.24134168818897,2.26823679327836,21.1513261715658));
#14817=CARTESIAN_POINT('Ctrl Pts',(1.17578739168021,2.17234603005742,21.1454728083696));
#14818=CARTESIAN_POINT('Ctrl Pts',(1.1145912561187,2.07372646099095,21.1396194451733));
#14819=CARTESIAN_POINT('Ctrl Pts',(1.05340430898868,1.97512169938158,21.1337669608434));
#14820=CARTESIAN_POINT('Ctrl Pts',(0.996574439458465,1.87378929756515,21.1279144765135));
#14821=CARTESIAN_POINT('Ctrl Pts',(0.944341332402823,1.77015465437184,21.1220619921837));
#14822=CARTESIAN_POINT('Ctrl Pts',(0.89210343630009,1.66651050932781,21.1162089712626));
#14823=CARTESIAN_POINT('Ctrl Pts',(0.844463326450425,1.56056407224726,21.1103559503416));
#14824=CARTESIAN_POINT('Ctrl Pts',(0.80161392064252,1.45276377035986,21.1045029294206));
#14825=CARTESIAN_POINT('Ctrl Pts',(0.758750223749061,1.34492751503722,21.0986479564066));
#14826=CARTESIAN_POINT('Ctrl Pts',(0.720680560556225,1.23523654916782,21.0927929833926));
#14827=CARTESIAN_POINT('Ctrl Pts',(0.687548815718343,1.12415694805401,21.0869380103786));
#14828=CARTESIAN_POINT('Ctrl Pts',(0.654379520311777,1.01295145250839,21.0810764015063));
#14829=CARTESIAN_POINT('Ctrl Pts',(0.626159431681027,0.900354576560428,
21.0752147926339));
#14830=CARTESIAN_POINT('Ctrl Pts',(0.602981910917189,0.786845242503738,
21.0693531837616));
#14831=CARTESIAN_POINT('Ctrl Pts',(0.579788761386301,0.673259368296008,
21.0634876223647));
#14832=CARTESIAN_POINT('Ctrl Pts',(0.561645014854082,0.558760217870424,
21.0576220609678));
#14833=CARTESIAN_POINT('Ctrl Pts',(0.54859226094128,0.443832808778391,21.0517564995709));
#14834=CARTESIAN_POINT('Ctrl Pts',(0.535520420697833,0.328737347599823,
21.0458823612833));
#14835=CARTESIAN_POINT('Ctrl Pts',(0.527554458298878,0.213212788560315,
21.0400082229957));
#14836=CARTESIAN_POINT('Ctrl Pts',(0.524683904091009,0.0977452010752936,
21.034134084708));
#14837=CARTESIAN_POINT('Ctrl Pts',(0.523957985853879,0.0685452551822368,
21.032648607061));
#14838=CARTESIAN_POINT('Ctrl Pts',(0.523557662259861,0.0393489297663216,
21.0311631294139));
#14839=CARTESIAN_POINT('Ctrl Pts',(0.523482239653076,0.0101640260651543,
21.0296776517669));
#14840=CARTESIAN_POINT('Ctrl Pts',(0.523184013030639,-0.105235263722956,
21.0238039621628));
#14841=CARTESIAN_POINT('Ctrl Pts',(0.527968556727335,-0.220839887055731,
21.0179302725588));
#14842=CARTESIAN_POINT('Ctrl Pts',(0.53786196686908,-0.336165268047883,
21.0120565829547));
#14843=CARTESIAN_POINT('Ctrl Pts',(0.547742603693473,-0.451341753192286,
21.006190476833));
#14844=CARTESIAN_POINT('Ctrl Pts',(0.562718954643329,-0.566239305094551,
21.0003243707113));
#14845=CARTESIAN_POINT('Ctrl Pts',(0.582765128113554,-0.680372317202752,
20.9944582645896));
#14846=CARTESIAN_POINT('Ctrl Pts',(0.602790774565711,-0.794388458607166,
20.9885981652834));
#14847=CARTESIAN_POINT('Ctrl Pts',(0.627875846305067,-0.90764121293055,
20.9827380659773));
#14848=CARTESIAN_POINT('Ctrl Pts',(0.657942627492596,-1.01964973908694,
20.9768779666711));
#14849=CARTESIAN_POINT('Ctrl Pts',(0.689094147977195,-1.13569927146781,
20.9708064486579));
#14850=CARTESIAN_POINT('Ctrl Pts',(0.725593582909424,-1.25041265292102,
20.9647349306448));
#14851=CARTESIAN_POINT('Ctrl Pts',(0.767296409776802,-1.36326586395718,
20.9586634126316));
#14852=CARTESIAN_POINT('Ctrl Pts',(0.807500822808823,-1.47206417451096,
20.9528100488127));
#14853=CARTESIAN_POINT('Ctrl Pts',(0.852540983897707,-1.57913326801493,
20.9469566849938));
#14854=CARTESIAN_POINT('Ctrl Pts',(0.902236783211508,-1.68401947556852,
20.9411033211749));
#14855=CARTESIAN_POINT('Ctrl Pts',(0.95192512087805,-1.78888993483163,20.9352508362177));
#14856=CARTESIAN_POINT('Ctrl Pts',(1.00626752998871,-1.89157778658281,20.9293983512605));
#14857=CARTESIAN_POINT('Ctrl Pts',(1.06503647993748,-1.99165100893663,20.9235458663033));
#14858=CARTESIAN_POINT('Ctrl Pts',(1.12381081821856,-2.09173340667606,20.9176928447509));
#14859=CARTESIAN_POINT('Ctrl Pts',(1.18701229491361,-2.18920034218853,20.9118398231986));
#14860=CARTESIAN_POINT('Ctrl Pts',(1.25436867559231,-2.2836466084281,20.9059868016462));
#14861=CARTESIAN_POINT('Ctrl Pts',(1.32174752093128,-2.37812437433055,20.9001318279976));
#14862=CARTESIAN_POINT('Ctrl Pts',(1.39328378598043,-2.4695791315016,20.8942768543489));
#14863=CARTESIAN_POINT('Ctrl Pts',(1.46866382516935,-2.55763730863785,20.8884218807003));
#14864=CARTESIAN_POINT('Ctrl Pts',(1.544129297945,-2.64579528840083,20.8825602711915));
#14865=CARTESIAN_POINT('Ctrl Pts',(1.62344697120118,-2.73054869055349,20.8766986616827));
#14866=CARTESIAN_POINT('Ctrl Pts',(1.70626501463763,-2.81155943466489,20.8708370521739));
#14867=CARTESIAN_POINT('Ctrl Pts',(1.78913890288927,-2.89262480491627,20.8649714901387));
#14868=CARTESIAN_POINT('Ctrl Pts',(1.875517554177,-2.96994221701334,20.8591059281036));
#14869=CARTESIAN_POINT('Ctrl Pts',(1.96501595050223,-3.04321379020151,20.8532403660684));
#14870=CARTESIAN_POINT('Ctrl Pts',(2.05464521540632,-3.11659250437821,20.8473662271447));
#14871=CARTESIAN_POINT('Ctrl Pts',(2.14740299994959,-3.18591332641153,20.841492088221));
#14872=CARTESIAN_POINT('Ctrl Pts',(2.24287518041693,-3.2509215511383,20.8356179492974));
#14873=CARTESIAN_POINT('Ctrl Pts',(2.26701850066163,-3.26736104566367,20.83413247765));
#14874=CARTESIAN_POINT('Ctrl Pts',(2.29133528512573,-3.2835249799823,20.8326470060026));
#14875=CARTESIAN_POINT('Ctrl Pts',(2.31581860241582,-3.29940970789782,20.8311615343553));
#14876=CARTESIAN_POINT('Ctrl Pts',(2.41262785544023,-3.36221936011026,20.8252878449828));
#14877=CARTESIAN_POINT('Ctrl Pts',(2.51236506985887,-3.42086923424214,20.8194141556103));
#14878=CARTESIAN_POINT('Ctrl Pts',(2.61463719975846,-3.47507470831156,20.8135404662378));
#14879=CARTESIAN_POINT('Ctrl Pts',(2.71677728673431,-3.52921019802369,20.8076743603498));
#14880=CARTESIAN_POINT('Ctrl Pts',(2.82144541892948,-3.57891250723855,20.8018082544619));
#14881=CARTESIAN_POINT('Ctrl Pts',(2.92821950130668,-3.62394014093605,20.795942148574));
#14882=CARTESIAN_POINT('Ctrl Pts',(3.03488424838858,-3.6689216669123,20.7900820495035));
#14883=CARTESIAN_POINT('Ctrl Pts',(3.14365027784584,-3.709237879147,20.784221950433));
#14884=CARTESIAN_POINT('Ctrl Pts',(3.25407140468637,-3.74469341433325,20.7783618513625));
#14885=CARTESIAN_POINT('Ctrl Pts',(3.36847627434058,-3.78142810449233,20.7722903332617));
#14886=CARTESIAN_POINT('Ctrl Pts',(3.48465752136863,-3.8129445599251,20.7662188151609));
#14887=CARTESIAN_POINT('Ctrl Pts',(3.60209646100962,-3.83908014804578,20.7601472970601));
#14888=CARTESIAN_POINT('Ctrl Pts',(3.71531572524634,-3.8642766634985,20.7542939334801));
#14889=CARTESIAN_POINT('Ctrl Pts',(3.82970341985477,-3.88447223730536,20.7484405699001));
#14890=CARTESIAN_POINT('Ctrl Pts',(3.9447806840801,-3.89957227893647,20.74258720632));
#14891=CARTESIAN_POINT('Ctrl Pts',(4.05984066984796,-3.91467005334798,20.7367347216025));
#14892=CARTESIAN_POINT('Ctrl Pts',(4.17558960983971,-3.92467376310736,20.730882236885));
#14893=CARTESIAN_POINT('Ctrl Pts',(4.29154112620292,-3.92954040078583,20.7250297521675));
#14894=CARTESIAN_POINT('Ctrl Pts',(4.40750327377036,-3.93440748466991,20.7191767308554));
#14895=CARTESIAN_POINT('Ctrl Pts',(4.5236676218275,-3.93413654284151,20.7133237095432));
#14896=CARTESIAN_POINT('Ctrl Pts',(4.63954609087238,-3.92873666942567,20.7074706882311));
#14897=CARTESIAN_POINT('Ctrl Pts',(4.75546320763204,-3.92333499504741,20.701615714823));
#14898=CARTESIAN_POINT('Ctrl Pts',(4.87109384331342,-3.91280100685486,20.6957607414148));
#14899=CARTESIAN_POINT('Ctrl Pts',(4.98595405280371,-3.89719574711604,20.6899057680067));
#14900=CARTESIAN_POINT('Ctrl Pts',(5.10094444160083,-3.88157280081802,20.6840441587375));
#14901=CARTESIAN_POINT('Ctrl Pts',(5.21516225178086,-3.8608671666907,20.6781825494684));
#14902=CARTESIAN_POINT('Ctrl Pts',(5.32813266118402,-3.83519121386984,20.6723209401993));
#14903=CARTESIAN_POINT('Ctrl Pts',(5.44117924737086,-3.80949794756384,20.6664553784037));
#14904=CARTESIAN_POINT('Ctrl Pts',(5.55297636046322,-3.77882779797132,20.660589816608));
#14905=CARTESIAN_POINT('Ctrl Pts',(5.66306496703822,-3.7433428147382,20.6547242548124));
#14906=CARTESIAN_POINT('Ctrl Pts',(5.77331455016921,-3.70780594375239,20.6488501161261));
#14907=CARTESIAN_POINT('Ctrl Pts',(5.88185025514948,-3.66744033158329,20.6429759774399));
#14908=CARTESIAN_POINT('Ctrl Pts',(5.98823355085912,-3.6224558915374,20.6371018387536));
#14909=CARTESIAN_POINT('Ctrl Pts',(6.01513615250219,-3.61108005980913,20.6356163648169));
#14910=CARTESIAN_POINT('Ctrl Pts',(6.04190123492469,-3.59940908001501,20.6341308908803));
#14911=CARTESIAN_POINT('Ctrl Pts',(6.0685219765932,-3.58744680003981,20.6326454169436));
#14912=CARTESIAN_POINT('Ctrl Pts',(6.17378263635646,-3.54014693521476,20.6267717276009));
#14913=CARTESIAN_POINT('Ctrl Pts',(6.27713507773352,-3.48813162624027,20.6208980382581));
#14914=CARTESIAN_POINT('Ctrl Pts',(6.37812705671332,-3.43157685638819,20.6150243489154));
#14915=CARTESIAN_POINT('Ctrl Pts',(6.47898864554543,-3.3750951040655,20.6091582430583));
#14916=CARTESIAN_POINT('Ctrl Pts',(6.57749547543551,-3.31408574623456,20.6032921372012));
#14917=CARTESIAN_POINT('Ctrl Pts',(6.67321579448948,-3.24877255591069,20.5974260313441));
#14918=CARTESIAN_POINT('Ctrl Pts',(6.76883809714315,-3.18352624547055,20.5915659323054));
#14919=CARTESIAN_POINT('Ctrl Pts',(6.86167922527287,-3.11398510004121,20.5857058332668));
#14920=CARTESIAN_POINT('Ctrl Pts',(6.95133313243069,-3.04041814405701,20.5798457342281));
#14921=CARTESIAN_POINT('Ctrl Pts',(7.04422154908736,-2.96419705926262,20.5737742161158));
#14922=CARTESIAN_POINT('Ctrl Pts',(7.13368803324021,-2.88365441590578,20.5677026980034));
#14923=CARTESIAN_POINT('Ctrl Pts',(7.21931473949862,-2.79913790418828,20.5616311798911));
#14924=CARTESIAN_POINT('Ctrl Pts',(7.30186480880349,-2.71765813923469,20.5557778163453));
#14925=CARTESIAN_POINT('Ctrl Pts',(7.38084596487764,-2.63248547505956,20.5499244527995));
#14926=CARTESIAN_POINT('Ctrl Pts',(7.45591912758554,-2.54397102367926,20.5440710892537));
#14927=CARTESIAN_POINT('Ctrl Pts',(7.53098101830435,-2.45546986245346,20.5382186045712));
#14928=CARTESIAN_POINT('Ctrl Pts',(7.6021358152192,-2.36362822670152,20.5323661198888));
#14929=CARTESIAN_POINT('Ctrl Pts',(7.66908370878854,-2.26883150880627,20.5265136352063));
#14930=CARTESIAN_POINT('Ctrl Pts',(7.73603774057587,-2.17402609933181,20.52066061393));
#14931=CARTESIAN_POINT('Ctrl Pts',(7.79878386390566,-2.07626540659848,20.5148075926537));
#14932=CARTESIAN_POINT('Ctrl Pts',(7.8570651281001,-1.97596449764699,20.5089545713774));
#14933=CARTESIAN_POINT('Ctrl Pts',(7.91536583021796,-1.87563013641175,20.5030995980058));
#14934=CARTESIAN_POINT('Ctrl Pts',(7.96919850470418,-1.77275423134245,20.4972446246343));
#14935=CARTESIAN_POINT('Ctrl Pts',(8.01835209460449,-1.66777653690316,20.4913896512627));
#14936=CARTESIAN_POINT('Ctrl Pts',(8.06756139378336,-1.56267986373549,20.4855280420311));
#14937=CARTESIAN_POINT('Ctrl Pts',(8.11208084833505,-1.45547702102329,20.4796664327995));
#14938=CARTESIAN_POINT('Ctrl Pts',(8.15174747731444,-1.34662792192524,20.473804823568));
#14939=CARTESIAN_POINT('Ctrl Pts',(8.1914408537916,-1.2377054250843,20.4679392618104));
#14940=CARTESIAN_POINT('Ctrl Pts',(8.22627476499539,-1.12713485451428,20.4620737000529));
#14941=CARTESIAN_POINT('Ctrl Pts',(8.25613653612756,-1.01538978825197,20.4562081382954));
#14942=CARTESIAN_POINT('Ctrl Pts',(8.28604197249384,-0.903481323293121,
20.4503339996478));
#14943=CARTESIAN_POINT('Ctrl Pts',(8.31096067015872,-0.79039533705663,20.4444598610003));
#14944=CARTESIAN_POINT('Ctrl Pts',(8.33083128902692,-0.676614126679309,
20.4385857223527));
#14945=CARTESIAN_POINT('Ctrl Pts',(8.33585624585906,-0.647840706271703,
20.4371002480791));
#14946=CARTESIAN_POINT('Ctrl Pts',(8.34055863683056,-0.619022841748624,
20.4356147738054));
#14947=CARTESIAN_POINT('Ctrl Pts',(8.34493799733069,-0.590168351278482,
20.4341292995318));
#14948=CARTESIAN_POINT('Ctrl Pts',(8.37438559411386,-0.39614563935008,20.4241407070328));
#14949=CARTESIAN_POINT('Ctrl Pts',(8.38931639816492,-0.199865449716072,
20.4141521145339));
#14950=CARTESIAN_POINT('Ctrl Pts',(8.38946794062561,-0.00302796142341772,
20.404163522035));
#14951=CARTESIAN_POINT('',(8.38723842052662,0.00122266794094017,22.9041631982879));
#14952=CARTESIAN_POINT('Ctrl Pts',(8.38336796207569,0.00123261681410103,
22.9041626365075));
#14953=CARTESIAN_POINT('Ctrl Pts',(8.38497779636529,0.582186035453978,22.8748826604955));
#14954=CARTESIAN_POINT('Ctrl Pts',(7.99175245620736,2.47400439996808,22.7794306453466));
#14955=CARTESIAN_POINT('Ctrl Pts',(5.06563975414788,4.60896388279017,22.6178065910599));
#14956=CARTESIAN_POINT('Ctrl Pts',(0.913755812908484,3.01046009038452,22.4192904736486));
#14957=CARTESIAN_POINT('Ctrl Pts',(0.00621832850917159,-1.3449738921826,
22.2207743562367));
#14958=CARTESIAN_POINT('Ctrl Pts',(3.17413741150636,-4.46870214230704,22.0222582388252));
#14959=CARTESIAN_POINT('Ctrl Pts',(7.30539079965451,-3.54714769877334,21.8333884662538));
#14960=CARTESIAN_POINT('Ctrl Pts',(8.38348861036977,-1.11174890873364,21.7106907328197));
#14961=CARTESIAN_POINT('Ctrl Pts',(8.39284687402911,0.00293392250969736,
21.6541650385228));
#14962=CARTESIAN_POINT('',(8.38861467094264,-0.00383499285989103,24.1541639327802));
#14963=CARTESIAN_POINT('Ctrl Pts',(8.3894672436094,-0.00382769875130555,
24.154163522035));
#14964=CARTESIAN_POINT('Ctrl Pts',(8.38957872098432,0.110716401084503,24.1483738591514));
#14965=CARTESIAN_POINT('Ctrl Pts',(8.38468202707299,0.22538347931669,24.1425841962678));
#14966=CARTESIAN_POINT('Ctrl Pts',(8.37477179070765,0.339695558880501,24.1367945333842));
#14967=CARTESIAN_POINT('Ctrl Pts',(8.36486710287917,0.453943637469739,24.1310081120134));
#14968=CARTESIAN_POINT('Ctrl Pts',(8.34995448815683,0.567836691468084,24.1252216906425));
#14969=CARTESIAN_POINT('Ctrl Pts',(8.3300806409311,0.680898434525721,24.1194352692717));
#14970=CARTESIAN_POINT('Ctrl Pts',(8.31021213067698,0.793929815705951,24.1136504018007));
#14971=CARTESIAN_POINT('Ctrl Pts',(8.28538510867146,0.906129912621712,24.1078655343296));
#14972=CARTESIAN_POINT('Ctrl Pts',(8.25569783068645,1.01703003848253,24.1020806668586));
#14973=CARTESIAN_POINT('Ctrl Pts',(8.22601094500458,1.12792869885134,24.0962958758318));
#14974=CARTESIAN_POINT('Ctrl Pts',(8.19146404106767,1.23752701318639,24.090511084805));
#14975=CARTESIAN_POINT('Ctrl Pts',(8.15220573392728,1.34536975534977,24.0847262937782));
#14976=CARTESIAN_POINT('Ctrl Pts',(8.11293792104757,1.45323860982082,24.0789401020614));
#14977=CARTESIAN_POINT('Ctrl Pts',(8.06895658339419,1.55935064961409,24.0731539103447));
#14978=CARTESIAN_POINT('Ctrl Pts',(8.02045881068432,1.66326978763516,24.0673677186279));
#14979=CARTESIAN_POINT('Ctrl Pts',(7.9719085602857,1.76730137280327,24.0615752658821));
#14980=CARTESIAN_POINT('Ctrl Pts',(7.91883230006276,1.8691349359658,24.0557828131362));
#14981=CARTESIAN_POINT('Ctrl Pts',(7.86147349324196,1.96835823069616,24.0499903603903));
#14982=CARTESIAN_POINT('Ctrl Pts',(7.80407933131469,2.06764268517414,24.0441943372637));
#14983=CARTESIAN_POINT('Ctrl Pts',(7.74239759702477,2.16431331302349,24.038398314137));
#14984=CARTESIAN_POINT('Ctrl Pts',(7.67671450659402,2.25798772391674,24.0326022910103));
#14985=CARTESIAN_POINT('Ctrl Pts',(7.61093136673586,2.35180482101905,24.0267974392979));
#14986=CARTESIAN_POINT('Ctrl Pts',(7.54113496401743,2.44261625802189,24.0209925875855));
#14987=CARTESIAN_POINT('Ctrl Pts',(7.46765113422866,2.53007347604514,24.0151877358731));
#14988=CARTESIAN_POINT('Ctrl Pts',(7.43487130634739,2.5690865835821,24.012598294896));
#14989=CARTESIAN_POINT('Ctrl Pts',(7.40135820148236,2.6074327375437,24.0100088539189));
#14990=CARTESIAN_POINT('Ctrl Pts',(7.3671429492336,2.64508351089078,24.0074194129418));
#14991=CARTESIAN_POINT('Ctrl Pts',(7.28951033312009,2.73051114451976,24.0015441069273));
#14992=CARTESIAN_POINT('Ctrl Pts',(7.20798478842049,2.81265988752737,23.9956688009128));
#14993=CARTESIAN_POINT('Ctrl Pts',(7.12287415018794,2.89115429223226,23.9897934948984));
#14994=CARTESIAN_POINT('Ctrl Pts',(7.03787327883904,2.96954746298605,23.9839257662449));
#14995=CARTESIAN_POINT('Ctrl Pts',(6.94929680982533,3.04429539077778,23.9780580375915));
#14996=CARTESIAN_POINT('Ctrl Pts',(6.857491643667,3.11505694565336,23.972190308938));
#14997=CARTESIAN_POINT('Ctrl Pts',(6.76578039464117,3.18574611111335,23.9663285829996));
#14998=CARTESIAN_POINT('Ctrl Pts',(6.67084734352806,3.25245676483631,23.9604668570611));
#14999=CARTESIAN_POINT('Ctrl Pts',(6.57307442721387,3.3148862597581,23.9546051311227));
#15000=CARTESIAN_POINT('Ctrl Pts',(6.47181234780927,3.37954363840931,23.9485342213063));
#15001=CARTESIAN_POINT('Ctrl Pts',(6.36750425895161,3.43960828565306,23.94246331149));
#15002=CARTESIAN_POINT('Ctrl Pts',(6.26061003237402,3.49479105506607,23.9363924016736));
#15003=CARTESIAN_POINT('Ctrl Pts',(6.15751763618798,3.54801117844515,23.9305374115583));
#15004=CARTESIAN_POINT('Ctrl Pts',(6.05202032634843,3.5966905657536,23.9246824214429));
#15005=CARTESIAN_POINT('Ctrl Pts',(5.94455728337713,3.64061568652886,23.9188274313276));
#15006=CARTESIAN_POINT('Ctrl Pts',(5.83711042554598,3.68453419168804,23.9129733230395));
#15007=CARTESIAN_POINT('Ctrl Pts',(5.72769880536155,3.72369969793359,23.9071192147514));
#15008=CARTESIAN_POINT('Ctrl Pts',(5.61678201126526,3.7579466417688,23.9012651064632));
#15009=CARTESIAN_POINT('Ctrl Pts',(5.50585514034607,3.79219669694879,23.8954104663277));
#15010=CARTESIAN_POINT('Ctrl Pts',(5.39342321820423,3.82152717959801,23.8895558261921));
#15011=CARTESIAN_POINT('Ctrl Pts',(5.27996075302319,3.84582247479554,23.8837011860566));
#15012=CARTESIAN_POINT('Ctrl Pts',(5.16646058301809,3.87012584358667,23.8778446003598));
#15013=CARTESIAN_POINT('Ctrl Pts',(5.0519295925132,3.88939061130453,23.871988014663));
#15014=CARTESIAN_POINT('Ctrl Pts',(4.93685153040162,3.90355244956895,23.8661314289662));
#15015=CARTESIAN_POINT('Ctrl Pts',(4.82164342997129,3.91773029072397,23.860268225322));
#15016=CARTESIAN_POINT('Ctrl Pts',(4.70588743407938,3.92679364270126,23.8544050216778));
#15017=CARTESIAN_POINT('Ctrl Pts',(4.59007155145518,3.93073013403703,23.8485418180336));
#15018=CARTESIAN_POINT('Ctrl Pts',(4.47417776288739,3.93466927333493,23.8426746703845));
#15019=CARTESIAN_POINT('Ctrl Pts',(4.3582244192234,3.93347468899277,23.8368075227354));
#15020=CARTESIAN_POINT('Ctrl Pts',(4.24269692991518,3.92718607359502,23.8309403750863));
#15021=CARTESIAN_POINT('Ctrl Pts',(4.12700104370852,3.9208882916921,23.8250646752781));
#15022=CARTESIAN_POINT('Ctrl Pts',(4.01173266001832,3.90948170024186,23.8191889754699));
#15023=CARTESIAN_POINT('Ctrl Pts',(3.8973695681331,3.89305750105403,23.8133132756617));
#15024=CARTESIAN_POINT('Ctrl Pts',(3.86875799961211,3.88894846471443,23.8118432822845));
#15025=CARTESIAN_POINT('Ctrl Pts',(3.84020302981038,3.88452561834951,23.8103732889073));
#15026=CARTESIAN_POINT('Ctrl Pts',(3.81171199966483,3.87979088013116,23.80890329553));
#15027=CARTESIAN_POINT('Ctrl Pts',(3.6978466187317,3.86086833615514,23.8030284164887));
#15028=CARTESIAN_POINT('Ctrl Pts',(3.58462623467261,3.83689754454862,23.7971535374474));
#15029=CARTESIAN_POINT('Ctrl Pts',(3.47253316722319,3.80793370057226,23.7912786584061));
#15030=CARTESIAN_POINT('Ctrl Pts',(3.36058435047757,3.7790071296849,23.7854113396489));
#15031=CARTESIAN_POINT('Ctrl Pts',(3.24976036148445,3.74510038711803,23.7795440208917));
#15032=CARTESIAN_POINT('Ctrl Pts',(3.14053585228774,3.70632009831853,23.7736767021345));
#15033=CARTESIAN_POINT('Ctrl Pts',(3.03142276210058,3.66757936896773,23.7678153685802));
#15034=CARTESIAN_POINT('Ctrl Pts',(2.92390629310609,3.62397511950738,23.7619540350258));
#15035=CARTESIAN_POINT('Ctrl Pts',(2.8184477448103,3.5756642766864,23.7560927014715));
#15036=CARTESIAN_POINT('Ctrl Pts',(2.70921568447076,3.52562477791316,23.7500216379984));
#15037=CARTESIAN_POINT('Ctrl Pts',(2.60219201303895,3.47053566783608,23.7439505745254));
#15038=CARTESIAN_POINT('Ctrl Pts',(2.49786904705436,3.41062674713068,23.7378795110523));
#15039=CARTESIAN_POINT('Ctrl Pts',(2.39726494954109,3.35285343860099,23.7320248667189));
#15040=CARTESIAN_POINT('Ctrl Pts',(2.29917268481772,3.29059830715117,23.7261702223854));
#15041=CARTESIAN_POINT('Ctrl Pts',(2.2040096801521,3.22411468994603,23.7203155780519));
#15042=CARTESIAN_POINT('Ctrl Pts',(2.10886071749359,3.15764088289168,23.7144617976147));
#15043=CARTESIAN_POINT('Ctrl Pts',(2.01664049387269,3.08694006716538,23.7086080171774));
#15044=CARTESIAN_POINT('Ctrl Pts',(1.92773718261452,3.01230872563677,23.7027542367401));
#15045=CARTESIAN_POINT('Ctrl Pts',(1.83882551486383,2.93767036911357,23.6968999060751));
#15046=CARTESIAN_POINT('Ctrl Pts',(1.75323169556833,2.85910101785432,23.69104557541));
#15047=CARTESIAN_POINT('Ctrl Pts',(1.67131000399742,2.77693676113024,23.685191244745));
#15048=CARTESIAN_POINT('Ctrl Pts',(1.58936082382134,2.69474493440889,23.6793349496749));
#15049=CARTESIAN_POINT('Ctrl Pts',(1.51108651293609,2.60895609586038,23.6734786546048));
#15050=CARTESIAN_POINT('Ctrl Pts',(1.43680325412089,2.51994189251998,23.6676223595347));
#15051=CARTESIAN_POINT('Ctrl Pts',(1.36243567570538,2.43082664835063,23.661759416931));
#15052=CARTESIAN_POINT('Ctrl Pts',(1.29206845627402,2.33847904918574,23.6558964743273));
#15053=CARTESIAN_POINT('Ctrl Pts',(1.22597642064575,2.24330247814747,23.6500335317235));
#15054=CARTESIAN_POINT('Ctrl Pts',(1.1598397336403,2.14806160639685,23.6441666281515));
#15055=CARTESIAN_POINT('Ctrl Pts',(1.09798420146503,2.04998830545557,23.6382997245794));
#15056=CARTESIAN_POINT('Ctrl Pts',(1.04063948185516,1.9495119844011,23.6324328210074));
#15057=CARTESIAN_POINT('Ctrl Pts',(0.983210908885853,1.84888874001837,23.6265573384488));
#15058=CARTESIAN_POINT('Ctrl Pts',(0.930306500406061,1.74585582866359,23.6206818558903));
#15059=CARTESIAN_POINT('Ctrl Pts',(0.882108493602307,1.64086416591374,23.6148063733318));
#15060=CARTESIAN_POINT('Ctrl Pts',(0.870024583963843,1.61454129802779,23.6133333082606));
#15061=CARTESIAN_POINT('Ctrl Pts',(0.858236263459379,1.58809538796028,23.6118602431895));
#15062=CARTESIAN_POINT('Ctrl Pts',(0.846745912493526,1.56153368989778,23.6103871781184));
#15063=CARTESIAN_POINT('Ctrl Pts',(0.800938032747483,1.45564179205121,23.6045145996536));
#15064=CARTESIAN_POINT('Ctrl Pts',(0.759717063322716,1.34755549104644,23.5986420211887));
#15065=CARTESIAN_POINT('Ctrl Pts',(0.723298308983122,1.23770949688158,23.5927694427239));
#15066=CARTESIAN_POINT('Ctrl Pts',(0.686926674708178,1.12800562592879,23.5869044624398));
#15067=CARTESIAN_POINT('Ctrl Pts',(0.655345028307665,1.01654697822477,23.5810394821557));
#15068=CARTESIAN_POINT('Ctrl Pts',(0.628721323107011,0.903789748164359,
23.5751745018716));
#15069=CARTESIAN_POINT('Ctrl Pts',(0.602124945671036,0.791148257180299,
23.5693155416662));
#15070=CARTESIAN_POINT('Ctrl Pts',(0.580476481403955,0.677211234967463,
23.5634565814608));
#15071=CARTESIAN_POINT('Ctrl Pts',(0.563894391757136,0.562450968830149,
23.5575976212554));
#15072=CARTESIAN_POINT('Ctrl Pts',(0.54670952443267,0.443519037469597,23.5515256812325));
#15073=CARTESIAN_POINT('Ctrl Pts',(0.534966516338779,0.323703301238925,
23.5454537412096));
#15074=CARTESIAN_POINT('Ctrl Pts',(0.52873955281778,0.203542514833005,23.5393818011868));
#15075=CARTESIAN_POINT('Ctrl Pts',(0.522737940790728,0.0877303025979404,
23.5335296024151));
#15076=CARTESIAN_POINT('Ctrl Pts',(0.521860071897171,-0.0284019698800386,
23.5276774036435));
#15077=CARTESIAN_POINT('Ctrl Pts',(0.526119592198509,-0.144366539214522,
23.5218252048718));
#15078=CARTESIAN_POINT('Ctrl Pts',(0.530378467271945,-0.260313542351281,
23.5159738925854));
#15079=CARTESIAN_POINT('Ctrl Pts',(0.539773169020989,-0.376092479920382,
23.510122580299));
#15080=CARTESIAN_POINT('Ctrl Pts',(0.554265228645449,-0.491216752417696,
23.5042712680126));
#15081=CARTESIAN_POINT('Ctrl Pts',(0.568758601425841,-0.606351456566922,
23.4984194255265));
#15082=CARTESIAN_POINT('Ctrl Pts',(0.588350198618752,-0.720830967609783,
23.4925675830404));
#15083=CARTESIAN_POINT('Ctrl Pts',(0.612949892469742,-0.834175673072546,
23.4867157405544));
#15084=CARTESIAN_POINT('Ctrl Pts',(0.637557770711563,-0.947558088653727,
23.480861951143));
#15085=CARTESIAN_POINT('Ctrl Pts',(0.66717697113529,-1.05980454421068,23.4750081617316));
#15086=CARTESIAN_POINT('Ctrl Pts',(0.701666829446231,-1.17044814594567,
23.4691543723202));
#15087=CARTESIAN_POINT('Ctrl Pts',(0.736195775273815,-1.28121714058848,
23.4632939487821));
#15088=CARTESIAN_POINT('Ctrl Pts',(0.775606273355798,-1.39037926092924,
23.457433525244));
#15089=CARTESIAN_POINT('Ctrl Pts',(0.819708565962934,-1.49748514945619,
23.4515731017059));
#15090=CARTESIAN_POINT('Ctrl Pts',(0.863840584538135,-1.60466322983608,
23.4457087281064));
#15091=CARTESIAN_POINT('Ctrl Pts',(0.912670520868715,-1.70978194477564,
23.439844354507));
#15092=CARTESIAN_POINT('Ctrl Pts',(0.965962257586456,-1.81241577449947,
23.4339799809075));
#15093=CARTESIAN_POINT('Ctrl Pts',(1.01933198579058,-1.9151998069644,23.428107024904));
#15094=CARTESIAN_POINT('Ctrl Pts',(1.07717634040011,-2.01549133986442,23.4222340689005));
#15095=CARTESIAN_POINT('Ctrl Pts',(1.13921542089719,-2.11289303733621,23.416361112897));
#15096=CARTESIAN_POINT('Ctrl Pts',(1.15502567097137,-2.13771521687756,23.4148644288336));
#15097=CARTESIAN_POINT('Ctrl Pts',(1.17110814291829,-2.16234988164376,23.4133677447702));
#15098=CARTESIAN_POINT('Ctrl Pts',(1.18745779228822,-2.18679080604374,23.4118710607068));
#15099=CARTESIAN_POINT('Ctrl Pts',(1.25162480698497,-2.2827134230792,23.4059970663402));
#15100=CARTESIAN_POINT('Ctrl Pts',(1.32012417082163,-2.3759689987107,23.4001230719736));
#15101=CARTESIAN_POINT('Ctrl Pts',(1.39270701194138,-2.46614087790462,23.3942490776071));
#15102=CARTESIAN_POINT('Ctrl Pts',(1.46519617184847,-2.55619637406833,23.3883826646868));
#15103=CARTESIAN_POINT('Ctrl Pts',(1.54175807112617,-2.64317576999886,23.3825162517666));
#15104=CARTESIAN_POINT('Ctrl Pts',(1.62210012899226,-2.72669057667694,23.3766498388464));
#15105=CARTESIAN_POINT('Ctrl Pts',(1.70235994456939,-2.81011989327616,23.3707894310901));
#15106=CARTESIAN_POINT('Ctrl Pts',(1.78639193713453,-2.89009137905395,23.3649290233338));
#15107=CARTESIAN_POINT('Ctrl Pts',(1.87386318781676,-2.96624942819001,23.3590686155774));
#15108=CARTESIAN_POINT('Ctrl Pts',(1.96448371064007,-3.0451494344902,23.3529972125657));
#15109=CARTESIAN_POINT('Ctrl Pts',(2.05879552561944,-3.11995588402797,23.3469258095539));
#15110=CARTESIAN_POINT('Ctrl Pts',(2.15638626882769,-3.19031470879306,23.3408544065422));
#15111=CARTESIAN_POINT('Ctrl Pts',(2.25047727794221,-3.25815037234706,23.3350007321327));
#15112=CARTESIAN_POINT('Ctrl Pts',(2.34761571722282,-3.32185166556091,23.3291470577232));
#15113=CARTESIAN_POINT('Ctrl Pts',(2.44739888087793,-3.38114268105488,23.3232933833138));
#15114=CARTESIAN_POINT('Ctrl Pts',(2.54716706759119,-3.44042479727107,23.3174405875109));
#15115=CARTESIAN_POINT('Ctrl Pts',(2.64957883433474,-3.49529774103474,23.311587791708));
#15116=CARTESIAN_POINT('Ctrl Pts',(2.7542042123478,-3.54553003528332,23.3057349959051));
#15117=CARTESIAN_POINT('Ctrl Pts',(2.85883918116785,-3.59576693422963,23.2998816635876));
#15118=CARTESIAN_POINT('Ctrl Pts',(2.96568779222055,-3.64136215920086,23.2940283312702));
#15119=CARTESIAN_POINT('Ctrl Pts',(3.07429795205795,-3.68213143445575,23.2881749989528));
#15120=CARTESIAN_POINT('Ctrl Pts',(3.18294432583411,-3.72291430343004,23.2823197149559));
#15121=CARTESIAN_POINT('Ctrl Pts',(3.29335302978794,-3.75886787792341,23.276464430959));
#15122=CARTESIAN_POINT('Ctrl Pts',(3.40505526806061,-3.78985724545537,23.2706091469621));
#15123=CARTESIAN_POINT('Ctrl Pts',(3.51688405793957,-3.82088172199051,23.2647472292969));
#15124=CARTESIAN_POINT('Ctrl Pts',(3.63000890889168,-3.84693065562783,23.2588853116318));
#15125=CARTESIAN_POINT('Ctrl Pts',(3.7439491511572,-3.86791989493575,23.2530233939666));
#15126=CARTESIAN_POINT('Ctrl Pts',(3.85796620256293,-3.88892328346253,23.2471575246786));
#15127=CARTESIAN_POINT('Ctrl Pts',(3.97279933163732,-3.90486012927119,23.2412916553907));
#15128=CARTESIAN_POINT('Ctrl Pts',(4.08796276814762,-3.91569815981796,23.2354257861027));
#15129=CARTESIAN_POINT('Ctrl Pts',(4.20329452048084,-3.92655203056615,23.2295513436196));
#15130=CARTESIAN_POINT('Ctrl Pts',(4.31895713270896,-3.93229219308944,23.2236769011366));
#15131=CARTESIAN_POINT('Ctrl Pts',(4.43446478202045,-3.93293844468949,23.2178024586535));
#15132=CARTESIAN_POINT('Ctrl Pts',(4.46361489829682,-3.93310153613319,23.216319953534));
#15133=CARTESIAN_POINT('Ctrl Pts',(4.49275517300633,-3.93294046322736,23.2148374484145));
#15134=CARTESIAN_POINT('Ctrl Pts',(4.52187786675592,-3.93245606384164,23.2133549432951));
#15135=CARTESIAN_POINT('Ctrl Pts',(4.63726460974797,-3.93053682972457,23.2074811241122));
#15136=CARTESIAN_POINT('Ctrl Pts',(4.752758877098,-3.92353155340743,23.2016073049293));
#15137=CARTESIAN_POINT('Ctrl Pts',(4.867875659089,-3.91142348106862,23.1957334857464));
#15138=CARTESIAN_POINT('Ctrl Pts',(4.98284387373924,-3.89933103515785,23.1898672471932));
#15139=CARTESIAN_POINT('Ctrl Pts',(5.0974351647547,-3.88214893258858,23.18400100864));
#15140=CARTESIAN_POINT('Ctrl Pts',(5.21116449427817,-3.85991241756093,23.1781347700868));
#15141=CARTESIAN_POINT('Ctrl Pts',(5.3247774210237,-3.83769866176462,23.1722745356705));
#15142=CARTESIAN_POINT('Ctrl Pts',(5.4375297380568,-3.8104408623037,23.1664143012542));
#15143=CARTESIAN_POINT('Ctrl Pts',(5.54894217099982,-3.7782259861907,23.1605540668379));
#15144=CARTESIAN_POINT('Ctrl Pts',(5.66437049944754,-3.74484991493324,23.1544825984648));
#15145=CARTESIAN_POINT('Ctrl Pts',(5.77836007944622,-3.70615271434604,23.1484111300917));
#15146=CARTESIAN_POINT('Ctrl Pts',(5.89038980051059,-3.66228896217654,23.1423396617186));
#15147=CARTESIAN_POINT('Ctrl Pts',(5.99839769379383,-3.6199999033597,23.1364861569354));
#15148=CARTESIAN_POINT('Ctrl Pts',(6.10458360750112,-3.57290903297098,23.1306326521522));
#15149=CARTESIAN_POINT('Ctrl Pts',(6.20849740629629,-3.52120516808175,23.1247791473689));
#15150=CARTESIAN_POINT('Ctrl Pts',(6.31239563745666,-3.46950904910207,23.1189265195166));
#15151=CARTESIAN_POINT('Ctrl Pts',(6.41402206076365,-3.41320149374667,23.1130738916643));
#15152=CARTESIAN_POINT('Ctrl Pts',(6.51294909697806,-3.35251831428323,23.107221263812));
#15153=CARTESIAN_POINT('Ctrl Pts',(6.61188523344937,-3.29182955259937,23.1013680975789));
#15154=CARTESIAN_POINT('Ctrl Pts',(6.7081211370295,-3.22676458267386,23.0955149313458));
#15155=CARTESIAN_POINT('Ctrl Pts',(6.80125689887346,-3.15760339615587,23.0896617651127));
#15156=CARTESIAN_POINT('Ctrl Pts',(6.89442374865687,-3.08841912421144,23.0838066451416));
#15157=CARTESIAN_POINT('Ctrl Pts',(6.9844880675476,-3.0151361630527,23.0779515251705));
#15158=CARTESIAN_POINT('Ctrl Pts',(7.07108237348684,-2.93807529900495,23.0720964051994));
#15159=CARTESIAN_POINT('Ctrl Pts',(7.15777484577421,-2.86092707605381,23.0662346476585));
#15160=CARTESIAN_POINT('Ctrl Pts',(7.24098914483427,-2.77999267686708,23.0603728901177));
#15161=CARTESIAN_POINT('Ctrl Pts',(7.32039400746091,-2.69563038268273,23.0545111325768));
#15162=CARTESIAN_POINT('Ctrl Pts',(7.3998524279898,-2.61121118685083,23.0486454213305));
#15163=CARTESIAN_POINT('Ctrl Pts',(7.47549602687772,-2.52335980442883,23.0427797100843));
#15164=CARTESIAN_POINT('Ctrl Pts',(7.54703437145913,-2.43246692501389,23.036913998838));
#15165=CARTESIAN_POINT('Ctrl Pts',(7.61867732712394,-2.34144113222718,23.031039710116));
#15166=CARTESIAN_POINT('Ctrl Pts',(7.68620280773775,-2.24736530047097,23.0251654213941));
#15167=CARTESIAN_POINT('Ctrl Pts',(7.74936410791157,-2.15065838938292,23.0192911326722));
#15168=CARTESIAN_POINT('Ctrl Pts',(7.76532141490701,-2.12622599384061,23.0178070304093));
#15169=CARTESIAN_POINT('Ctrl Pts',(7.78100039336455,-2.10162577615285,23.0163229281464));
#15170=CARTESIAN_POINT('Ctrl Pts',(7.7963975407554,-2.07686471686776,23.0148388258835));
#15171=CARTESIAN_POINT('Ctrl Pts',(7.859037879908,-1.97612909928727,23.0088010406544));
#15172=CARTESIAN_POINT('Ctrl Pts',(7.91720903096368,-1.87240947858011,23.0027632554254));
#15173=CARTESIAN_POINT('Ctrl Pts',(7.97062389833732,-1.76612714633646,22.9967254701964));
#15174=CARTESIAN_POINT('Ctrl Pts',(8.02395744405096,-1.66000662401786,22.9906968772156));
#15175=CARTESIAN_POINT('Ctrl Pts',(8.07254894942104,-1.55133149453898,22.9846682842348));
#15176=CARTESIAN_POINT('Ctrl Pts',(8.11615516574377,-1.44055091743213,22.978639691254));
#15177=CARTESIAN_POINT('Ctrl Pts',(8.16104712140932,-1.32650394946593,22.9724333438191));
#15178=CARTESIAN_POINT('Ctrl Pts',(8.20065500283404,-1.21022577448384,22.9662269963841));
#15179=CARTESIAN_POINT('Ctrl Pts',(8.23476416089464,-1.0922341689436,22.9600206489492));
#15180=CARTESIAN_POINT('Ctrl Pts',(8.26780337610315,-0.977943747546674,
22.9540089834547));
#15181=CARTESIAN_POINT('Ctrl Pts',(8.29568352281609,-0.862046175210224,
22.9479973179601));
#15182=CARTESIAN_POINT('Ctrl Pts',(8.31825837322447,-0.745031984035302,
22.9419856524656));
#15183=CARTESIAN_POINT('Ctrl Pts',(8.34192982049566,-0.622333706692535,
22.9356819640605));
#15184=CARTESIAN_POINT('Ctrl Pts',(8.35976743530867,-0.498407995694312,
22.9293782756554));
#15185=CARTESIAN_POINT('Ctrl Pts',(8.37166192269059,-0.373837143477487,
22.9230745872503));
#15186=CARTESIAN_POINT('Ctrl Pts',(8.3835564100725,-0.249266291260661,22.9167708988452));
#15187=CARTESIAN_POINT('Ctrl Pts',(8.38950767782919,-0.12405077695408,22.9104672104401));
#15188=CARTESIAN_POINT('Ctrl Pts',(8.38946891794852,0.00121693452816299,
22.904163522035));
#15189=CARTESIAN_POINT('',(2.70777463088706,3.52286199445081,25.));
#15190=CARTESIAN_POINT('Ctrl Pts',(2.70777463088727,3.52286199445091,25.));
#15191=CARTESIAN_POINT('Ctrl Pts',(1.53601102873651,2.94121657640656,24.9338279608628));
#15192=CARTESIAN_POINT('Ctrl Pts',(-0.161182576319996,0.526756619563024,
24.8014838825885));
#15193=CARTESIAN_POINT('Ctrl Pts',(1.51353445936752,-3.60293174152366,24.6029677651766));
#15194=CARTESIAN_POINT('Ctrl Pts',(5.88727120760258,-4.42203261044561,24.4044516477652));
#15195=CARTESIAN_POINT('Ctrl Pts',(8.19434681762875,-1.99168802557944,24.254850422542));
#15196=CARTESIAN_POINT('Ctrl Pts',(8.39132408849758,-0.345158373668096,
24.1714212364563));
#15197=CARTESIAN_POINT('Ctrl Pts',(8.38828935556429,-0.00383777606628122,
24.1541640895078));
#15198=CARTESIAN_POINT('',(6.2051666064271,3.52286049294652,24.999933612301));
#15199=CARTESIAN_POINT('Origin',(4.45646910621825,5.55111512312578E-15,
25.));
#15200=CARTESIAN_POINT('',(8.38946742624093,-0.00363520271639387,23.9708364988139));
#15201=CARTESIAN_POINT('Ctrl Pts',(8.38946742624093,-0.00363520271639387,
23.9708364988139));
#15202=CARTESIAN_POINT('Ctrl Pts',(8.38933012983173,-0.152178926091542,
23.9783480087104));
#15203=CARTESIAN_POINT('Ctrl Pts',(8.38077390761021,-0.300347425473105,
23.9858595186069));
#15204=CARTESIAN_POINT('Ctrl Pts',(8.36394689447948,-0.447332465002422,
23.9933710285034));
#15205=CARTESIAN_POINT('Ctrl Pts',(8.34673858497178,-0.597648152853239,
24.0010527475444));
#15206=CARTESIAN_POINT('Ctrl Pts',(8.320880397383,-0.74672642332909,24.0087344665854));
#15207=CARTESIAN_POINT('Ctrl Pts',(8.28657873929154,-0.893727698261136,
24.0164161856264));
#15208=CARTESIAN_POINT('Ctrl Pts',(8.28057428401054,-0.919460057298328,
24.0177608593544));
#15209=CARTESIAN_POINT('Ctrl Pts',(8.27431122111926,-0.945128826938406,
24.0191055330824));
#15210=CARTESIAN_POINT('Ctrl Pts',(8.26779080650492,-0.970729569408433,
24.0204502068104));
#15211=CARTESIAN_POINT('Ctrl Pts',(8.23930241018745,-1.08258198074202,24.0263252316895));
#15212=CARTESIAN_POINT('Ctrl Pts',(8.20583861026129,-1.19336520554438,24.0322002565686));
#15213=CARTESIAN_POINT('Ctrl Pts',(8.16749505797018,-1.30260331084475,24.0380752814478));
#15214=CARTESIAN_POINT('Ctrl Pts',(8.12920103269124,-1.41170031714287,24.0439427177647));
#15215=CARTESIAN_POINT('Ctrl Pts',(8.08603992529645,-1.51925578683239,24.0498101540817));
#15216=CARTESIAN_POINT('Ctrl Pts',(8.03815798798727,-1.62480575891772,24.0556775903987));
#15217=CARTESIAN_POINT('Ctrl Pts',(7.99032512344514,-1.73024755599002,24.0615390133555));
#15218=CARTESIAN_POINT('Ctrl Pts',(7.9377812223183,-1.83368756997744,24.0674004363123));
#15219=CARTESIAN_POINT('Ctrl Pts',(7.88072153424563,-1.9346793814864,24.0732618592691));
#15220=CARTESIAN_POINT('Ctrl Pts',(7.82162147027464,-2.03928252115172,24.0793328786422));
#15221=CARTESIAN_POINT('Ctrl Pts',(7.75767676660413,-2.14125866643526,24.0854038980152));
#15222=CARTESIAN_POINT('Ctrl Pts',(7.68915788820171,-2.24013665628646,24.0914749173882));
#15223=CARTESIAN_POINT('Ctrl Pts',(7.6230808545844,-2.33549087707562,24.0973295805199));
#15224=CARTESIAN_POINT('Ctrl Pts',(7.55275036285019,-2.42796362735164,24.1031842436515));
#15225=CARTESIAN_POINT('Ctrl Pts',(7.47845403191733,-2.51716032640901,24.1090389067831));
#15226=CARTESIAN_POINT('Ctrl Pts',(7.40416899530404,-2.60634346603469,24.1148926799053));
#15227=CARTESIAN_POINT('Ctrl Pts',(7.32591958247458,-2.69225122749522,24.1207464530275));
#15228=CARTESIAN_POINT('Ctrl Pts',(7.24403394073769,-2.77452181345733,24.1266002261497));
#15229=CARTESIAN_POINT('Ctrl Pts',(7.16214096730267,-2.85679976558388,24.1324545233943));
#15230=CARTESIAN_POINT('Ctrl Pts',(7.07661140908675,-2.93543960214524,24.1383088206388));
#15231=CARTESIAN_POINT('Ctrl Pts',(6.98781002448427,-3.01011663486851,24.1441631178834));
#15232=CARTESIAN_POINT('Ctrl Pts',(6.89897923880363,-3.08481839226567,24.1500193534159));
#15233=CARTESIAN_POINT('Ctrl Pts',(6.80687478858566,-3.15555447124593,24.1558755889484));
#15234=CARTESIAN_POINT('Ctrl Pts',(6.71189365531805,-3.22204113929632,24.1617318244808));
#15235=CARTESIAN_POINT('Ctrl Pts',(6.61680532874655,-3.28860284251809,24.1675946692126));
#15236=CARTESIAN_POINT('Ctrl Pts',(6.5188341776721,-3.35090532574933,24.1734575139443));
#15237=CARTESIAN_POINT('Ctrl Pts',(6.41840532143876,-3.40870874194411,24.1793203586761));
#15238=CARTESIAN_POINT('Ctrl Pts',(6.31790900000042,-3.46655098880439,24.1851871418976));
#15239=CARTESIAN_POINT('Ctrl Pts',(6.21495205157806,-3.51988796087664,24.1910539251191));
#15240=CARTESIAN_POINT('Ctrl Pts',(6.10998172615481,-3.56852700924492,24.1969207083406));
#15241=CARTESIAN_POINT('Ctrl Pts',(6.00485847347324,-3.61723691798526,24.2027960386545));
#15242=CARTESIAN_POINT('Ctrl Pts',(5.89771637034563,-3.66123508732565,24.2086713689684));
#15243=CARTESIAN_POINT('Ctrl Pts',(5.78902010226335,-3.70037793244679,24.2145466992823));
#15244=CARTESIAN_POINT('Ctrl Pts',(5.7617650821707,-3.71019279591066,24.2160199075956));
#15245=CARTESIAN_POINT('Ctrl Pts',(5.73441240637848,-3.71970264008899,24.2174931159088));
#15246=CARTESIAN_POINT('Ctrl Pts',(5.7069695069686,-3.72890570378538,24.218966324222));
#15247=CARTESIAN_POINT('Ctrl Pts',(5.59752569619918,-3.76560803420041,24.2248415609982));
#15248=CARTESIAN_POINT('Ctrl Pts',(5.48628331429453,-3.79754882582684,24.2307167977744));
#15249=CARTESIAN_POINT('Ctrl Pts',(5.3736942655493,-3.82455056275768,24.2365920345506));
#15250=CARTESIAN_POINT('Ctrl Pts',(5.26125020068939,-3.85151752884025,24.2424597056295));
#15251=CARTESIAN_POINT('Ctrl Pts',(5.14746331553314,-3.87355799324999,24.2483273767085));
#15252=CARTESIAN_POINT('Ctrl Pts',(5.03280286735199,-3.89054345763897,24.2541950477874));
#15253=CARTESIAN_POINT('Ctrl Pts',(4.91825949136105,-3.90751157929513,24.260056727776));
#15254=CARTESIAN_POINT('Ctrl Pts',(4.80284473252738,-3.91943490723643,24.2659184077646));
#15255=CARTESIAN_POINT('Ctrl Pts',(4.68703965175696,-3.92623563015899,24.2717800877532));
#15256=CARTESIAN_POINT('Ctrl Pts',(4.56710053808121,-3.93327912664688,24.2778510191649));
#15257=CARTESIAN_POINT('Ctrl Pts',(4.44674315279411,-3.93482734251477,24.2839219505766));
#15258=CARTESIAN_POINT('Ctrl Pts',(4.3265100107905,-3.93085227826175,24.2899928819883));
#15259=CARTESIAN_POINT('Ctrl Pts',(4.21055385895036,-3.92701861687341,24.2958478553579));
#15260=CARTESIAN_POINT('Ctrl Pts',(4.09471370924887,-3.91804795116584,24.3017028287276));
#15261=CARTESIAN_POINT('Ctrl Pts',(3.97947710394769,-3.90396819015856,24.3075578020973));
#15262=CARTESIAN_POINT('Ctrl Pts',(3.86425764172276,-3.88989052371503,24.3134119044568));
#15263=CARTESIAN_POINT('Ctrl Pts',(3.74964195509695,-3.8707053233214,24.3192660068164));
#15264=CARTESIAN_POINT('Ctrl Pts',(3.63611199311522,-3.84649232509064,24.3251201091759));
#15265=CARTESIAN_POINT('Ctrl Pts',(3.52257150699411,-3.82227708233374,24.3309747542062));
#15266=CARTESIAN_POINT('Ctrl Pts',(3.41011734942133,-3.79303320133721,24.3368293992364));
#15267=CARTESIAN_POINT('Ctrl Pts',(3.29922011882796,-3.75889129680337,24.3426840442667));
#15268=CARTESIAN_POINT('Ctrl Pts',(3.18828583061333,-3.7247379833483,24.3485406456958));
#15269=CARTESIAN_POINT('Ctrl Pts',(3.07890989831364,-3.68568351315681,24.354397247125));
#15270=CARTESIAN_POINT('Ctrl Pts',(2.97154595985575,-3.64190777606969,24.3602538485541));
#15271=CARTESIAN_POINT('Ctrl Pts',(2.86406040794536,-3.59808245325947,24.3661170838822));
#15272=CARTESIAN_POINT('Ctrl Pts',(2.75859178123781,-3.54952534544128,24.3719803192103));
#15273=CARTESIAN_POINT('Ctrl Pts',(2.65557208355584,-3.49646377269458,24.3778435545384));
#15274=CARTESIAN_POINT('Ctrl Pts',(2.55248292375787,-3.4433664226237,24.3837107432147));
#15275=CARTESIAN_POINT('Ctrl Pts',(2.45184633842582,-3.38575876443387,24.389577931891));
#15276=CARTESIAN_POINT('Ctrl Pts',(2.35406665645412,-3.32391229415364,24.3954451205673));
#15277=CARTESIAN_POINT('Ctrl Pts',(2.25614422635233,-3.26197553448193,24.4013208747266));
#15278=CARTESIAN_POINT('Ctrl Pts',(2.16108736102153,-3.19578784755157,24.407196628886));
#15279=CARTESIAN_POINT('Ctrl Pts',(2.06926860346537,-3.12566197143203,24.4130723830453));
#15280=CARTESIAN_POINT('Ctrl Pts',(2.04629702175556,-3.10811760102093,24.4145424025748));
#15281=CARTESIAN_POINT('Ctrl Pts',(2.02352794312778,-3.09032691541717,24.4160124221043));
#15282=CARTESIAN_POINT('Ctrl Pts',(2.00096683935795,-3.07229517095019,24.4174824416337));
#15283=CARTESIAN_POINT('Ctrl Pts',(1.91094497346396,-3.00034606337101,24.4233480190582));
#15284=CARTESIAN_POINT('Ctrl Pts',(1.82393565654982,-2.92431514790276,24.4292135964826));
#15285=CARTESIAN_POINT('Ctrl Pts',(1.74033251279291,-2.84448431281591,24.4350791739071));
#15286=CARTESIAN_POINT('Ctrl Pts',(1.65683770803279,-2.7647569282956,24.4409371502923));
#15287=CARTESIAN_POINT('Ctrl Pts',(1.57674059598749,-2.68123969966455,24.4467951266775));
#15288=CARTESIAN_POINT('Ctrl Pts',(1.50040311551035,-2.59425574270928,24.4526531030628));
#15289=CARTESIAN_POINT('Ctrl Pts',(1.42414401815731,-2.50736110065214,24.4585050644933));
#15290=CARTESIAN_POINT('Ctrl Pts',(1.35163714593628,-2.41700711978729,24.4643570259237));
#15291=CARTESIAN_POINT('Ctrl Pts',(1.28320831761017,-2.32355438229501,24.4702089873542));
#15292=CARTESIAN_POINT('Ctrl Pts',(1.21217650993141,-2.22654677542837,24.4762835528414));
#15293=CARTESIAN_POINT('Ctrl Pts',(1.14553949184232,-2.1262002924728,24.4823581183285));
#15294=CARTESIAN_POINT('Ctrl Pts',(1.08361666321857,-2.02295709241472,24.4884326838156));
#15295=CARTESIAN_POINT('Ctrl Pts',(1.0240313716104,-1.92361124018631,24.4942779393375));
#15296=CARTESIAN_POINT('Ctrl Pts',(0.968811035467309,-1.82158379424227,
24.5001231948594));
#15297=CARTESIAN_POINT('Ctrl Pts',(0.918196132723883,-1.71729827491886,
24.5059684503812));
#15298=CARTESIAN_POINT('Ctrl Pts',(0.867588629715818,-1.61302800180167,
24.5118128513456));
#15299=CARTESIAN_POINT('Ctrl Pts',(0.821585402365603,-1.5065006843668,24.51765725231));
#15300=CARTESIAN_POINT('Ctrl Pts',(0.780380357407895,-1.39816326331008,
24.5235016532744));
#15301=CARTESIAN_POINT('Ctrl Pts',(0.739171299207984,-1.28981529052819,
24.5293466234652));
#15302=CARTESIAN_POINT('Ctrl Pts',(0.702761499724706,-1.17965725101988,
24.5351915936559));
#15303=CARTESIAN_POINT('Ctrl Pts',(0.67129596052861,-1.06815413548326,24.5410365638466));
#15304=CARTESIAN_POINT('Ctrl Pts',(0.639819691834387,-0.956612998272772,
24.5468835271256));
#15305=CARTESIAN_POINT('Ctrl Pts',(0.613291148174243,-0.843726271658716,
24.5527304904046));
#15306=CARTESIAN_POINT('Ctrl Pts',(0.591804726849639,-0.729971393165113,
24.5585774536836));
#15307=CARTESIAN_POINT('Ctrl Pts',(0.570293550341119,-0.616085454086971,
24.5644311534334));
#15308=CARTESIAN_POINT('Ctrl Pts',(0.553836167676953,-0.501329774199917,
24.5702848531833));
#15309=CARTESIAN_POINT('Ctrl Pts',(0.542475388479427,-0.386189302675539,
24.5761385529331));
#15310=CARTESIAN_POINT('Ctrl Pts',(0.531106843665713,-0.270970127332164,
24.5819962539566));
#15311=CARTESIAN_POINT('Ctrl Pts',(0.524841860939504,-0.155366049371791,
24.58785395498));
#15312=CARTESIAN_POINT('Ctrl Pts',(0.523671124009247,-0.0398626533586009,
24.5937116560034));
#15313=CARTESIAN_POINT('Ctrl Pts',(0.522498646528485,0.0758124631230528,
24.5995780657506));
#15314=CARTESIAN_POINT('Ctrl Pts',(0.52643551552501,0.191386186441255,24.6054444754977));
#15315=CARTESIAN_POINT('Ctrl Pts',(0.53542053161511,0.306377341855894,24.6113108852449));
#15316=CARTESIAN_POINT('Ctrl Pts',(0.537813751451311,0.337006014232916,
24.6128734431783));
#15317=CARTESIAN_POINT('Ctrl Pts',(0.540564835520931,0.367593410839932,
24.6144360011118));
#15318=CARTESIAN_POINT('Ctrl Pts',(0.543672019020073,0.398130574577568,
24.6159985590453));
#15319=CARTESIAN_POINT('Ctrl Pts',(0.555374373293993,0.513140424712632,
24.6218835048544));
#15320=CARTESIAN_POINT('Ctrl Pts',(0.572170952547528,0.627822293185062,
24.6277684506634));
#15321=CARTESIAN_POINT('Ctrl Pts',(0.594036604177521,0.741690074882627,
24.6336533964725));
#15322=CARTESIAN_POINT('Ctrl Pts',(0.615873974234077,0.85541057718122,24.6395307305474));
#15323=CARTESIAN_POINT('Ctrl Pts',(0.642767300034292,0.968318686419494,
24.6454080646223));
#15324=CARTESIAN_POINT('Ctrl Pts',(0.674639622070907,1.07993275384806,24.6512853986972));
#15325=CARTESIAN_POINT('Ctrl Pts',(0.706479146451478,1.19143196677092,24.6571566848042));
#15326=CARTESIAN_POINT('Ctrl Pts',(0.743287362771263,1.30163939346209,24.6630279709112));
#15327=CARTESIAN_POINT('Ctrl Pts',(0.784936274317255,1.4100835664148,24.6688992570182));
#15328=CARTESIAN_POINT('Ctrl Pts',(0.827975706773152,1.52214833554758,24.6749665661615));
#15329=CARTESIAN_POINT('Ctrl Pts',(0.876184643187749,1.63232961045123,24.6810338753048));
#15330=CARTESIAN_POINT('Ctrl Pts',(0.929365697162591,1.74012371451801,24.687101184448));
#15331=CARTESIAN_POINT('Ctrl Pts',(0.980768027523406,1.84431247600458,24.6929655629376));
#15332=CARTESIAN_POINT('Ctrl Pts',(1.03681499186309,1.94627080252259,24.6988299414272));
#15333=CARTESIAN_POINT('Ctrl Pts',(1.09727972431754,2.04556488445748,24.7046943199168));
#15334=CARTESIAN_POINT('Ctrl Pts',(1.15773454406417,2.14484268792421,24.7105577369886));
#15335=CARTESIAN_POINT('Ctrl Pts',(1.22260547769648,2.24145676411002,24.7164211540604));
#15336=CARTESIAN_POINT('Ctrl Pts',(1.29162073274145,2.33499973723795,24.7222845711322));
#15337=CARTESIAN_POINT('Ctrl Pts',(1.36064119517317,2.42854976843497,24.7281484306146));
#15338=CARTESIAN_POINT('Ctrl Pts',(1.43380635628817,2.5190279048759,24.734012290097));
#15339=CARTESIAN_POINT('Ctrl Pts',(1.51080271943892,2.60605804574618,24.7398761495794));
#15340=CARTESIAN_POINT('Ctrl Pts',(1.58782332448655,2.69311558759508,24.7457418552669));
#15341=CARTESIAN_POINT('Ctrl Pts',(1.66867725772992,2.77672266712549,24.7516075609543));
#15342=CARTESIAN_POINT('Ctrl Pts',(1.75301307349878,2.85653889858912,24.7574732666418));
#15343=CARTESIAN_POINT('Ctrl Pts',(1.83744127867344,2.93644256827968,24.7633453981765));
#15344=CARTESIAN_POINT('Ctrl Pts',(1.92535868085909,3.01254681782126,24.7692175297111));
#15345=CARTESIAN_POINT('Ctrl Pts',(2.01637948944588,3.08455047974898,24.7750896612457));
#15346=CARTESIAN_POINT('Ctrl Pts',(2.10745985758375,3.15660125734012,24.7809656352151));
#15347=CARTESIAN_POINT('Ctrl Pts',(2.20164734338103,3.22454586344089,24.7868416091845));
#15348=CARTESIAN_POINT('Ctrl Pts',(2.29852722361588,3.28812649259583,24.7927175831539));
#15349=CARTESIAN_POINT('Ctrl Pts',(2.3955445661498,3.351797335936,24.7986018945086));
#15350=CARTESIAN_POINT('Ctrl Pts',(2.49526157526195,3.41109163450781,24.8044862058633));
#15351=CARTESIAN_POINT('Ctrl Pts',(2.59723896199172,3.46579749419948,24.810370517218));
#15352=CARTESIAN_POINT('Ctrl Pts',(2.62117892165194,3.47864010682366,24.811751903631));
#15353=CARTESIAN_POINT('Ctrl Pts',(2.64524336845189,3.49123005542841,24.813133290044));
#15354=CARTESIAN_POINT('Ctrl Pts',(2.6694264723439,3.50356498793949,24.814514676457));
#15355=CARTESIAN_POINT('Ctrl Pts',(2.77135311732336,3.55555410780257,24.8203369266993));
#15356=CARTESIAN_POINT('Ctrl Pts',(2.87573214684329,3.60318416315759,24.8261591769416));
#15357=CARTESIAN_POINT('Ctrl Pts',(2.98215070061731,3.64621368530512,24.831981427184));
#15358=CARTESIAN_POINT('Ctrl Pts',(3.08843356897375,3.68918834409966,24.8377962539609));
#15359=CARTESIAN_POINT('Ctrl Pts',(3.19675040535977,3.72757397422257,24.8436110807378));
#15360=CARTESIAN_POINT('Ctrl Pts',(3.30666363734902,3.76117486747937,24.8494259075147));
#15361=CARTESIAN_POINT('Ctrl Pts',(3.41646738191227,3.79474229001342,24.8552349419915));
#15362=CARTESIAN_POINT('Ctrl Pts',(3.527863959767,3.82353433053595,24.8610439764684));
#15363=CARTESIAN_POINT('Ctrl Pts',(3.64039641461402,3.84740358709843,24.8668530109453));
#15364=CARTESIAN_POINT('Ctrl Pts',(3.75285104990077,3.87125633735566,24.8726580283009));
#15365=CARTESIAN_POINT('Ctrl Pts',(3.86643958958456,3.89019298622537,24.8784630456566));
#15366=CARTESIAN_POINT('Ctrl Pts',(3.98069124466208,3.90411634386747,24.8842680630123));
#15367=CARTESIAN_POINT('Ctrl Pts',(4.094902305717,3.91803475449069,24.8900710178245));
#15368=CARTESIAN_POINT('Ctrl Pts',(4.20977559646827,3.92694336304545,24.8958739726367));
#15369=CARTESIAN_POINT('Ctrl Pts',(4.32483218276851,3.93079644860742,24.9016769274489));
#15370=CARTESIAN_POINT('Ctrl Pts',(4.43987691797427,3.93464913729267,24.9074792845434));
#15371=CARTESIAN_POINT('Ctrl Pts',(4.55510449040278,3.93344732449005,24.9132816416378));
#15372=CARTESIAN_POINT('Ctrl Pts',(4.67003373631365,3.9271973656505,24.9190839987322));
#15373=CARTESIAN_POINT('Ctrl Pts',(4.78498014188058,3.92094647365297,24.9248872221549));
#15374=CARTESIAN_POINT('Ctrl Pts',(4.89962771203976,3.90964596129763,24.9306904455776));
#15375=CARTESIAN_POINT('Ctrl Pts',(5.01349899973073,3.89335417060065,24.9364936690003));
#15376=CARTESIAN_POINT('Ctrl Pts',(5.12748189437155,3.87704641207628,24.9423025802489));
#15377=CARTESIAN_POINT('Ctrl Pts',(5.2406865700215,3.85573766745363,24.9481114914976));
#15378=CARTESIAN_POINT('Ctrl Pts',(5.35264438188033,3.82953768427627,24.9539204027462));
#15379=CARTESIAN_POINT('Ctrl Pts',(5.46466153009208,3.80332381540909,24.959732392651));
#15380=CARTESIAN_POINT('Ctrl Pts',(5.5754300937844,3.77221366046194,24.9655443825558));
#15381=CARTESIAN_POINT('Ctrl Pts',(5.68449700357783,3.73636674903664,24.9713563724606));
#15382=CARTESIAN_POINT('Ctrl Pts',(5.79372777102106,3.70046598268257,24.9771770940606));
#15383=CARTESIAN_POINT('Ctrl Pts',(5.90125138639329,3.659814398766,24.9829978156605));
#15384=CARTESIAN_POINT('Ctrl Pts',(6.00663497107806,3.61461959152322,24.9888185372605));
#15385=CARTESIAN_POINT('Ctrl Pts',(6.07371407983929,3.58585204295718,24.992523562274));
#15386=CARTESIAN_POINT('Ctrl Pts',(6.13992659654999,3.55524469959169,24.9962285872875));
#15387=CARTESIAN_POINT('Ctrl Pts',(6.2051666064271,3.52286049294652,24.999933612301));
#15388=CARTESIAN_POINT('',(8.38711649681319,0.000995139969927731,22.720836447585));
#15389=CARTESIAN_POINT('Ctrl Pts',(8.38324944744337,0.000993557744290128,
22.7208364779651));
#15390=CARTESIAN_POINT('Ctrl Pts',(8.38162681228849,-0.716766452668138,
22.7570088194235));
#15391=CARTESIAN_POINT('Ctrl Pts',(7.84956874665837,-2.74980322918279,22.8593532000194));
#15392=CARTESIAN_POINT('Ctrl Pts',(4.5842072224326,-4.64729231912613,23.027869619752));
#15393=CARTESIAN_POINT('Ctrl Pts',(0.620554861050964,-2.6266912297477,23.2263857371638));
#15394=CARTESIAN_POINT('Ctrl Pts',(0.169765939565332,1.79941472931466,23.4249018545754));
#15395=CARTESIAN_POINT('Ctrl Pts',(3.6446464547419,4.57759142130336,23.6234179719871));
#15396=CARTESIAN_POINT('Ctrl Pts',(7.51158011891165,3.28158979616131,23.8053961797836));
#15397=CARTESIAN_POINT('Ctrl Pts',(8.37991817647902,0.977746425416355,23.9212023484429));
#15398=CARTESIAN_POINT('Ctrl Pts',(8.3887972543666,-0.00363417106214093,
23.9708364779651));
#15399=CARTESIAN_POINT('',(8.38946788667635,0.00309724314203014,21.4708364780002));
#15400=CARTESIAN_POINT('Ctrl Pts',(8.38946788667635,0.00309724314205896,
21.4708364780002));
#15401=CARTESIAN_POINT('Ctrl Pts',(8.38955759207542,-0.110814131887231,
21.4766158527956));
#15402=CARTESIAN_POINT('Ctrl Pts',(8.38469430172365,-0.224907558527928,
21.482395227591));
#15403=CARTESIAN_POINT('Ctrl Pts',(8.37485717235591,-0.338709260502223,
21.4881746023863));
#15404=CARTESIAN_POINT('Ctrl Pts',(8.36503009874381,-0.452394631577112,
21.4939480693626));
#15405=CARTESIAN_POINT('Ctrl Pts',(8.35023932928709,-0.565788448603539,
21.4997215363389));
#15406=CARTESIAN_POINT('Ctrl Pts',(8.33051606647788,-0.678416649046213,
21.5054950033152));
#15407=CARTESIAN_POINT('Ctrl Pts',(8.31080678309884,-0.790965021010322,
21.5112643781806));
#15408=CARTESIAN_POINT('Ctrl Pts',(8.28617202958311,-0.902748436502693,
21.517033753046));
#15409=CARTESIAN_POINT('Ctrl Pts',(8.25669478176716,-1.0132984826293,21.5228031279114));
#15410=CARTESIAN_POINT('Ctrl Pts',(8.22722829330747,-1.12380817738598,21.5285703969235));
#15411=CARTESIAN_POINT('Ctrl Pts',(8.19292293181746,-1.23308498557155,21.5343376659356));
#15412=CARTESIAN_POINT('Ctrl Pts',(8.15391250301967,-1.34067196862229,21.5401049349477));
#15413=CARTESIAN_POINT('Ctrl Pts',(8.11490622651922,-1.44824750003928,21.5458715900876));
#15414=CARTESIAN_POINT('Ctrl Pts',(8.07119602371571,-1.55413316295026,21.5516382452276));
#15415=CARTESIAN_POINT('Ctrl Pts',(8.02296488132278,-1.65788928646081,21.5574049003675));
#15416=CARTESIAN_POINT('Ctrl Pts',(7.97472640111752,-1.76166119526951,21.5631724328376));
#15417=CARTESIAN_POINT('Ctrl Pts',(7.92196579535307,-1.86330253458784,21.5689399653076));
#15418=CARTESIAN_POINT('Ctrl Pts',(7.86491290666649,-1.96239645820766,21.5747074977777));
#15419=CARTESIAN_POINT('Ctrl Pts',(7.80780235561602,-2.06159053433534,21.5804808593927));
#15420=CARTESIAN_POINT('Ctrl Pts',(7.7463910740646,-2.15823168457841,21.5862542210076));
#15421=CARTESIAN_POINT('Ctrl Pts',(7.68095329816581,-2.2519304376202,21.5920275826226));
#15422=CARTESIAN_POINT('Ctrl Pts',(7.61548004606714,-2.34567998816611,21.597804074187));
#15423=CARTESIAN_POINT('Ctrl Pts',(7.54597621438161,-2.43648362868273,21.6035805657515));
#15424=CARTESIAN_POINT('Ctrl Pts',(7.47275633226652,-2.52398501778002,21.6093570573159));
#15425=CARTESIAN_POINT('Ctrl Pts',(7.39942243936746,-2.61162265541639,21.6151425434637));
#15426=CARTESIAN_POINT('Ctrl Pts',(7.32236123103663,-2.6959474614805,21.6209280296114));
#15427=CARTESIAN_POINT('Ctrl Pts',(7.24192417901073,-2.77663988256573,21.6267135157592));
#15428=CARTESIAN_POINT('Ctrl Pts',(7.18842780549793,-2.83030609470683,21.630561276463));
#15429=CARTESIAN_POINT('Ctrl Pts',(7.13343895539129,-2.88236643337257,21.6344090371668));
#15430=CARTESIAN_POINT('Ctrl Pts',(7.07706859112929,-2.9327371753507,21.6382567978706));
#15431=CARTESIAN_POINT('Ctrl Pts',(6.99101801832057,-3.00962919577249,21.6441304872981));
#15432=CARTESIAN_POINT('Ctrl Pts',(6.90143708305444,-3.08285880543593,21.6500041767256));
#15433=CARTESIAN_POINT('Ctrl Pts',(6.80867061650115,-3.15208455708644,21.6558778661532));
#15434=CARTESIAN_POINT('Ctrl Pts',(6.71602392022475,-3.22122093174814,21.6617439720924));
#15435=CARTESIAN_POINT('Ctrl Pts',(6.62020019980454,-3.28636348372526,21.6676100780317));
#15436=CARTESIAN_POINT('Ctrl Pts',(6.52157959640588,-3.34720893631052,21.673476183971));
#15437=CARTESIAN_POINT('Ctrl Pts',(6.42305997930556,-3.40799208389239,21.6793362830892));
#15438=CARTESIAN_POINT('Ctrl Pts',(6.32174952542897,-3.46448666875841,21.6851963822073));
#15439=CARTESIAN_POINT('Ctrl Pts',(6.21805924531874,-3.51643131339486,21.6910564813255));
#15440=CARTESIAN_POINT('Ctrl Pts',(6.1106280572322,-3.570250001917,21.697127999407));
#15441=CARTESIAN_POINT('Ctrl Pts',(6.00064244543429,-3.61918397870955,21.7031995174885));
#15442=CARTESIAN_POINT('Ctrl Pts',(5.88859007690819,-3.66299311019146,21.7092710355701));
#15443=CARTESIAN_POINT('Ctrl Pts',(5.78056383891217,-3.70522814481066,21.7151243991883));
#15444=CARTESIAN_POINT('Ctrl Pts',(5.670617226365,-3.74270011227689,21.7209777628066));
#15445=CARTESIAN_POINT('Ctrl Pts',(5.5592089701512,-3.77524221640057,21.7268311264249));
#15446=CARTESIAN_POINT('Ctrl Pts',(5.44781744157284,-3.8077794344191,21.7326836111771));
#15447=CARTESIAN_POINT('Ctrl Pts',(5.33496510216676,-3.83538814509375,21.7385360959294));
#15448=CARTESIAN_POINT('Ctrl Pts',(5.2211260094527,-3.85795137609792,21.7443885806816));
#15449=CARTESIAN_POINT('Ctrl Pts',(5.10727647928484,-3.88051667583503,21.7502416020249));
#15450=CARTESIAN_POINT('Ctrl Pts',(4.99244042124382,-3.89803549596782,21.7560946233682));
#15451=CARTESIAN_POINT('Ctrl Pts',(4.87710155199393,-3.91044209080773,21.7619476447115));
#15452=CARTESIAN_POINT('Ctrl Pts',(4.76172421506629,-3.92285282347988,21.7678026181473));
#15453=CARTESIAN_POINT('Ctrl Pts',(4.64584414402544,-3.93014789633503,21.773657591583));
#15454=CARTESIAN_POINT('Ctrl Pts',(4.52994892396885,-3.93231353230936,21.7795125650188));
#15455=CARTESIAN_POINT('Ctrl Pts',(4.4139223516613,-3.93448162275213,21.7853741743101));
#15456=CARTESIAN_POINT('Ctrl Pts',(4.29788100937271,-3.93150866508802,21.7912357836015));
#15457=CARTESIAN_POINT('Ctrl Pts',(4.18231132576629,-3.92343300075554,21.7970973928928));
#15458=CARTESIAN_POINT('Ctrl Pts',(4.06666371272803,-3.91535189094711,21.8029629547076));
#15459=CARTESIAN_POINT('Ctrl Pts',(3.95148880111156,-3.90216126998636,21.8088285165223));
#15460=CARTESIAN_POINT('Ctrl Pts',(3.8372650238806,-3.88395099150547,21.8146940783371));
#15461=CARTESIAN_POINT('Ctrl Pts',(3.72287422355083,-3.86571408514363,21.8205682170378));
#15462=CARTESIAN_POINT('Ctrl Pts',(3.60943773643655,-3.84244295523982,21.8264423557385));
#15463=CARTESIAN_POINT('Ctrl Pts',(3.4974210636286,-3.81427789391451,21.8323164944392));
#15464=CARTESIAN_POINT('Ctrl Pts',(3.4690938789469,-3.80715541050437,21.8338019680535));
#15465=CARTESIAN_POINT('Ctrl Pts',(3.44085740010028,-3.79972020312893,21.8352874416679));
#15466=CARTESIAN_POINT('Ctrl Pts',(3.412718957351,-3.79197502981488,21.8367729152822));
#15467=CARTESIAN_POINT('Ctrl Pts',(3.30145712738501,-3.76134994640131,21.8426466060962));
#15468=CARTESIAN_POINT('Ctrl Pts',(3.19135900814053,-3.72577284172737,21.8485202969102));
#15469=CARTESIAN_POINT('Ctrl Pts',(3.08289845684532,-3.68534837853644,21.8543939877241));
#15470=CARTESIAN_POINT('Ctrl Pts',(2.97457793816869,-3.64497610707206,21.8602600950592));
#15471=CARTESIAN_POINT('Ctrl Pts',(2.86789116648166,-3.59976906594414,21.8661262023942));
#15472=CARTESIAN_POINT('Ctrl Pts',(2.76329906586566,-3.54988228177392,21.8719923097293));
#15473=CARTESIAN_POINT('Ctrl Pts',(2.65881406612829,-3.50004658098748,21.8778524102508));
#15474=CARTESIAN_POINT('Ctrl Pts',(2.5564198417327,-3.44554084563276,21.8837125107722));
#15475=CARTESIAN_POINT('Ctrl Pts',(2.45655884310556,-3.38656875605627,21.8895726112937));
#15476=CARTESIAN_POINT('Ctrl Pts',(2.3530951219056,-3.32546910836195,21.8956441288521));
#15477=CARTESIAN_POINT('Ctrl Pts',(2.25235128499276,-3.25957491100247,21.9017156464104));
#15478=CARTESIAN_POINT('Ctrl Pts',(2.15479348708341,-3.18916577560343,21.9077871639687));
#15479=CARTESIAN_POINT('Ctrl Pts',(2.06074098746527,-3.1212864740802,21.9136405290003));
#15480=CARTESIAN_POINT('Ctrl Pts',(1.96964987895512,-3.04921136114959,21.9194938940318));
#15481=CARTESIAN_POINT('Ctrl Pts',(1.88190900418916,-2.9732354903438,21.9253472590634));
#15482=CARTESIAN_POINT('Ctrl Pts',(1.79418130344622,-2.89727102708179,21.9311997452301));
#15483=CARTESIAN_POINT('Ctrl Pts',(1.70980314848196,-2.81740724088383,21.9370522313969));
#15484=CARTESIAN_POINT('Ctrl Pts',(1.62912982325913,-2.7339790743596,21.9429047175636));
#15485=CARTESIAN_POINT('Ctrl Pts',(1.54844910142523,-2.65054325864404,21.9487577403212));
#15486=CARTESIAN_POINT('Ctrl Pts',(1.47147417179507,-2.5635427099633,21.9546107630787));
#15487=CARTESIAN_POINT('Ctrl Pts',(1.39852250849697,-2.47334825802693,21.9604637858363));
#15488=CARTESIAN_POINT('Ctrl Pts',(1.32554651447847,-2.38312372458325,21.9663187606845));
#15489=CARTESIAN_POINT('Ctrl Pts',(1.256596714642,-2.28970349078143,21.9721737355327));
#15490=CARTESIAN_POINT('Ctrl Pts',(1.19194901058673,-2.19348980969093,21.9780287103809));
#15491=CARTESIAN_POINT('Ctrl Pts',(1.12722803684081,-2.09716708301633,21.9838903210749));
#15492=CARTESIAN_POINT('Ctrl Pts',(1.06681912134687,-1.99804493301132,21.9897519317689));
#15493=CARTESIAN_POINT('Ctrl Pts',(1.01095374320409,-1.89655289492104,21.995613542463));
#15494=CARTESIAN_POINT('Ctrl Pts',(0.955050694700068,-1.79499242013768,
22.0014791056764));
#15495=CARTESIAN_POINT('Ctrl Pts',(0.903697466682843,-1.69105924471863,
22.0073446688898));
#15496=CARTESIAN_POINT('Ctrl Pts',(0.857077917608687,-1.58520411031508,
22.0132102321033));
#15497=CARTESIAN_POINT('Ctrl Pts',(0.81039019950015,-1.47919419015233,22.019084372186));
#15498=CARTESIAN_POINT('Ctrl Pts',(0.768450123527769,-1.3712570858322,22.0249585122688));
#15499=CARTESIAN_POINT('Ctrl Pts',(0.731392153800996,-1.2618600154414,22.0308326523516));
#15500=CARTESIAN_POINT('Ctrl Pts',(0.722020886660144,-1.23419554330174,
22.0323181124657));
#15501=CARTESIAN_POINT('Ctrl Pts',(0.712961570755281,-1.20643776306536,
22.0338035725798));
#15502=CARTESIAN_POINT('Ctrl Pts',(0.704215862256281,-1.17859432935038,
22.0352890326939));
#15503=CARTESIAN_POINT('Ctrl Pts',(0.669634288741553,-1.06849807470993,
22.0411627189875));
#15504=CARTESIAN_POINT('Ctrl Pts',(0.63984478843726,-0.956695158277188,
22.0470364052811));
#15505=CARTESIAN_POINT('Ctrl Pts',(0.615016295092537,-0.84364050394368,
22.0529100915748));
#15506=CARTESIAN_POINT('Ctrl Pts',(0.590219857680636,-0.730731813859958,
22.058776194384));
#15507=CARTESIAN_POINT('Ctrl Pts',(0.570371777338458,-0.616574999635444,
22.0646422971931));
#15508=CARTESIAN_POINT('Ctrl Pts',(0.555591655487483,-0.501641420120213,
22.0705084000023));
#15509=CARTESIAN_POINT('Ctrl Pts',(0.54082666829106,-0.386825531111181,
22.0763684959977));
#15510=CARTESIAN_POINT('Ctrl Pts',(0.531119369574364,-0.271234866258815,
22.0822285919931));
#15511=CARTESIAN_POINT('Ctrl Pts',(0.526538461916261,-0.155351636541585,
22.0880886879886));
#15512=CARTESIAN_POINT('Ctrl Pts',(0.521792282148428,-0.0352875179510033,
22.0941602072434));
#15513=CARTESIAN_POINT('Ctrl Pts',(0.522549479060774,0.0850902335095483,
22.1002317264983));
#15514=CARTESIAN_POINT('Ctrl Pts',(0.528827799952726,0.205238323216817,
22.1063032457532));
#15515=CARTESIAN_POINT('Ctrl Pts',(0.53488053143222,0.321069313267738,22.1121566062861));
#15516=CARTESIAN_POINT('Ctrl Pts',(0.54606442746512,0.436686413749744,22.1180099668191));
#15517=CARTESIAN_POINT('Ctrl Pts',(0.562342347678128,0.551602926407942,
22.1238633273521));
#15518=CARTESIAN_POINT('Ctrl Pts',(0.578617823858808,0.666502185039311,
22.129715809038));
#15519=CARTESIAN_POINT('Ctrl Pts',(0.599985745507873,0.780700656050129,
22.1355682907239));
#15520=CARTESIAN_POINT('Ctrl Pts',(0.626357260670107,0.893718216549156,
22.1414207724098));
#15521=CARTESIAN_POINT('Ctrl Pts',(0.652731193832982,1.00674613961294,22.147273790709));
#15522=CARTESIAN_POINT('Ctrl Pts',(0.684109538631827,1.11859253455979,22.1531268090082));
#15523=CARTESIAN_POINT('Ctrl Pts',(0.720352789829755,1.22878959566545,22.1589798273073));
#15524=CARTESIAN_POINT('Ctrl Pts',(0.756608128995365,1.33902341005536,22.1648347977243));
#15525=CARTESIAN_POINT('Ctrl Pts',(0.79773147193756,1.44760640452048,22.1706897681413));
#15526=CARTESIAN_POINT('Ctrl Pts',(0.843534371264841,1.55408867217001,22.1765447385583));
#15527=CARTESIAN_POINT('Ctrl Pts',(0.889389182695605,1.6606916247233,22.1824063448833));
#15528=CARTESIAN_POINT('Ctrl Pts',(0.939933973069185,1.76518871854719,22.1882679512084));
#15529=CARTESIAN_POINT('Ctrl Pts',(0.994933287714969,1.86715258541418,22.1941295575334));
#15530=CARTESIAN_POINT('Ctrl Pts',(1.04996968904864,1.96918520772168,22.1999951164089));
#15531=CARTESIAN_POINT('Ctrl Pts',(1.10946638425299,2.06868084799046,22.2058606752844));
#15532=CARTESIAN_POINT('Ctrl Pts',(1.17314428316303,2.16524065782753,22.2117262341599));
#15533=CARTESIAN_POINT('Ctrl Pts',(1.23691529545404,2.26194166281259,22.2176003699832));
#15534=CARTESIAN_POINT('Ctrl Pts',(1.30487947188746,2.35569793653009,22.2234745058065));
#15535=CARTESIAN_POINT('Ctrl Pts',(1.37671709989604,2.44614320503816,22.2293486416299));
#15536=CARTESIAN_POINT('Ctrl Pts',(1.39488402735091,2.46901579531113,22.2308341444551));
#15537=CARTESIAN_POINT('Ctrl Pts',(1.41329848829932,2.49167682159717,22.2323196472803));
#15538=CARTESIAN_POINT('Ctrl Pts',(1.43195494784296,2.51412074208607,22.2338051501055));
#15539=CARTESIAN_POINT('Ctrl Pts',(1.50572274489267,2.60286419138592,22.2396788406988));
#15540=CARTESIAN_POINT('Ctrl Pts',(1.58352249613533,2.6885060166343,22.2455525312921));
#15541=CARTESIAN_POINT('Ctrl Pts',(1.66506350554639,2.77065764260722,22.2514262218855));
#15542=CARTESIAN_POINT('Ctrl Pts',(1.74649923756383,2.852703202821,22.2572923289715));
#15543=CARTESIAN_POINT('Ctrl Pts',(1.83166633342138,2.93126723454188,22.2631584360576));
#15544=CARTESIAN_POINT('Ctrl Pts',(1.9202335431614,3.00599370735964,22.2690245431437));
#15545=CARTESIAN_POINT('Ctrl Pts',(2.00871006087096,3.08064366093772,22.2748846433886));
#15546=CARTESIAN_POINT('Ctrl Pts',(2.10057945321058,3.15146360712732,22.2807447436334));
#15547=CARTESIAN_POINT('Ctrl Pts',(2.1954737583591,3.21813440318444,22.2866048438783));
#15548=CARTESIAN_POINT('Ctrl Pts',(2.29379160697434,3.28721051079219,22.2926763615299));
#15549=CARTESIAN_POINT('Ctrl Pts',(2.39535643328392,3.35183211386048,22.2987478791816));
#15550=CARTESIAN_POINT('Ctrl Pts',(2.49972132434884,3.41168977460571,22.3048193968332));
#15551=CARTESIAN_POINT('Ctrl Pts',(2.60033632757285,3.46939671673357,22.3106727615218));
#15552=CARTESIAN_POINT('Ctrl Pts',(2.70355325358029,3.52267594388975,22.3165261262104));
#15553=CARTESIAN_POINT('Ctrl Pts',(2.80894299142305,3.57129482135931,22.3223794908991));
#15554=CARTESIAN_POINT('Ctrl Pts',(2.91431690489155,3.61990639865594,22.3282319766991));
#15555=CARTESIAN_POINT('Ctrl Pts',(3.02186260643961,3.66385884462494,22.3340844624992));
#15556=CARTESIAN_POINT('Ctrl Pts',(3.13112847709521,3.70296654275944,22.3399369482993));
#15557=CARTESIAN_POINT('Ctrl Pts',(3.2404043654636,3.74207782636564,22.345789970667));
#15558=CARTESIAN_POINT('Ctrl Pts',(3.35140034744718,3.77634333992773,22.3516429930346));
#15559=CARTESIAN_POINT('Ctrl Pts',(3.46364769463818,3.80562670853411,22.3574960154022));
#15560=CARTESIAN_POINT('Ctrl Pts',(3.57593247794847,3.8349198435689,22.3633509898378));
#15561=CARTESIAN_POINT('Ctrl Pts',(3.68946905679595,3.85922742536008,22.3692059642733));
#15562=CARTESIAN_POINT('Ctrl Pts',(3.8037772112643,3.87846390859338,22.3750609387089));
#15563=CARTESIAN_POINT('Ctrl Pts',(3.91821491842669,3.89772219375533,22.3809225489589));
#15564=CARTESIAN_POINT('Ctrl Pts',(4.03342553896684,3.91189784029784,22.386784159209));
#15565=CARTESIAN_POINT('Ctrl Pts',(4.14892230926012,3.92095702191198,22.3926457694591));
#15566=CARTESIAN_POINT('Ctrl Pts',(4.2644969593582,3.93002231215836,22.3985113322098));
#15567=CARTESIAN_POINT('Ctrl Pts',(4.38035773153477,3.93396425365368,22.4043768949606));
#15568=CARTESIAN_POINT('Ctrl Pts',(4.49601817233813,3.93280114821091,22.4102424577113));
#15569=CARTESIAN_POINT('Ctrl Pts',(4.61184773617339,3.93163634203178,22.4161165973078));
#15570=CARTESIAN_POINT('Ctrl Pts',(4.72747597306673,3.92535161340455,22.4219907369042));
#15571=CARTESIAN_POINT('Ctrl Pts',(4.84242178029476,3.91401705839068,22.4278648765007));
#15572=CARTESIAN_POINT('Ctrl Pts',(4.87148949618726,3.91115075440921,22.4293503401729));
#15573=CARTESIAN_POINT('Ctrl Pts',(4.90051362575562,3.90796177220534,22.430835803845));
#15574=CARTESIAN_POINT('Ctrl Pts',(4.92948651226061,3.90445175838824,22.4323212675171));
#15575=CARTESIAN_POINT('Ctrl Pts',(5.04404871734446,3.89057275041667,22.4381949658048));
#15576=CARTESIAN_POINT('Ctrl Pts',(5.15819035855018,3.87162422586959,22.4440686640925));
#15577=CARTESIAN_POINT('Ctrl Pts',(5.27142732289849,3.84763980968403,22.4499423623801));
#15578=CARTESIAN_POINT('Ctrl Pts',(5.38451808878241,3.82368635940114,22.4558084772283));
#15579=CARTESIAN_POINT('Ctrl Pts',(5.49670610012062,3.79471003217636,22.4616745920764));
#15580=CARTESIAN_POINT('Ctrl Pts',(5.60751260704967,3.76079617357732,22.4675407069246));
#15581=CARTESIAN_POINT('Ctrl Pts',(5.71820565034903,3.72691704208592,22.4734008149894));
#15582=CARTESIAN_POINT('Ctrl Pts',(5.82751961035471,3.68811055608318,22.4792609230542));
#15583=CARTESIAN_POINT('Ctrl Pts',(5.93498683245613,3.64451290753654,22.4851210311189));
#15584=CARTESIAN_POINT('Ctrl Pts',(6.04633099472505,3.59934244942476,22.491192545861));
#15585=CARTESIAN_POINT('Ctrl Pts',(6.15569221744842,3.54902870825381,22.4972640606031));
#15586=CARTESIAN_POINT('Ctrl Pts',(6.26256820374707,3.49377947928967,22.5033355753452));
#15587=CARTESIAN_POINT('Ctrl Pts',(6.36560426585618,3.44051528792004,22.5091889479476));
#15588=CARTESIAN_POINT('Ctrl Pts',(6.46633020291411,3.38266436374306,22.5150423205501));
#15589=CARTESIAN_POINT('Ctrl Pts',(6.56431790427514,3.32046117949453,22.5208956931525));
#15590=CARTESIAN_POINT('Ctrl Pts',(6.66229089305707,3.25826733488,22.5267481868875));
#15591=CARTESIAN_POINT('Ctrl Pts',(6.7575261149343,3.19172275091743,22.5326006806224));
#15592=CARTESIAN_POINT('Ctrl Pts',(6.84962276725822,3.12110630300396,22.5384531743574));
#15593=CARTESIAN_POINT('Ctrl Pts',(6.94172786337115,3.05048338069242,22.5443062046723));
#15594=CARTESIAN_POINT('Ctrl Pts',(7.03069349002169,2.97578810369883,22.5501592349873));
#15595=CARTESIAN_POINT('Ctrl Pts',(7.11615094749728,2.89734041893089,22.5560122653022));
#15596=CARTESIAN_POINT('Ctrl Pts',(7.20163690629269,2.8188665707055,22.5618672476889));
#15597=CARTESIAN_POINT('Ctrl Pts',(7.28361206518037,2.73663810542358,22.5677222300757));
#15598=CARTESIAN_POINT('Ctrl Pts',(7.36174420731161,2.65101218159536,22.5735772124624));
#15599=CARTESIAN_POINT('Ctrl Pts',(7.43996490098065,2.56528921310634,22.5794388306289));
#15600=CARTESIAN_POINT('Ctrl Pts',(7.51433360593221,2.47616140600076,22.5853004487955));
#15601=CARTESIAN_POINT('Ctrl Pts',(7.58455801779941,2.3840194548793,22.591162066962));
#15602=CARTESIAN_POINT('Ctrl Pts',(7.65482978199884,2.29181537242536,22.5970276376186));
#15603=CARTESIAN_POINT('Ctrl Pts',(7.72095145358791,2.19659343743236,22.6028932082753));
#15604=CARTESIAN_POINT('Ctrl Pts',(7.78267470000588,2.0987723430272,22.6087587789319));
#15605=CARTESIAN_POINT('Ctrl Pts',(7.84448819954077,2.00080821242122,22.6146329263576));
#15606=CARTESIAN_POINT('Ctrl Pts',(7.90189023428523,1.90023769489433,22.6205070737834));
#15607=CARTESIAN_POINT('Ctrl Pts',(7.95467889546119,1.7975030654897,22.6263812212091));
#15608=CARTESIAN_POINT('Ctrl Pts',(7.96802749453962,1.77152469534649,22.6278666091157));
#15609=CARTESIAN_POINT('Ctrl Pts',(7.98108134602636,1.74540803842346,22.6293519970222));
#15610=CARTESIAN_POINT('Ctrl Pts',(7.99383768320666,1.71916042024444,22.6308373849288));
#15611=CARTESIAN_POINT('Ctrl Pts',(8.04811447871309,1.60747972504976,22.6371575452156));
#15612=CARTESIAN_POINT('Ctrl Pts',(8.09716102928467,1.49309802179009,22.6434777055024));
#15613=CARTESIAN_POINT('Ctrl Pts',(8.14072086865502,1.3765093355955,22.6497978657891));
#15614=CARTESIAN_POINT('Ctrl Pts',(8.18413881155106,1.26030043784261,22.6560974381106));
#15615=CARTESIAN_POINT('Ctrl Pts',(8.22210557102849,1.14189918600747,22.6623970104321));
#15616=CARTESIAN_POINT('Ctrl Pts',(8.25441234767607,1.02182001089472,22.6686965827536));
#15617=CARTESIAN_POINT('Ctrl Pts',(8.28665456255747,0.901980801647662,22.6749835660285));
#15618=CARTESIAN_POINT('Ctrl Pts',(8.31325924883263,0.780470651645069,22.6812705493034));
#15619=CARTESIAN_POINT('Ctrl Pts',(8.33406621362973,0.657821915562379,22.6875575325783));
#15620=CARTESIAN_POINT('Ctrl Pts',(8.3548100386261,0.535545363353235,22.6938254376804));
#15621=CARTESIAN_POINT('Ctrl Pts',(8.36979116524708,0.412137422350944,22.7000933427825));
#15622=CARTESIAN_POINT('Ctrl Pts',(8.37889986957347,0.288142164017332,22.7063612478845));
#15623=CARTESIAN_POINT('Ctrl Pts',(8.3859117894865,0.192690078860521,22.7111863082908));
#15624=CARTESIAN_POINT('Ctrl Pts',(8.38944469315269,0.0968903237123851,
22.7160113686972));
#15625=CARTESIAN_POINT('Ctrl Pts',(8.38946898007787,0.000996102502074969,
22.7208364291035));
#15626=CARTESIAN_POINT('',(8.39049475251801,-0.00287584216518763,20.2208360257257));
#15627=CARTESIAN_POINT('Ctrl Pts',(8.38946804882023,-0.00288400618541905,
20.2208364779651));
#15628=CARTESIAN_POINT('Ctrl Pts',(8.38933415447296,-0.185479428099694,
20.230105643973));
#15629=CARTESIAN_POINT('Ctrl Pts',(8.37648338631382,-0.367615513710913,
20.239374809981));
#15630=CARTESIAN_POINT('Ctrl Pts',(8.35111160572364,-0.547949633676686,
20.248643975989));
#15631=CARTESIAN_POINT('Ctrl Pts',(8.33503400411599,-0.66222384185733,20.2545176653732));
#15632=CARTESIAN_POINT('Ctrl Pts',(8.31389591767628,-0.77598016486602,20.2603913547574));
#15633=CARTESIAN_POINT('Ctrl Pts',(8.28774026569583,-0.888735226349951,
20.2662650441417));
#15634=CARTESIAN_POINT('Ctrl Pts',(8.26161838311929,-1.0013447104567,20.2721311500411));
#15635=CARTESIAN_POINT('Ctrl Pts',(8.23049191042047,-1.11295510505729,20.2779972559405));
#15636=CARTESIAN_POINT('Ctrl Pts',(8.19445537494036,-1.2230893895562,20.2838633618399));
#15637=CARTESIAN_POINT('Ctrl Pts',(8.15845574041331,-1.3331108979514,20.2897234609216));
#15638=CARTESIAN_POINT('Ctrl Pts',(8.11755617161554,-1.44165891245357,20.2955835600033));
#15639=CARTESIAN_POINT('Ctrl Pts',(8.0719018197416,-1.54826848252657,20.3014436590851));
#15640=CARTESIAN_POINT('Ctrl Pts',(8.02460036293674,-1.65872428283489,20.3075151771816));
#15641=CARTESIAN_POINT('Ctrl Pts',(7.97219466407808,-1.76709868861349,20.313586695278));
#15642=CARTESIAN_POINT('Ctrl Pts',(7.91490213138158,-1.87289348614907,20.3196582133745));
#15643=CARTESIAN_POINT('Ctrl Pts',(7.85966816525232,-1.97488699191162,20.3255115769651));
#15644=CARTESIAN_POINT('Ctrl Pts',(7.79989271092155,-2.07448267950373,20.3313649405556));
#15645=CARTESIAN_POINT('Ctrl Pts',(7.73581842257439,-2.17125702331955,20.3372183041461));
#15646=CARTESIAN_POINT('Ctrl Pts',(7.67175375476552,-2.26801683679405,20.3430707888738));
#15647=CARTESIAN_POINT('Ctrl Pts',(7.60339176436818,-2.36195580440928,20.3489232736015));
#15648=CARTESIAN_POINT('Ctrl Pts',(7.53101897535869,-2.45267855663323,20.3547757583292));
#15649=CARTESIAN_POINT('Ctrl Pts',(7.45863955073542,-2.54340962691641,20.3606287796513));
#15650=CARTESIAN_POINT('Ctrl Pts',(7.38224885413203,-2.63092357262074,20.3664818009733));
#15651=CARTESIAN_POINT('Ctrl Pts',(7.3021738566419,-2.71485791035484,20.3723348222953));
#15652=CARTESIAN_POINT('Ctrl Pts',(7.22207215259273,-2.79882024181253,20.3781897957131));
#15653=CARTESIAN_POINT('Ctrl Pts',(7.13828398930198,-2.87920029257801,20.3840447691308));
#15654=CARTESIAN_POINT('Ctrl Pts',(7.05117284161667,-2.95567277037048,20.3898997425486));
#15655=CARTESIAN_POINT('Ctrl Pts',(6.96396296463272,-3.03223191989552,20.3957613518268));
#15656=CARTESIAN_POINT('Ctrl Pts',(6.87342289684813,-3.10487438424982,20.401622961105));
#15657=CARTESIAN_POINT('Ctrl Pts',(6.77994887612719,-3.17331542063248,20.4074845703832));
#15658=CARTESIAN_POINT('Ctrl Pts',(6.68641182518651,-3.2418026073094,20.4133501321876));
#15659=CARTESIAN_POINT('Ctrl Pts',(6.58993722487058,-3.30608249626153,20.4192156939921));
#15660=CARTESIAN_POINT('Ctrl Pts',(6.49094846149591,-3.36591484636034,20.4250812557965));
#15661=CARTESIAN_POINT('Ctrl Pts',(6.39181495226808,-3.42583468603137,20.4309553944911));
#15662=CARTESIAN_POINT('Ctrl Pts',(6.29016030425197,-3.48129381060674,20.4368295331857));
#15663=CARTESIAN_POINT('Ctrl Pts',(6.18643058930618,-3.53209884729069,20.4427036718803));
#15664=CARTESIAN_POINT('Ctrl Pts',(6.16019903673279,-3.54494661219069,20.4441891457203));
#15665=CARTESIAN_POINT('Ctrl Pts',(6.13383487071145,-3.55749699255338,20.4456746195604));
#15666=CARTESIAN_POINT('Ctrl Pts',(6.1073454698712,-3.56974736247987,20.4471600934005));
#15667=CARTESIAN_POINT('Ctrl Pts',(6.00260413524884,-3.61818636279764,20.4530337827864));
#15668=CARTESIAN_POINT('Ctrl Pts',(5.89555464664127,-3.66209224752305,20.4589074721724));
#15669=CARTESIAN_POINT('Ctrl Pts',(5.7866264559468,-3.70123903915474,20.4647811615584));
#15670=CARTESIAN_POINT('Ctrl Pts',(5.67783890178138,-3.74033528860021,20.4706472674595));
#15671=CARTESIAN_POINT('Ctrl Pts',(5.56717785446262,-3.77468452577001,20.4765133733605));
#15672=CARTESIAN_POINT('Ctrl Pts',(5.45509540231072,-3.80410758532834,20.4823794792616));
#15673=CARTESIAN_POINT('Ctrl Pts',(5.34312772116331,-3.83350051604816,20.4882395783449));
#15674=CARTESIAN_POINT('Ctrl Pts',(5.22974192752406,-3.85797719849521,20.4940996774282));
#15675=CARTESIAN_POINT('Ctrl Pts',(5.11540741082015,-3.87740755024905,20.4999597765115));
#15676=CARTESIAN_POINT('Ctrl Pts',(4.99694796546249,-3.89753890478851,20.5060312946074));
#15677=CARTESIAN_POINT('Ctrl Pts',(4.87747047409657,-3.9122527809085,20.5121028127033));
#15678=CARTESIAN_POINT('Ctrl Pts',(4.75751144867638,-3.92146178204599,20.5181743307991));
#15679=CARTESIAN_POINT('Ctrl Pts',(4.64186264703803,-3.93033989640301,20.524027694391));
#15680=CARTESIAN_POINT('Ctrl Pts',(4.52576676687471,-3.93410188254948,20.5298810579829));
#15681=CARTESIAN_POINT('Ctrl Pts',(4.40971124521822,-3.93272204744178,20.5357344215748));
#15682=CARTESIAN_POINT('Ctrl Pts',(4.29367314890863,-3.93134241951168,20.5415869063038));
#15683=CARTESIAN_POINT('Ctrl Pts',(4.17767581206175,-3.92482251031784,20.5474393910328));
#15684=CARTESIAN_POINT('Ctrl Pts',(4.0622067941707,-3.91318875462185,20.5532918757618));
#15685=CARTESIAN_POINT('Ctrl Pts',(3.94672718932174,-3.90155393226672,20.559144897085));
#15686=CARTESIAN_POINT('Ctrl Pts',(3.83177641080876,-3.88480437275555,20.5649979184082));
#15687=CARTESIAN_POINT('Ctrl Pts',(3.7178363104098,-3.86301832676939,20.5708509397314));
#15688=CARTESIAN_POINT('Ctrl Pts',(3.60385820878753,-3.84122501471627,20.5767059131503));
#15689=CARTESIAN_POINT('Ctrl Pts',(3.49089186112378,-3.81439195359782,20.5825608865691));
#15690=CARTESIAN_POINT('Ctrl Pts',(3.37940765624663,-3.78264823014049,20.588415859988));
#15691=CARTESIAN_POINT('Ctrl Pts',(3.26779709834318,-3.75086852925005,20.5942774692671));
#15692=CARTESIAN_POINT('Ctrl Pts',(3.15767243361623,-3.71416717061233,20.6001390785463));
#15693=CARTESIAN_POINT('Ctrl Pts',(3.04948773799101,-3.67272275423307,20.6060006878255));
#15694=CARTESIAN_POINT('Ctrl Pts',(2.94123009263126,-3.63125039157957,20.6118662496308));
#15695=CARTESIAN_POINT('Ctrl Pts',(2.83491539910909,-3.58502876701982,20.6177318114361));
#15696=CARTESIAN_POINT('Ctrl Pts',(2.73097505567941,-3.53428341839687,20.6235973732414));
#15697=CARTESIAN_POINT('Ctrl Pts',(2.62688272597427,-3.48346386762795,20.6294715119368));
#15698=CARTESIAN_POINT('Ctrl Pts',(2.52517203685204,-3.42810758806947,20.6353456506321));
#15699=CARTESIAN_POINT('Ctrl Pts',(2.42624730078802,-3.36848458817249,20.6412197893274));
#15700=CARTESIAN_POINT('Ctrl Pts',(2.40123084918291,-3.35340690436134,20.6427052631557));
#15701=CARTESIAN_POINT('Ctrl Pts',(2.37639240112385,-3.33805656944734,20.644190736984));
#15702=CARTESIAN_POINT('Ctrl Pts',(2.35173816319912,-3.32243836022548,20.6456762108123));
#15703=CARTESIAN_POINT('Ctrl Pts',(2.25425321678615,-3.26068263718476,20.651549900236));
#15704=CARTESIAN_POINT('Ctrl Pts',(2.15932621079835,-3.19452990911246,20.6574235896598));
#15705=CARTESIAN_POINT('Ctrl Pts',(2.0673798458647,-3.12421854326219,20.6632972790835));
#15706=CARTESIAN_POINT('Ctrl Pts',(1.97555219232417,-3.05399795598916,20.6691633850225));
#15707=CARTESIAN_POINT('Ctrl Pts',(1.88669785204408,-2.97962965717206,20.6750294909615));
#15708=CARTESIAN_POINT('Ctrl Pts',(1.80121246044254,-2.90139641294738,20.6808955969005));
#15709=CARTESIAN_POINT('Ctrl Pts',(1.7158146047917,-2.82324327856697,20.6867556960218));
#15710=CARTESIAN_POINT('Ctrl Pts',(1.63377913892778,-2.74123334814802,20.6926157951432));
#15711=CARTESIAN_POINT('Ctrl Pts',(1.55546983260423,-2.65569053439796,20.6984758942645));
#15712=CARTESIAN_POINT('Ctrl Pts',(1.47433530578824,-2.56706153176774,20.7045474123461));
#15713=CARTESIAN_POINT('Ctrl Pts',(1.39720123616582,-2.4746401905453,20.7106189304278));
#15714=CARTESIAN_POINT('Ctrl Pts',(1.32443191198014,-2.37882996742285,20.7166904485094));
#15715=CARTESIAN_POINT('Ctrl Pts',(1.25427724722614,-2.28646228147308,20.7225438121394));
#15716=CARTESIAN_POINT('Ctrl Pts',(1.1881793396891,-2.19094541013953,20.7283971757693));
#15717=CARTESIAN_POINT('Ctrl Pts',(1.12642402368809,-2.0926750221467,20.7342505393993));
#15718=CARTESIAN_POINT('Ctrl Pts',(1.06467798004083,-1.99441938912332,20.7401030241663));
#15719=CARTESIAN_POINT('Ctrl Pts',(1.00727345122547,-1.89341141121052,20.7459555089334));
#15720=CARTESIAN_POINT('Ctrl Pts',(0.95445253454464,-1.79007511901691,20.7518079937004));
#15721=CARTESIAN_POINT('Ctrl Pts',(0.901626774896074,-1.68672935227494,
20.7576610150616));
#15722=CARTESIAN_POINT('Ctrl Pts',(0.853385650860985,-1.58105521477579,
20.7635140364227));
#15723=CARTESIAN_POINT('Ctrl Pts',(0.809924624211627,-1.47350003079302,
20.7693670577839));
#15724=CARTESIAN_POINT('Ctrl Pts',(0.766449102471797,-1.36590897508234,
20.7752220312406));
#15725=CARTESIAN_POINT('Ctrl Pts',(0.72775700292333,-1.25643600824745,20.7810770046973));
#15726=CARTESIAN_POINT('Ctrl Pts',(0.693994855236427,-1.14554638085883,
20.7869319781539));
#15727=CARTESIAN_POINT('Ctrl Pts',(0.660194442494234,-1.0345310743291,20.7927935874705));
#15728=CARTESIAN_POINT('Ctrl Pts',(0.631335254263033,-0.922096298012428,
20.7986551967871));
#15729=CARTESIAN_POINT('Ctrl Pts',(0.60751337043616,-0.808720436238716,
20.8045168061037));
#15730=CARTESIAN_POINT('Ctrl Pts',(0.583675423338946,-0.695268124292923,
20.8103823679463));
#15731=CARTESIAN_POINT('Ctrl Pts',(0.56488161102356,-0.580873869969791,
20.8162479297889));
#15732=CARTESIAN_POINT('Ctrl Pts',(0.551176277369566,-0.466022446823152,
20.8221134916315));
#15733=CARTESIAN_POINT('Ctrl Pts',(0.537450903157662,-0.351003082737979,
20.8279876303636));
#15734=CARTESIAN_POINT('Ctrl Pts',(0.52882888782412,-0.235525626099837,
20.8338617690956));
#15735=CARTESIAN_POINT('Ctrl Pts',(0.525302522788892,-0.120076198009198,
20.8397359078277));
#15736=CARTESIAN_POINT('Ctrl Pts',(0.524410762834271,-0.0908809287371239,
20.8412213812931));
#15737=CARTESIAN_POINT('Ctrl Pts',(0.523844610997288,-0.0616874304851447,
20.8427068547585));
#15738=CARTESIAN_POINT('Ctrl Pts',(0.523603417950699,-0.0325035082383315,
20.8441923282239));
#15739=CARTESIAN_POINT('Ctrl Pts',(0.522649719982162,0.0828922204297335,
20.8500660175624));
#15740=CARTESIAN_POINT('Ctrl Pts',(0.526777543537242,0.198522149960062,
20.8559397069009));
#15741=CARTESIAN_POINT('Ctrl Pts',(0.536015736779851,0.313901860553742,
20.8618133962393));
#15742=CARTESIAN_POINT('Ctrl Pts',(0.545242002647123,0.429132605101971,
20.8676795020931));
#15743=CARTESIAN_POINT('Ctrl Pts',(0.559565484335337,0.54411336510068,20.8735456079469));
#15744=CARTESIAN_POINT('Ctrl Pts',(0.578963048970497,0.658358394802545,
20.8794117138007));
#15745=CARTESIAN_POINT('Ctrl Pts',(0.598340750746892,0.772486439051222,
20.8852718128369));
#15746=CARTESIAN_POINT('Ctrl Pts',(0.622782131854229,0.885879846640568,
20.8911319118731));
#15747=CARTESIAN_POINT('Ctrl Pts',(0.652212208952136,0.998057342843189,
20.8969920109093));
#15748=CARTESIAN_POINT('Ctrl Pts',(0.682704056458585,1.11428194859214,20.9030635290228));
#15749=CARTESIAN_POINT('Ctrl Pts',(0.718551321817345,1.22920080160129,20.9091350471364));
#15750=CARTESIAN_POINT('Ctrl Pts',(0.759612461323276,1.34228906987127,20.91520656525));
#15751=CARTESIAN_POINT('Ctrl Pts',(0.799198240798473,1.45131398498159,20.9210599287956));
#15752=CARTESIAN_POINT('Ctrl Pts',(0.843629512017629,1.55863717857696,20.9269132923412));
#15753=CARTESIAN_POINT('Ctrl Pts',(0.8927287449547,1.66380396606726,20.9327666558868));
#15754=CARTESIAN_POINT('Ctrl Pts',(0.941820605809915,1.7689549631242,20.9386191405699));
#15755=CARTESIAN_POINT('Ctrl Pts',(0.99557886004476,1.87194982361109,20.944471625253));
#15756=CARTESIAN_POINT('Ctrl Pts',(1.05377843466681,1.97235524024878,20.950324109936));
#15757=CARTESIAN_POINT('Ctrl Pts',(1.11198334541237,2.07276986272188,20.9561771312138));
#15758=CARTESIAN_POINT('Ctrl Pts',(1.1746301788411,2.17059421192432,20.9620301524915));
#15759=CARTESIAN_POINT('Ctrl Pts',(1.24144900654662,2.26542154106194,20.9678831737693));
#15760=CARTESIAN_POINT('Ctrl Pts',(1.30829011962685,2.3602804969526,20.9737381471431));
#15761=CARTESIAN_POINT('Ctrl Pts',(1.37930575595772,2.45214010764749,20.9795931205169));
#15762=CARTESIAN_POINT('Ctrl Pts',(1.45418439696715,2.54062502636597,20.9854480938908));
#15763=CARTESIAN_POINT('Ctrl Pts',(1.52914790331058,2.62921023138879,20.9913097031258));
#15764=CARTESIAN_POINT('Ctrl Pts',(1.60798288596538,2.71441279485008,20.9971713123609));
#15765=CARTESIAN_POINT('Ctrl Pts',(1.69033944065475,2.79589264337699,21.003032921596));
#15766=CARTESIAN_POINT('Ctrl Pts',(1.77275152898083,2.87742743437113,21.0088984833577));
#15767=CARTESIAN_POINT('Ctrl Pts',(1.85868961223166,2.95523423535495,21.0147640451194));
#15768=CARTESIAN_POINT('Ctrl Pts',(1.94777037063086,3.02901298347535,21.0206296068811));
#15769=CARTESIAN_POINT('Ctrl Pts',(2.03698138696435,3.10289961423502,21.0265037455339));
#15770=CARTESIAN_POINT('Ctrl Pts',(2.12934392137204,3.17274618892872,21.0323778841867));
#15771=CARTESIAN_POINT('Ctrl Pts',(2.22444530359067,3.23829565427617,21.0382520228394));
#15772=CARTESIAN_POINT('Ctrl Pts',(2.24849489864431,3.2548720494958,21.0397374971048));
#15773=CARTESIAN_POINT('Ctrl Pts',(2.27271952094194,3.27117387327726,21.0412229713702));
#15774=CARTESIAN_POINT('Ctrl Pts',(2.29711225987554,3.28719744009283,21.0427084456356));
#15775=CARTESIAN_POINT('Ctrl Pts',(2.39356318796271,3.35055596226765,21.0485821350124));
#15776=CARTESIAN_POINT('Ctrl Pts',(2.49296565804658,3.40977140450462,21.0544558243892));
#15777=CARTESIAN_POINT('Ctrl Pts',(2.59492824722972,3.4645569168822,21.060329513766));
#15778=CARTESIAN_POINT('Ctrl Pts',(2.69675919312201,3.51927169601145,21.0661956196575));
#15779=CARTESIAN_POINT('Ctrl Pts',(2.80114332423419,3.56956772564308,21.072061725549));
#15780=CARTESIAN_POINT('Ctrl Pts',(2.90765992404886,3.61520111712029,21.0779278314404));
#15781=CARTESIAN_POINT('Ctrl Pts',(3.01406745221326,3.66078778058212,21.0837879305137));
#15782=CARTESIAN_POINT('Ctrl Pts',(3.12260272817269,3.70172114100203,21.089648029587));
#15783=CARTESIAN_POINT('Ctrl Pts',(3.23282068381178,3.73780330385939,21.0955081286603));
#15784=CARTESIAN_POINT('Ctrl Pts',(3.34701505223099,3.7751872289631,21.1015796467597));
#15785=CARTESIAN_POINT('Ctrl Pts',(3.46301540931486,3.80736309348091,21.1076511648592));
#15786=CARTESIAN_POINT('Ctrl Pts',(3.58030400243654,3.83416532128118,21.1137226829587));
#15787=CARTESIAN_POINT('Ctrl Pts',(3.69337832226668,3.86000452352401,21.1195760465395));
#15788=CARTESIAN_POINT('Ctrl Pts',(3.80764945932911,3.88084950156652,21.1254294101204));
#15789=CARTESIAN_POINT('Ctrl Pts',(3.92263909787558,3.89660294643846,21.1312827737013));
#15790=CARTESIAN_POINT('Ctrl Pts',(4.0376114711073,3.91235402598265,21.137135258419));
#15791=CARTESIAN_POINT('Ctrl Pts',(4.15330172210416,3.92301503636198,21.1429877431367));
#15792=CARTESIAN_POINT('Ctrl Pts',(4.26922372514543,3.92854020817745,21.1488402278543));
#15793=CARTESIAN_POINT('Ctrl Pts',(4.38515635667092,3.93406588657666,21.1546932491659));
#15794=CARTESIAN_POINT('Ctrl Pts',(4.50132036978176,3.93445477066204,21.1605462704775));
#15795=CARTESIAN_POINT('Ctrl Pts',(4.61722764119416,3.92971318208243,21.1663992917891));
#15796=CARTESIAN_POINT('Ctrl Pts',(4.73317356991329,3.92497001209173,21.172254265196));
#15797=CARTESIAN_POINT('Ctrl Pts',(4.84886217408903,3.91509298384522,21.1781092386028));
#15798=CARTESIAN_POINT('Ctrl Pts',(4.96380916969043,3.90014038978036,21.1839642120097));
#15799=CARTESIAN_POINT('Ctrl Pts',(5.07888644293921,3.88517084887172,21.1898258212765));
#15800=CARTESIAN_POINT('Ctrl Pts',(5.19322002006796,3.86511431382172,21.1956874305433));
#15801=CARTESIAN_POINT('Ctrl Pts',(5.30633444831095,3.84008045492665,21.2015490398101));
#15802=CARTESIAN_POINT('Ctrl Pts',(5.41952515043878,3.81502971551775,21.2074146016029));
#15803=CARTESIAN_POINT('Ctrl Pts',(5.5314946686843,3.7849950760068,21.2132801633956));
#15804=CARTESIAN_POINT('Ctrl Pts',(5.64178305657467,3.75013597608013,21.2191457251883));
#15805=CARTESIAN_POINT('Ctrl Pts',(5.75223271313403,3.71522590360091,21.2250198638708));
#15806=CARTESIAN_POINT('Ctrl Pts',(5.86099594678789,3.67547743287776,21.2308940025533));
#15807=CARTESIAN_POINT('Ctrl Pts',(5.96763304116629,3.6310979829402,21.2367681412357));
#15808=CARTESIAN_POINT('Ctrl Pts',(5.99459982438271,3.61987514333915,21.2382536151729));
#15809=CARTESIAN_POINT('Ctrl Pts',(6.02143076705886,3.60835637931336,21.2397390891101));
#15810=CARTESIAN_POINT('Ctrl Pts',(6.04811902591505,3.59654549993868,21.2412245630472));
#15811=CARTESIAN_POINT('Ctrl Pts',(6.15364665911984,3.54984428375247,21.2470982526581));
#15812=CARTESIAN_POINT('Ctrl Pts',(6.25729288846732,3.49841686028241,21.2529719422689));
#15813=CARTESIAN_POINT('Ctrl Pts',(6.35860447761976,3.44243664122715,21.2588456318798));
#15814=CARTESIAN_POINT('Ctrl Pts',(6.45978526401042,3.38652869788406,21.2647117380066));
#15815=CARTESIAN_POINT('Ctrl Pts',(6.55863704622935,3.32607984652786,21.2705778441334));
#15816=CARTESIAN_POINT('Ctrl Pts',(6.65472680827972,3.26131140422491,21.2764439502602));
#15817=CARTESIAN_POINT('Ctrl Pts',(6.75071817564942,3.19660928397399,21.2823040495697));
#15818=CARTESIAN_POINT('Ctrl Pts',(6.84395280796955,3.12759660044398,21.2881641488793));
#15819=CARTESIAN_POINT('Ctrl Pts',(6.93402313724634,3.05454006739746,21.2940242481889));
#15820=CARTESIAN_POINT('Ctrl Pts',(7.02734299371901,2.97884782520146,21.3000957662001));
#15821=CARTESIAN_POINT('Ctrl Pts',(7.11726551967245,2.89881465760119,21.3061672842113));
#15822=CARTESIAN_POINT('Ctrl Pts',(7.20337090161216,2.81478587577487,21.3122388022226));
#15823=CARTESIAN_POINT('Ctrl Pts',(7.28638245263658,2.73377631106523,21.3180921660407));
#15824=CARTESIAN_POINT('Ctrl Pts',(7.36584612356239,2.64905363478006,21.3239455298587));
#15825=CARTESIAN_POINT('Ctrl Pts',(7.44142084536629,2.56096702730768,21.3297988936768));
#15826=CARTESIAN_POINT('Ctrl Pts',(7.51698421987462,2.47289364574928,21.3356513786315));
#15827=CARTESIAN_POINT('Ctrl Pts',(7.58865953735275,2.38145765077103,21.3415038635863));
#15828=CARTESIAN_POINT('Ctrl Pts',(7.65614480402373,2.28704272563348,21.3473563485411));
#15829=CARTESIAN_POINT('Ctrl Pts',(7.72363625817945,2.19261914392633,21.3532093700894));
#15830=CARTESIAN_POINT('Ctrl Pts',(7.7869366575749,2.09521642523866,21.3590623916378));
#15831=CARTESIAN_POINT('Ctrl Pts',(7.84578669805172,1.99524817045103,21.3649154131861));
#15832=CARTESIAN_POINT('Ctrl Pts',(7.90465636614359,1.89524657433677,21.3707703868292));
#15833=CARTESIAN_POINT('Ctrl Pts',(7.95907251441327,1.79267809653119,21.3766253604723));
#15834=CARTESIAN_POINT('Ctrl Pts',(8.00882159145933,1.68798128561946,21.3824803341154));
#15835=CARTESIAN_POINT('Ctrl Pts',(8.05862705267118,1.58316581436881,21.3883419436163));
#15836=CARTESIAN_POINT('Ctrl Pts',(8.10375470767438,1.47621756879183,21.3942035531173));
#15837=CARTESIAN_POINT('Ctrl Pts',(8.14403896579817,1.36759552891844,21.4000651626182));
#15838=CARTESIAN_POINT('Ctrl Pts',(8.18435038788405,1.25890024443018,21.4059307246442));
#15839=CARTESIAN_POINT('Ctrl Pts',(8.21981178382042,1.14852931061809,21.4117962866702));
#15840=CARTESIAN_POINT('Ctrl Pts',(8.25030779065407,1.03695565791324,21.4176618486961));
#15841=CARTESIAN_POINT('Ctrl Pts',(8.2808483901102,0.925218857233,21.4235359876087));
#15842=CARTESIAN_POINT('Ctrl Pts',(8.30640901925999,0.812276229203628,21.4294101265213));
#15843=CARTESIAN_POINT('Ctrl Pts',(8.32692559949976,0.698609714801456,21.4352842654339));
#15844=CARTESIAN_POINT('Ctrl Pts',(8.33211390016254,0.669865350725404,21.4367697371089));
#15845=CARTESIAN_POINT('Ctrl Pts',(8.33697989374072,0.641074711219869,21.4382552087839));
#15846=CARTESIAN_POINT('Ctrl Pts',(8.34152307122561,0.61224561164665,21.4397406804589));
#15847=CARTESIAN_POINT('Ctrl Pts',(8.37110695828926,0.424518667507654,21.4494136519451));
#15848=CARTESIAN_POINT('Ctrl Pts',(8.38708943569742,0.234594111220408,21.4590866234314));
#15849=CARTESIAN_POINT('Ctrl Pts',(8.38922270894465,0.0440238599231025,
21.4687595949177));
#15850=CARTESIAN_POINT('Ctrl Pts',(8.3893753872624,0.0303847513748413,21.4694518892668));
#15851=CARTESIAN_POINT('Ctrl Pts',(8.38945714112686,0.0167423532144361,
21.470144183616));
#15852=CARTESIAN_POINT('Ctrl Pts',(8.38946788667581,0.00309724383391784,
21.4708364779651));
#15853=CARTESIAN_POINT('',(8.38721926685989,-0.00134106201782228,18.9708368356832));
#15854=CARTESIAN_POINT('Ctrl Pts',(8.38344183965918,-0.00135169739119494,
18.9708374363438));
#15855=CARTESIAN_POINT('Ctrl Pts',(8.38518238981383,-0.574802882154291,
18.9997407147355));
#15856=CARTESIAN_POINT('Ctrl Pts',(7.99895462546289,-2.45889274337807,19.0948160322645));
#15857=CARTESIAN_POINT('Ctrl Pts',(5.09181089789537,-4.60543441257073,19.2560633889306));
#15858=CARTESIAN_POINT('Ctrl Pts',(0.930911257582632,-3.03053249053979,
19.4545795063423));
#15859=CARTESIAN_POINT('Ctrl Pts',(-0.00134956819690293,1.31967343935667,
19.6530956237539));
#15860=CARTESIAN_POINT('Ctrl Pts',(3.14877515140037,4.46134753659125,19.8516117411657));
#15861=CARTESIAN_POINT('Ctrl Pts',(7.2934463239171,3.56148175989967,20.0408581667598));
#15862=CARTESIAN_POINT('Ctrl Pts',(8.38379978416848,1.11910507696889,20.1639325532169));
#15863=CARTESIAN_POINT('Ctrl Pts',(8.39304923023168,-0.00285552977342319,
20.2208349005368));
#15864=CARTESIAN_POINT('',(8.38946749588772,0.00355905287639204,17.7208364779273));
#15865=CARTESIAN_POINT('Ctrl Pts',(8.38946749588839,0.003559052130875,17.720836477965));
#15866=CARTESIAN_POINT('Ctrl Pts',(8.38957613282376,-0.116492263818579,
17.7269037316768));
#15867=CARTESIAN_POINT('Ctrl Pts',(8.38418299164283,-0.236671020316373,
17.7329709853887));
#15868=CARTESIAN_POINT('Ctrl Pts',(8.37328515500261,-0.356428169460906,
17.7390382391005));
#15869=CARTESIAN_POINT('Ctrl Pts',(8.36287449178463,-0.470831733108411,
17.7448342642326));
#15870=CARTESIAN_POINT('Ctrl Pts',(8.34744071078401,-0.584850100472209,
17.7506302893647));
#15871=CARTESIAN_POINT('Ctrl Pts',(8.32703452225374,-0.698005988649095,
17.7564263144967));
#15872=CARTESIAN_POINT('Ctrl Pts',(8.3066329990051,-0.811136007022526,17.7622210145362));
#15873=CARTESIAN_POINT('Ctrl Pts',(8.28126140237628,-0.923403522833055,
17.7680157145757));
#15874=CARTESIAN_POINT('Ctrl Pts',(8.25102193708545,-1.03433931268114,17.7738104146152));
#15875=CARTESIAN_POINT('Ctrl Pts',(8.2207817158513,-1.14527787576511,17.7796052595138));
#15876=CARTESIAN_POINT('Ctrl Pts',(8.18567349567977,-1.25488423951721,17.7854001044125));
#15877=CARTESIAN_POINT('Ctrl Pts',(8.14584972406252,-1.36270306988538,17.7911949493112));
#15878=CARTESIAN_POINT('Ctrl Pts',(8.1060148561022,-1.47055194247913,17.7969914088632));
#15879=CARTESIAN_POINT('Ctrl Pts',(8.06146197206998,-1.57661189612038,17.8027878684152));
#15880=CARTESIAN_POINT('Ctrl Pts',(8.01239183446375,-1.68044712822125,17.8085843279673));
#15881=CARTESIAN_POINT('Ctrl Pts',(7.96326770939825,-1.78439660088957,17.8143871648425));
#15882=CARTESIAN_POINT('Ctrl Pts',(7.90961659298189,-1.88611608537518,17.8201900017176));
#15883=CARTESIAN_POINT('Ctrl Pts',(7.85168541861316,-1.98519399355516,17.8259928385928));
#15884=CARTESIAN_POINT('Ctrl Pts',(7.79371681124774,-2.08433592223964,17.831799425048));
#15885=CARTESIAN_POINT('Ctrl Pts',(7.73146287032479,-2.18083252392463,17.8376060115032));
#15886=CARTESIAN_POINT('Ctrl Pts',(7.6652130495779,-2.27430237786288,17.8434125979584));
#15887=CARTESIAN_POINT('Ctrl Pts',(7.59886475324261,-2.36791116800896,17.8492278154863));
#15888=CARTESIAN_POINT('Ctrl Pts',(7.5285089834235,-2.45848390128237,17.8550430330141));
#15889=CARTESIAN_POINT('Ctrl Pts',(7.45447449914436,-2.54567332232279,17.860858250542));
#15890=CARTESIAN_POINT('Ctrl Pts',(7.43074226748708,-2.57362245384363,17.8627223560444));
#15891=CARTESIAN_POINT('Ctrl Pts',(7.40663229723318,-2.6012242220324,17.8645864615467));
#15892=CARTESIAN_POINT('Ctrl Pts',(7.38215616249663,-2.62846804217306,17.8664505670491));
#15893=CARTESIAN_POINT('Ctrl Pts',(7.3050332674982,-2.71431175494391,17.8723242564396));
#15894=CARTESIAN_POINT('Ctrl Pts',(7.22400056262058,-2.7969012245466,17.8781979458302));
#15895=CARTESIAN_POINT('Ctrl Pts',(7.13936345849576,-2.87585933148988,17.8840716352208));
#15896=CARTESIAN_POINT('Ctrl Pts',(7.05483562882367,-2.95471549609931,17.8899377411265));
#15897=CARTESIAN_POINT('Ctrl Pts',(6.9667129537625,-3.02994934254737,17.8958038470323));
#15898=CARTESIAN_POINT('Ctrl Pts',(6.87534011754019,-3.10121783023804,17.901669952938));
#15899=CARTESIAN_POINT('Ctrl Pts',(6.78406084593812,-3.17241333990525,17.9075300520261));
#15900=CARTESIAN_POINT('Ctrl Pts',(6.68953835692216,-3.23965131485814,17.9133901511141));
#15901=CARTESIAN_POINT('Ctrl Pts',(6.59215260222646,-3.30262698542814,17.9192502502022));
#15902=CARTESIAN_POINT('Ctrl Pts',(6.49125339167387,-3.36787467452176,17.9253217682963));
#15903=CARTESIAN_POINT('Ctrl Pts',(6.38728074481688,-3.42854639602921,17.9313932863904));
#15904=CARTESIAN_POINT('Ctrl Pts',(6.28069313369929,-3.48435011122029,17.9374648044845));
#15905=CARTESIAN_POINT('Ctrl Pts',(6.17793530063186,-3.53814875432732,17.9433181680812));
#15906=CARTESIAN_POINT('Ctrl Pts',(6.07274758221572,-3.58742298538944,17.949171531678));
#15907=CARTESIAN_POINT('Ctrl Pts',(5.96556771046482,-3.63195682830358,17.9550248952747));
#15908=CARTESIAN_POINT('Ctrl Pts',(5.85840393141092,-3.6764839846111,17.9608773800086));
#15909=CARTESIAN_POINT('Ctrl Pts',(5.74924897519467,-3.71627200952174,17.9667298647425));
#15910=CARTESIAN_POINT('Ctrl Pts',(5.6385612587536,-3.75115277520315,17.9725823494764));
#15911=CARTESIAN_POINT('Ctrl Pts',(5.52786339373526,-3.78603673898239,17.9784353708046));
#15912=CARTESIAN_POINT('Ctrl Pts',(5.41563288318893,-3.81601242493351,17.9842883921328));
#15913=CARTESIAN_POINT('Ctrl Pts',(5.302343348947,-3.84096156782231,17.9901414134609));
#15914=CARTESIAN_POINT('Ctrl Pts',(5.18901603045765,-3.86591903173206,17.9959963868848));
#15915=CARTESIAN_POINT('Ctrl Pts',(5.07462938919954,-3.88584653022755,18.0018513603086));
#15916=CARTESIAN_POINT('Ctrl Pts',(4.95966657710611,-3.90067703165643,18.0077063337324));
#15917=CARTESIAN_POINT('Ctrl Pts',(4.84457346943133,-3.9155243415538,18.0135679430165));
#15918=CARTESIAN_POINT('Ctrl Pts',(4.72890329752009,-3.92526307136828,18.0194295523007));
#15919=CARTESIAN_POINT('Ctrl Pts',(4.61314376508996,-3.92987812168105,18.0252911615848));
#15920=CARTESIAN_POINT('Ctrl Pts',(4.49730617515689,-3.93449628395615,18.0311567233952));
#15921=CARTESIAN_POINT('Ctrl Pts',(4.3813795168395,-3.93398388900967,18.0370222852055));
#15922=CARTESIAN_POINT('Ctrl Pts',(4.26584918109284,-3.92837791513815,18.0428878470159));
#15923=CARTESIAN_POINT('Ctrl Pts',(4.15014991165982,-3.92276374395788,18.0487619857162));
#15924=CARTESIAN_POINT('Ctrl Pts',(4.03484853116391,-3.91204116750257,18.0546361244165));
#15925=CARTESIAN_POINT('Ctrl Pts',(3.920423093794,-3.89629871449354,18.0605102631168));
#15926=CARTESIAN_POINT('Ctrl Pts',(3.89148676869231,-3.89231770512502,18.0619957368981));
#15927=CARTESIAN_POINT('Ctrl Pts',(3.8626063960005,-3.8880159260561,18.0634812106794));
#15928=CARTESIAN_POINT('Ctrl Pts',(3.83378956369566,-3.88339531690038,18.0649666844607));
#15929=CARTESIAN_POINT('Ctrl Pts',(3.71984536332599,-3.86512503618739,18.0708403738513));
#15930=CARTESIAN_POINT('Ctrl Pts',(3.6065161839055,-3.84180515537926,18.0767140632418));
#15931=CARTESIAN_POINT('Ctrl Pts',(3.49428448791038,-3.81348787336366,18.0825877526324));
#15932=CARTESIAN_POINT('Ctrl Pts',(3.38219769357849,-3.78520715161943,18.0884538585381));
#15933=CARTESIAN_POINT('Ctrl Pts',(3.27120596174663,-3.7519419599581,18.0943199644439));
#15934=CARTESIAN_POINT('Ctrl Pts',(3.16178440871784,-3.71379597367145,18.1001860703497));
#15935=CARTESIAN_POINT('Ctrl Pts',(3.0524749019655,-3.67568904838883,18.1060461694377));
#15936=CARTESIAN_POINT('Ctrl Pts',(2.94473276368286,-3.63271140485437,18.1119062685257));
#15937=CARTESIAN_POINT('Ctrl Pts',(2.83902006966279,-3.58501710095584,18.1177663676137));
#15938=CARTESIAN_POINT('Ctrl Pts',(2.7294935028116,-3.5356020953807,18.1238378857078));
#15939=CARTESIAN_POINT('Ctrl Pts',(2.62214601837952,-3.48112378161057,18.1299094038019));
#15940=CARTESIAN_POINT('Ctrl Pts',(2.51747156085872,-3.42180910032832,18.1359809218961));
#15941=CARTESIAN_POINT('Ctrl Pts',(2.41655814025049,-3.36462564294771,18.1418342854928));
#15942=CARTESIAN_POINT('Ctrl Pts',(2.31812935462938,-3.30294760703951,18.1476876490895));
#15943=CARTESIAN_POINT('Ctrl Pts',(2.22260398909766,-3.2370257395504,18.1535410126863));
#15944=CARTESIAN_POINT('Ctrl Pts',(2.12709296637793,-3.17111377000772,18.1593934974202));
#15945=CARTESIAN_POINT('Ctrl Pts',(2.03448483688213,-3.10095947046617,18.1652459821541));
#15946=CARTESIAN_POINT('Ctrl Pts',(1.94516939192894,-3.02685690857867,18.171098466888));
#15947=CARTESIAN_POINT('Ctrl Pts',(1.85584575794859,-2.95274755248114,18.1769514882162));
#15948=CARTESIAN_POINT('Ctrl Pts',(1.76981572662577,-2.87468947822612,18.1828045095444));
#15949=CARTESIAN_POINT('Ctrl Pts',(1.68743543206477,-2.79301656124772,18.1886575308726));
#15950=CARTESIAN_POINT('Ctrl Pts',(1.6050276620849,-2.71131640477453,18.1945125042964));
#15951=CARTESIAN_POINT('Ctrl Pts',(1.52627234256563,-2.62599929897492,18.2003674777202));
#15952=CARTESIAN_POINT('Ctrl Pts',(1.45148772198882,-2.53743490171365,18.206222451144));
#15953=CARTESIAN_POINT('Ctrl Pts',(1.37661834265025,-2.44877012808368,18.2120840604281));
#15954=CARTESIAN_POINT('Ctrl Pts',(1.30572891123235,-2.35685103299678,18.2179456697123));
#15955=CARTESIAN_POINT('Ctrl Pts',(1.23909650471908,-2.2620792521754,18.2238072789964));
#15956=CARTESIAN_POINT('Ctrl Pts',(1.17241916748489,-2.16724356604642,18.2296728408068));
#15957=CARTESIAN_POINT('Ctrl Pts',(1.11000479292623,-2.06955171118859,18.2355384026171));
#15958=CARTESIAN_POINT('Ctrl Pts',(1.05208544294362,-1.96943161171664,18.2414039644274));
#15959=CARTESIAN_POINT('Ctrl Pts',(0.99408140066554,-1.86916511210294,18.2472781031277));
#15960=CARTESIAN_POINT('Ctrl Pts',(0.940585690803906,-1.76646364659972,
18.2531522418281));
#15961=CARTESIAN_POINT('Ctrl Pts',(0.891783079702071,-1.66177692015513,
18.2590263805284));
#15962=CARTESIAN_POINT('Ctrl Pts',(0.879441696062798,-1.63530335606045,
18.2605118543097));
#15963=CARTESIAN_POINT('Ctrl Pts',(0.867400190053486,-1.60870291690944,
18.261997328091));
#15964=CARTESIAN_POINT('Ctrl Pts',(0.855661045316142,-1.58198303042175,
18.2634828018723));
#15965=CARTESIAN_POINT('Ctrl Pts',(0.809243470825123,-1.47633033176402,
18.2693564912629));
#15966=CARTESIAN_POINT('Ctrl Pts',(0.767402523625336,-1.3684570037977,18.2752301806535));
#15967=CARTESIAN_POINT('Ctrl Pts',(0.730355888078917,-1.25879676104101,
18.2811038700441));
#15968=CARTESIAN_POINT('Ctrl Pts',(0.693357083219335,-1.14927809995974,
18.2869699759499));
#15969=CARTESIAN_POINT('Ctrl Pts',(0.661140411341709,-1.03797749994103,
18.2928360818556));
#15970=CARTESIAN_POINT('Ctrl Pts',(0.633876318351498,-0.92535040830438,
18.2987021877614));
#15971=CARTESIAN_POINT('Ctrl Pts',(0.60664014344528,-0.812838645375174,
18.3045622868494));
#15972=CARTESIAN_POINT('Ctrl Pts',(0.584346556662297,-0.699003491780741,
18.3104223859375));
#15973=CARTESIAN_POINT('Ctrl Pts',(0.567116597632666,-0.584316749682063,
18.3162824850255));
#15974=CARTESIAN_POINT('Ctrl Pts',(0.54926502098909,-0.465492371570913,
18.3223540031196));
#15975=CARTESIAN_POINT('Ctrl Pts',(0.53684948325925,-0.345754225986596,
18.3284255212137));
#15976=CARTESIAN_POINT('Ctrl Pts',(0.529947056413576,-0.225640405064559,
18.3344970393078));
#15977=CARTESIAN_POINT('Ctrl Pts',(0.523292639280731,-0.109842369720487,
18.3403504029046));
#15978=CARTESIAN_POINT('Ctrl Pts',(0.52176199601243,0.00630436111424336,
18.3462037665014));
#15979=CARTESIAN_POINT('Ctrl Pts',(0.52537144936873,0.122311946727261,18.3520571300981));
#15980=CARTESIAN_POINT('Ctrl Pts',(0.528980360777749,0.238302114191518,
18.357909614832));
#15981=CARTESIAN_POINT('Ctrl Pts',(0.537727821401377,0.354152765141346,
18.3637620995659));
#15982=CARTESIAN_POINT('Ctrl Pts',(0.551578033464427,0.469376938001323,
18.3696145842999));
#15983=CARTESIAN_POINT('Ctrl Pts',(0.565429515405994,0.584611675371151,
18.375467605628));
#15984=CARTESIAN_POINT('Ctrl Pts',(0.584384629527829,0.699219410251753,
18.3813206269562));
#15985=CARTESIAN_POINT('Ctrl Pts',(0.60835588136781,0.812719883312295,18.3871736482844));
#15986=CARTESIAN_POINT('Ctrl Pts',(0.63233512808316,0.926258210972273,18.3930286217083));
#15987=CARTESIAN_POINT('Ctrl Pts',(0.661333753833645,1.03868813847936,18.3988835951321));
#15988=CARTESIAN_POINT('Ctrl Pts',(0.695213657743602,1.14954184409258,18.4047385685559));
#15989=CARTESIAN_POINT('Ctrl Pts',(0.729131960172976,1.26052118814265,18.4106001778401));
#15990=CARTESIAN_POINT('Ctrl Pts',(0.767942462081084,1.36992034933718,18.4164617871243));
#15991=CARTESIAN_POINT('Ctrl Pts',(0.811457871886902,1.47728876716716,18.4223233964084));
#15992=CARTESIAN_POINT('Ctrl Pts',(0.855002624453212,1.58472958431,18.4281889582188));
#15993=CARTESIAN_POINT('Ctrl Pts',(0.903258430626849,1.69013655669717,18.4340545200292));
#15994=CARTESIAN_POINT('Ctrl Pts',(0.95599150537962,1.79308269916004,18.4399200818395));
#15995=CARTESIAN_POINT('Ctrl Pts',(1.00880168882113,1.89617937413202,18.4457942205399));
#15996=CARTESIAN_POINT('Ctrl Pts',(1.06610200308904,1.99680768016434,18.4516683592402));
#15997=CARTESIAN_POINT('Ctrl Pts',(1.12761472117852,2.09456856731924,18.4575424979405));
#15998=CARTESIAN_POINT('Ctrl Pts',(1.14317028337947,2.11929069972031,18.4590279717217));
#15999=CARTESIAN_POINT('Ctrl Pts',(1.15899502620116,2.14382962277052,18.4605134455029));
#16000=CARTESIAN_POINT('Ctrl Pts',(1.17508405447843,2.1681792228085,18.461998919284));
#16001=CARTESIAN_POINT('Ctrl Pts',(1.23870143762904,2.26445960770712,18.4678726086746));
#16002=CARTESIAN_POINT('Ctrl Pts',(1.30666586619626,2.35809804104783,18.4737462980651));
#16003=CARTESIAN_POINT('Ctrl Pts',(1.37873089523012,2.44867648018753,18.4796199874557));
#16004=CARTESIAN_POINT('Ctrl Pts',(1.45070288154124,2.53913797405278,18.4854860933614));
#16005=CARTESIAN_POINT('Ctrl Pts',(1.52676468489713,2.62654701009299,18.4913521992672));
#16006=CARTESIAN_POINT('Ctrl Pts',(1.60662598968765,2.7105134589526,18.4972183051729));
#16007=CARTESIAN_POINT('Ctrl Pts',(1.68640551751977,2.79439392723859,18.5030784042609));
#16008=CARTESIAN_POINT('Ctrl Pts',(1.7699765249434,2.87483852260551,18.508938503349));
#16009=CARTESIAN_POINT('Ctrl Pts',(1.85700816963507,2.95148976606359,18.514798602437));
#16010=CARTESIAN_POINT('Ctrl Pts',(1.94717971751622,3.03090641151614,18.5208701205311));
#16011=CARTESIAN_POINT('Ctrl Pts',(2.04106603977298,3.10625047284982,18.5269416386253));
#16012=CARTESIAN_POINT('Ctrl Pts',(2.13825675480958,3.17716548101862,18.5330131567194));
#16013=CARTESIAN_POINT('Ctrl Pts',(2.23195532978195,3.24553245627,18.5388665203161));
#16014=CARTESIAN_POINT('Ctrl Pts',(2.32872456285561,3.30978291527765,18.5447198839129));
#16015=CARTESIAN_POINT('Ctrl Pts',(2.42816336637527,3.36963867880817,18.5505732475096));
#16016=CARTESIAN_POINT('Ctrl Pts',(2.52758723949308,3.42948545519714,18.5564257322435));
#16017=CARTESIAN_POINT('Ctrl Pts',(2.62967953219101,3.48493863512843,18.5622782169774));
#16018=CARTESIAN_POINT('Ctrl Pts',(2.73401164052156,3.53576431325191,18.5681307017113));
#16019=CARTESIAN_POINT('Ctrl Pts',(2.83835331470551,3.58659465140761,18.5739837230395));
#16020=CARTESIAN_POINT('Ctrl Pts',(2.94493484132314,3.63279646338019,18.5798367443676));
#16021=CARTESIAN_POINT('Ctrl Pts',(3.05330522310997,3.67418291830177,18.5856897656958));
#16022=CARTESIAN_POINT('Ctrl Pts',(3.16171174851262,3.71558317640557,18.5915447391196));
#16023=CARTESIAN_POINT('Ctrl Pts',(3.27190792968327,3.75216473665313,18.5973997125435));
#16024=CARTESIAN_POINT('Ctrl Pts',(3.3834257865437,3.78379003567876,18.6032546859673));
#16025=CARTESIAN_POINT('Ctrl Pts',(3.49507003457047,3.81545117791857,18.6091162952515));
#16026=CARTESIAN_POINT('Ctrl Pts',(3.60803855041088,3.84214473439123,18.6149779045356));
#16027=CARTESIAN_POINT('Ctrl Pts',(3.72185119198616,3.86378383454475,18.6208395138197));
#16028=CARTESIAN_POINT('Ctrl Pts',(3.83574057826135,3.8854375261024,18.6267050756301));
#16029=CARTESIAN_POINT('Ctrl Pts',(3.95047481579575,3.9020299157593,18.6325706374404));
#16030=CARTESIAN_POINT('Ctrl Pts',(4.0655683685142,3.91352598218824,18.6384361992507));
#16031=CARTESIAN_POINT('Ctrl Pts',(4.18083021623513,3.92503885868588,18.644310337951));
#16032=CARTESIAN_POINT('Ctrl Pts',(4.29645201679292,3.9314405167363,18.6501844766514));
#16033=CARTESIAN_POINT('Ctrl Pts',(4.41194788694267,3.9327480037544,18.6560586153517));
#16034=CARTESIAN_POINT('Ctrl Pts',(4.44115490702077,3.93307864587641,18.657544089133));
#16035=CARTESIAN_POINT('Ctrl Pts',(4.47035390021833,3.9330837738788,18.6590295629144));
#16036=CARTESIAN_POINT('Ctrl Pts',(4.49953707546216,3.93276418693331,18.6605150366957));
#16037=CARTESIAN_POINT('Ctrl Pts',(4.61492982689533,3.93150051303031,18.6663887260862));
#16038=CARTESIAN_POINT('Ctrl Pts',(4.7304591003676,3.92515175568444,18.6722624154768));
#16039=CARTESIAN_POINT('Ctrl Pts',(4.84564001121418,3.91369837962824,18.6781361048673));
#16040=CARTESIAN_POINT('Ctrl Pts',(4.96067221268433,3.9022597909565,18.684002210773));
#16041=CARTESIAN_POINT('Ctrl Pts',(5.0753565386091,3.88572973050952,18.6898683166788));
#16042=CARTESIAN_POINT('Ctrl Pts',(5.18920777737616,3.86414065993848,18.6957344225845));
#16043=CARTESIAN_POINT('Ctrl Pts',(5.30294243392468,3.84257369630075,18.7015945216725));
#16044=CARTESIAN_POINT('Ctrl Pts',(5.41584529664469,3.81595810322179,18.7074546207605));
#16045=CARTESIAN_POINT('Ctrl Pts',(5.52743662036568,3.78437809734187,18.7133147198485));
#16046=CARTESIAN_POINT('Ctrl Pts',(5.6430539044671,3.75165875689501,18.7193862379426));
#16047=CARTESIAN_POINT('Ctrl Pts',(5.7572627786953,3.71361007580449,18.7254577560367));
#16048=CARTESIAN_POINT('Ctrl Pts',(5.86954122754744,3.67038365568536,18.7315292741308));
#16049=CARTESIAN_POINT('Ctrl Pts',(5.97778542200087,3.6287103953871,18.7373826377275));
#16050=CARTESIAN_POINT('Ctrl Pts',(6.08423510851336,3.58222523438231,18.7432360013243));
#16051=CARTESIAN_POINT('Ctrl Pts',(6.18843909745943,3.53111440616699,18.749089364921));
#16052=CARTESIAN_POINT('Ctrl Pts',(6.2926274405271,3.48001125207059,18.7549418496548));
#16053=CARTESIAN_POINT('Ctrl Pts',(6.39457038564771,3.42428399363418,18.7607943343887));
#16054=CARTESIAN_POINT('Ctrl Pts',(6.49383903004364,3.36416598780318,18.7666468191226));
#16055=CARTESIAN_POINT('Ctrl Pts',(6.59311677604133,3.30404246995829,18.7724998404507));
#16056=CARTESIAN_POINT('Ctrl Pts',(6.68971938047393,3.23952761847101,18.7783528617788));
#16057=CARTESIAN_POINT('Ctrl Pts',(6.78324535799057,3.1708991270913,18.784205883107));
#16058=CARTESIAN_POINT('Ctrl Pts',(6.87680252822683,3.10224774678441,18.7900608565308));
#16059=CARTESIAN_POINT('Ctrl Pts',(6.96728069825453,3.0294802427534,18.7959158299545));
#16060=CARTESIAN_POINT('Ctrl Pts',(7.05431057604661,2.95291528792143,18.8017708033783));
#16061=CARTESIAN_POINT('Ctrl Pts',(7.14143909102679,2.87626355654737,18.8076324126624));
#16062=CARTESIAN_POINT('Ctrl Pts',(7.2251112028821,2.79580605704661,18.8134940219466));
#16063=CARTESIAN_POINT('Ctrl Pts',(7.30499362401849,2.71189916322325,18.8193556312307));
#16064=CARTESIAN_POINT('Ctrl Pts',(7.38492991045813,2.62793569036514,18.825221193041));
#16065=CARTESIAN_POINT('Ctrl Pts',(7.46107114709653,2.54051850246574,18.8310867548513));
#16066=CARTESIAN_POINT('Ctrl Pts',(7.53312469151333,2.4500366139045,18.8369523166616));
#16067=CARTESIAN_POINT('Ctrl Pts',(7.60528359588407,2.35942241863041,18.8428264553619));
#16068=CARTESIAN_POINT('Ctrl Pts',(7.67334263714126,2.26573491202981,18.8487005940622));
#16069=CARTESIAN_POINT('Ctrl Pts',(7.73705273843312,2.16939162717199,18.8545747327625));
#16070=CARTESIAN_POINT('Ctrl Pts',(7.75316398297845,2.14502798324159,18.8560602065441));
#16071=CARTESIAN_POINT('Ctrl Pts',(7.7689973440063,2.12049462006162,18.8575456803257));
#16072=CARTESIAN_POINT('Ctrl Pts',(7.78454926945208,2.09579851777062,18.8590311541073));
#16073=CARTESIAN_POINT('Ctrl Pts',(7.84764214276654,1.99560847643847,18.8650575981925));
#16074=CARTESIAN_POINT('Ctrl Pts',(7.90630062493316,1.89241860175928,18.8710840422777));
#16075=CARTESIAN_POINT('Ctrl Pts',(7.96023592199444,1.78664688751461,18.8771104863629));
#16076=CARTESIAN_POINT('Ctrl Pts',(8.01409026531018,1.68103393046431,18.8831278851058));
#16077=CARTESIAN_POINT('Ctrl Pts',(8.06323536030736,1.57284718606672,18.8891452838487));
#16078=CARTESIAN_POINT('Ctrl Pts',(8.10742607641088,1.46253280366693,18.8951626825916));
#16079=CARTESIAN_POINT('Ctrl Pts',(8.15373732803705,1.34692487576338,18.9014688322061));
#16080=CARTESIAN_POINT('Ctrl Pts',(8.19460665858368,1.22898037754779,18.9077749818206));
#16081=CARTESIAN_POINT('Ctrl Pts',(8.22980582173832,1.10924254845737,18.914081131435));
#16082=CARTESIAN_POINT('Ctrl Pts',(8.26330090637412,0.995301523727039,18.9200819847546));
#16083=CARTESIAN_POINT('Ctrl Pts',(8.29166179065473,0.879737151538623,18.9260828380741));
#16084=CARTESIAN_POINT('Ctrl Pts',(8.31474103369602,0.763037832375923,18.9320836913937));
#16085=CARTESIAN_POINT('Ctrl Pts',(8.33780142356753,0.646433843552852,18.9380796426848));
#16086=CARTESIAN_POINT('Ctrl Pts',(8.35558868569572,0.528697128874555,18.9440755939759));
#16087=CARTESIAN_POINT('Ctrl Pts',(8.36800575363701,0.410329204298241,18.9500715452669));
#16088=CARTESIAN_POINT('Ctrl Pts',(8.38041353140312,0.292049839981025,18.9560630105201));
#16089=CARTESIAN_POINT('Ctrl Pts',(8.38745907960768,0.173140588104466,18.9620544757732));
#16090=CARTESIAN_POINT('Ctrl Pts',(8.38909685992391,0.0541105422630869,
18.9680459410264));
#16091=CARTESIAN_POINT('Ctrl Pts',(8.38935112641114,0.0356310481993439,
18.968976120006));
#16092=CARTESIAN_POINT('Ctrl Pts',(8.389475152377,0.0171486531632183,18.9699062989855));
#16093=CARTESIAN_POINT('Ctrl Pts',(8.38946887973726,-0.00133472821663341,
18.9708364779651));
#16094=CARTESIAN_POINT('',(8.39185523779378,-0.000723473480808207,16.4708361660978));
#16095=CARTESIAN_POINT('Ctrl Pts',(8.38946903862512,-0.000729169072716852,
16.4708364779651));
#16096=CARTESIAN_POINT('Ctrl Pts',(8.38946175098302,-0.0400373309035612,
16.4728369003659));
#16097=CARTESIAN_POINT('Ctrl Pts',(8.38886518453448,-0.0793393664645754,
16.4748373227667));
#16098=CARTESIAN_POINT('Ctrl Pts',(8.38767979182206,-0.118623544857041,
16.4768377451675));
#16099=CARTESIAN_POINT('Ctrl Pts',(8.38419921262247,-0.23397071440906,16.4827114345581));
#16100=CARTESIAN_POINT('Ctrl Pts',(8.37563186558806,-0.349356676786783,
16.4885851239486));
#16101=CARTESIAN_POINT('Ctrl Pts',(8.36196753555699,-0.464296261488952,
16.4944588133392));
#16102=CARTESIAN_POINT('Ctrl Pts',(8.34832084745971,-0.579087448389105,
16.5003249192449));
#16103=CARTESIAN_POINT('Ctrl Pts',(8.32959031151523,-0.693432997207276,
16.5061910251507));
#16104=CARTESIAN_POINT('Ctrl Pts',(8.3058177061635,-0.80684840961582,16.5120571310564));
#16105=CARTESIAN_POINT('Ctrl Pts',(8.28206944365678,-0.920147686086943,
16.5179172301445));
#16106=CARTESIAN_POINT('Ctrl Pts',(8.25328946565947,-1.03251831869173,16.5237773292325));
#16107=CARTESIAN_POINT('Ctrl Pts',(8.21957119101511,-1.1434822689476,16.5296374283205));
#16108=CARTESIAN_POINT('Ctrl Pts',(8.18463643794527,-1.25844954537939,16.5357089464147));
#16109=CARTESIAN_POINT('Ctrl Pts',(8.14440038901463,-1.37190627480333,16.5417804645088));
#16110=CARTESIAN_POINT('Ctrl Pts',(8.09902464777767,-1.48333345093231,16.5478519826029));
#16111=CARTESIAN_POINT('Ctrl Pts',(8.05527929318676,-1.59075695957257,16.5537053461996));
#16112=CARTESIAN_POINT('Ctrl Pts',(8.00675740558003,-1.69629383642343,16.5595587097964));
#16113=CARTESIAN_POINT('Ctrl Pts',(7.95365385316226,-1.79949655341213,16.5654120733931));
#16114=CARTESIAN_POINT('Ctrl Pts',(7.90055827406422,-1.90268377486013,16.571264558127));
#16115=CARTESIAN_POINT('Ctrl Pts',(7.84288258698029,-2.00353716603874,16.5771170428609));
#16116=CARTESIAN_POINT('Ctrl Pts',(7.78086834664954,-2.10163238703154,16.5829695275948));
#16117=CARTESIAN_POINT('Ctrl Pts',(7.7188484204455,-2.19973660203915,16.588822548923));
#16118=CARTESIAN_POINT('Ctrl Pts',(7.6524893710108,-2.29508179491168,16.5946755702512));
#16119=CARTESIAN_POINT('Ctrl Pts',(7.58207655491009,-2.38727188997862,16.6005285915793));
#16120=CARTESIAN_POINT('Ctrl Pts',(7.51164025477536,-2.47949273222268,16.6063835650032));
#16121=CARTESIAN_POINT('Ctrl Pts',(7.43714775020153,-2.5685560560827,16.612238538427));
#16122=CARTESIAN_POINT('Ctrl Pts',(7.35892475080396,-2.65409876063656,16.6180935118508));
#16123=CARTESIAN_POINT('Ctrl Pts',(7.28061309568405,-2.73973841685837,16.623955121135));
#16124=CARTESIAN_POINT('Ctrl Pts',(7.19856278579147,-2.82184918457426,16.6298167304191));
#16125=CARTESIAN_POINT('Ctrl Pts',(7.11313653287923,-2.90010468502751,16.6356783397033));
#16126=CARTESIAN_POINT('Ctrl Pts',(7.02765267641722,-2.97841295373948,16.6415439015136));
#16127=CARTESIAN_POINT('Ctrl Pts',(6.93878865998304,-3.05286051407819,16.647409463324));
#16128=CARTESIAN_POINT('Ctrl Pts',(6.84693904892941,-3.12316225210835,16.6532750251343));
#16129=CARTESIAN_POINT('Ctrl Pts',(6.75495513121677,-3.19356678852219,16.6591491638346));
#16130=CARTESIAN_POINT('Ctrl Pts',(6.65997724365918,-3.25981316853829,16.665023302535));
#16131=CARTESIAN_POINT('Ctrl Pts',(6.56242762797238,-3.32166038370137,16.6708974412353));
#16132=CARTESIAN_POINT('Ctrl Pts',(6.53775892267483,-3.33730053475261,16.6723829150166));
#16133=CARTESIAN_POINT('Ctrl Pts',(6.51292586866964,-3.35265959262508,16.6738683887978));
#16134=CARTESIAN_POINT('Ctrl Pts',(6.48793551305559,-3.36773414002521,16.6753538625791));
#16135=CARTESIAN_POINT('Ctrl Pts',(6.38912152624024,-3.42734017969304,16.6812275519697));
#16136=CARTESIAN_POINT('Ctrl Pts',(6.28751735628548,-3.48269279839213,16.6871012413602));
#16137=CARTESIAN_POINT('Ctrl Pts',(6.18352515803437,-3.53352039669864,16.6929749307508));
#16138=CARTESIAN_POINT('Ctrl Pts',(6.07966722348089,-3.58428237180066,16.6988410366566));
#16139=CARTESIAN_POINT('Ctrl Pts',(5.97342775983422,-3.63053076501999,16.7047071425623));
#16140=CARTESIAN_POINT('Ctrl Pts',(5.8652365433307,-3.67203803195604,16.7105732484681));
#16141=CARTESIAN_POINT('Ctrl Pts',(5.75715611325451,-3.71350279597956,16.7164333475561));
#16142=CARTESIAN_POINT('Ctrl Pts',(5.64712828908232,-3.75023594331914,16.7222934466441));
#16143=CARTESIAN_POINT('Ctrl Pts',(5.5356054135459,-3.78205682535406,16.7281535457322));
#16144=CARTESIAN_POINT('Ctrl Pts',(5.42005904708462,-3.81502573221772,16.7342250638263));
#16145=CARTESIAN_POINT('Ctrl Pts',(5.30290812222079,-3.84272103666939,16.7402965819204));
#16146=CARTESIAN_POINT('Ctrl Pts',(5.18467637083413,-3.86499717719957,16.7463681000145));
#16147=CARTESIAN_POINT('Ctrl Pts',(5.0706927807632,-3.88647291819786,16.7522214636112));
#16148=CARTESIAN_POINT('Ctrl Pts',(4.95570513821216,-3.90291213998371,16.758074827208));
#16149=CARTESIAN_POINT('Ctrl Pts',(4.84019514443961,-3.91423598261409,16.7639281908047));
#16150=CARTESIAN_POINT('Ctrl Pts',(4.72470249410394,-3.92555812500761,16.7697806755387));
#16151=CARTESIAN_POINT('Ctrl Pts',(4.6086880595571,-3.93176637513343,16.7756331602726));
#16152=CARTESIAN_POINT('Ctrl Pts',(4.4926393660822,-3.9328336746297,16.7814856450065));
#16153=CARTESIAN_POINT('Ctrl Pts',(4.37658003250018,-3.93390107198301,16.7873386663346));
#16154=CARTESIAN_POINT('Ctrl Pts',(4.2604868468961,-3.92982657789509,16.7931916876628));
#16155=CARTESIAN_POINT('Ctrl Pts',(4.1448473292717,-3.92063526333841,16.799044708991));
#16156=CARTESIAN_POINT('Ctrl Pts',(4.02916924363496,-3.91144088330082,16.8048996824148));
#16157=CARTESIAN_POINT('Ctrl Pts',(3.91394553846898,-3.89712632209603,16.8107546558386));
#16158=CARTESIAN_POINT('Ctrl Pts',(3.79965790060827,-3.87776843560638,16.8166096292625));
#16159=CARTESIAN_POINT('Ctrl Pts',(3.68524073238977,-3.85838860943883,16.8224712385466));
#16160=CARTESIAN_POINT('Ctrl Pts',(3.57176215656407,-3.83395411830546,16.8283328478308));
#16161=CARTESIAN_POINT('Ctrl Pts',(3.45969306125265,-3.80459281871039,16.8341944571149));
#16162=CARTESIAN_POINT('Ctrl Pts',(3.34754839692717,-3.77521172057537,16.8400600189253));
#16163=CARTESIAN_POINT('Ctrl Pts',(3.23681549927388,-3.74089732076254,16.8459255807356));
#16164=CARTESIAN_POINT('Ctrl Pts',(3.12794784940035,-3.70182661265799,16.851791142546));
#16165=CARTESIAN_POINT('Ctrl Pts',(3.01892100832124,-3.66269877359551,16.8576652812463));
#16166=CARTESIAN_POINT('Ctrl Pts',(2.91176523916443,-3.61880090204656,16.8635394199466));
#16167=CARTESIAN_POINT('Ctrl Pts',(2.80691196447618,-3.57035715806244,16.8694135586469));
#16168=CARTESIAN_POINT('Ctrl Pts',(2.78039628305049,-3.5581065260591,16.8708990324282));
#16169=CARTESIAN_POINT('Ctrl Pts',(2.75402771143118,-3.54556540726136,16.8723845062095));
#16170=CARTESIAN_POINT('Ctrl Pts',(2.72781294149613,-3.5327378708543,16.8738699799907));
#16171=CARTESIAN_POINT('Ctrl Pts',(2.62415751654921,-3.48201670333726,16.8797436693813));
#16172=CARTESIAN_POINT('Ctrl Pts',(2.52256368980246,-3.42664510307157,16.8856173587718));
#16173=CARTESIAN_POINT('Ctrl Pts',(2.42347770034835,-3.36681376729678,16.8914910481624));
#16174=CARTESIAN_POINT('Ctrl Pts',(2.32451964021537,-3.30705967939739,16.8973571540682));
#16175=CARTESIAN_POINT('Ctrl Pts',(2.22806332878527,-3.24285751824533,16.9032232599739));
#16176=CARTESIAN_POINT('Ctrl Pts',(2.13453295918874,-3.1744450742008,16.9090893658797));
#16177=CARTESIAN_POINT('Ctrl Pts',(2.04109836349919,-3.10610268362746,16.9149494649677));
#16178=CARTESIAN_POINT('Ctrl Pts',(1.95058408157798,-3.03355882810684,16.9208095640558));
#16179=CARTESIAN_POINT('Ctrl Pts',(1.86338713317583,-2.95709568345064,16.9266696631438));
#16180=CARTESIAN_POINT('Ctrl Pts',(1.77304431780336,-2.87787392297555,16.9327411812379));
#16181=CARTESIAN_POINT('Ctrl Pts',(1.68626310554974,-2.7944449694587,16.938812699332));
#16182=CARTESIAN_POINT('Ctrl Pts',(1.60344973292686,-2.70717000862967,16.9448842174261));
#16183=CARTESIAN_POINT('Ctrl Pts',(1.52361191096514,-2.62303090689167,16.9507375810229));
#16184=CARTESIAN_POINT('Ctrl Pts',(1.44746200922122,-2.53531774700819,16.9565909446196));
#16185=CARTESIAN_POINT('Ctrl Pts',(1.37532742915778,-2.44439255560169,16.9624443082164));
#16186=CARTESIAN_POINT('Ctrl Pts',(1.30320367985882,-2.35348101630673,16.9682967929503));
#16187=CARTESIAN_POINT('Ctrl Pts',(1.23509431017858,-2.25935872800797,16.9741492776842));
#16188=CARTESIAN_POINT('Ctrl Pts',(1.1712863495637,-2.16242069343123,16.9800017624181));
#16189=CARTESIAN_POINT('Ctrl Pts',(1.10747253861552,-2.06547377093821,16.9858547837463));
#16190=CARTESIAN_POINT('Ctrl Pts',(1.04796114789175,-1.96571093407056,16.9917078050744));
#16191=CARTESIAN_POINT('Ctrl Pts',(0.992995399287234,-1.86355544092402,
16.9975608264026));
#16192=CARTESIAN_POINT('Ctrl Pts',(0.938011318544051,-1.76136587694766,
17.0034157998264));
#16193=CARTESIAN_POINT('Ctrl Pts',(0.887576090189599,-1.65678243353768,
17.0092707732503));
#16194=CARTESIAN_POINT('Ctrl Pts',(0.841886258637142,-1.55025154022579,
17.0151257466741));
#16195=CARTESIAN_POINT('Ctrl Pts',(0.796144643529277,-1.44359990782976,
17.0209873559582));
#16196=CARTESIAN_POINT('Ctrl Pts',(0.755159322920271,-1.33499680003379,
17.0268489652424));
#16197=CARTESIAN_POINT('Ctrl Pts',(0.719078130915673,-1.22490722004846,
17.0327105745265));
#16198=CARTESIAN_POINT('Ctrl Pts',(0.682972609098328,-1.11474340585084,
17.0385761363369));
#16199=CARTESIAN_POINT('Ctrl Pts',(0.651777911533777,-1.00309152050607,
17.0444416981472));
#16200=CARTESIAN_POINT('Ctrl Pts',(0.625591145712266,-0.890428577545389,
17.0503072599576));
#16201=CARTESIAN_POINT('Ctrl Pts',(0.599366088416401,-0.777600893729711,
17.0561813986579));
#16202=CARTESIAN_POINT('Ctrl Pts',(0.578163652735192,-0.663759606354293,
17.0620555373582));
#16203=CARTESIAN_POINT('Ctrl Pts',(0.562029353484096,-0.54938876246601,
17.0679296760586));
#16204=CARTESIAN_POINT('Ctrl Pts',(0.557949252597881,-0.520466243164526,
17.0694151498399));
#16205=CARTESIAN_POINT('Ctrl Pts',(0.554192999669724,-0.491509865733668,
17.0709006236212));
#16206=CARTESIAN_POINT('Ctrl Pts',(0.550760803062122,-0.46252745935487,
17.0723860974024));
#16207=CARTESIAN_POINT('Ctrl Pts',(0.537189606414729,-0.347928565046156,
17.078259786793));
#16208=CARTESIAN_POINT('Ctrl Pts',(0.528643816891126,-0.232541004059473,
17.0841334761836));
#16209=CARTESIAN_POINT('Ctrl Pts',(0.525205100560675,-0.116843133393246,
17.0900071655741));
#16210=CARTESIAN_POINT('Ctrl Pts',(0.52177082393606,-0.00129463954741409,
17.0958732714799));
#16211=CARTESIAN_POINT('Ctrl Pts',(0.523430519936596,0.114562958047589,
17.1017393773857));
#16212=CARTESIAN_POINT('Ctrl Pts',(0.530214330587271,0.23024429815942,17.1076054832914));
#16213=CARTESIAN_POINT('Ctrl Pts',(0.536991194702262,0.345807182052693,
17.1134655823795));
#16214=CARTESIAN_POINT('Ctrl Pts',(0.548881712651152,0.461193757478206,
17.1193256814675));
#16215=CARTESIAN_POINT('Ctrl Pts',(0.565863998068018,0.575917435432653,
17.1251857805555));
#16216=CARTESIAN_POINT('Ctrl Pts',(0.583458965599931,0.694780081961094,
17.1312572986496));
#16217=CARTESIAN_POINT('Ctrl Pts',(0.606520049384706,0.812930644802737,
17.1373288167438));
#16218=CARTESIAN_POINT('Ctrl Pts',(0.634963966896292,0.929831958009547,
17.1434003348379));
#16219=CARTESIAN_POINT('Ctrl Pts',(0.662385871719876,1.04253291360764,17.1492536984346));
#16220=CARTESIAN_POINT('Ctrl Pts',(0.694810342275373,1.15407241182042,17.1551070620314));
#16221=CARTESIAN_POINT('Ctrl Pts',(0.732110652197893,1.26397907655432,17.1609604256281));
#16222=CARTESIAN_POINT('Ctrl Pts',(0.769405361604394,1.37386923917234,17.166812910362));
#16223=CARTESIAN_POINT('Ctrl Pts',(0.811574321966307,1.48212666466751,17.1726653950959));
#16224=CARTESIAN_POINT('Ctrl Pts',(0.858441210786417,1.5882960252089,17.1785178798298));
#16225=CARTESIAN_POINT('Ctrl Pts',(0.905312396670987,1.69447512005519,17.184370901158));
#16226=CARTESIAN_POINT('Ctrl Pts',(0.956882200425629,1.79856539138962,17.1902239224862));
#16227=CARTESIAN_POINT('Ctrl Pts',(1.01292680785358,1.90013300570601,17.1960769438144));
#16228=CARTESIAN_POINT('Ctrl Pts',(1.06899010724043,2.00173449478324,17.2019319172382));
#16229=CARTESIAN_POINT('Ctrl Pts',(1.12953097844474,2.10081129231162,17.207786890662));
#16230=CARTESIAN_POINT('Ctrl Pts',(1.19428083182352,2.19695622678321,17.2136418640858));
#16231=CARTESIAN_POINT('Ctrl Pts',(1.25910407084427,2.29321012918863,17.21950347337));
#16232=CARTESIAN_POINT('Ctrl Pts',(1.32814558244219,2.38652519337785,17.2253650826541));
#16233=CARTESIAN_POINT('Ctrl Pts',(1.40109476304516,2.47652511052879,17.2312266919383));
#16234=CARTESIAN_POINT('Ctrl Pts',(1.47409313381637,2.56658571528485,17.2370922537486));
#16235=CARTESIAN_POINT('Ctrl Pts',(1.55100414698407,2.65332641340697,17.242957815559));
#16236=CARTESIAN_POINT('Ctrl Pts',(1.63147960722877,2.7364070111369,17.2488233773693));
#16237=CARTESIAN_POINT('Ctrl Pts',(1.71207274233427,2.81960909307758,17.2546975160696));
#16238=CARTESIAN_POINT('Ctrl Pts',(1.79624042741247,2.89914011079204,17.26057165477));
#16239=CARTESIAN_POINT('Ctrl Pts',(1.88360058794582,2.97469941131581,17.2664457934703));
#16240=CARTESIAN_POINT('Ctrl Pts',(1.90569254637927,2.99380712490334,17.2679312672516));
#16241=CARTESIAN_POINT('Ctrl Pts',(1.9279885171227,3.01266106132437,17.2694167410328));
#16242=CARTESIAN_POINT('Ctrl Pts',(1.95048203420881,3.03125680121655,17.2709022148141));
#16243=CARTESIAN_POINT('Ctrl Pts',(2.03942330959911,3.10478593481113,17.2767759042047));
#16244=CARTESIAN_POINT('Ctrl Pts',(2.13175162878624,3.17451972307133,17.2826495935952));
#16245=CARTESIAN_POINT('Ctrl Pts',(2.22710929658357,3.24013021947971,17.2885232829858));
#16246=CARTESIAN_POINT('Ctrl Pts',(2.32234384867323,3.30565600657334,17.2943893888916));
#16247=CARTESIAN_POINT('Ctrl Pts',(2.42059963407783,3.36706885657892,17.3002554947973));
#16248=CARTESIAN_POINT('Ctrl Pts',(2.52148514022352,3.42408032197601,17.3061216007031));
#16249=CARTESIAN_POINT('Ctrl Pts',(2.62226734089618,3.48103340835885,17.3119816997911));
#16250=CARTESIAN_POINT('Ctrl Pts',(2.72567354855922,3.53359387279992,17.3178417988791));
#16251=CARTESIAN_POINT('Ctrl Pts',(2.83128301384766,3.58151632205763,17.3237018979672));
#16252=CARTESIAN_POINT('Ctrl Pts',(2.94070262771,3.63116770395598,17.3297734160613));
#16253=CARTESIAN_POINT('Ctrl Pts',(3.05248710567141,3.67583983813406,17.3358449341554));
#16254=CARTESIAN_POINT('Ctrl Pts',(3.16613991472104,3.71531150478263,17.3419164522495));
#16255=CARTESIAN_POINT('Ctrl Pts',(3.27570908751243,3.75336492290354,17.3477698158462));
#16256=CARTESIAN_POINT('Ctrl Pts',(3.38701421701145,3.78658500868856,17.353623179443));
#16257=CARTESIAN_POINT('Ctrl Pts',(3.49959050262001,3.81482271383296,17.3594765430397));
#16258=CARTESIAN_POINT('Ctrl Pts',(3.61214988527817,3.84305617918098,17.3653290277736));
#16259=CARTESIAN_POINT('Ctrl Pts',(3.72597964392154,3.86630865087863,17.3711815125075));
#16260=CARTESIAN_POINT('Ctrl Pts',(3.84060157689801,3.88448145655621,17.3770339972414));
#16261=CARTESIAN_POINT('Ctrl Pts',(3.95523401916669,3.90265592843605,17.3828870185696));
#16262=CARTESIAN_POINT('Ctrl Pts',(4.07065837208287,3.91574974375606,17.3887400398978));
#16263=CARTESIAN_POINT('Ctrl Pts',(4.18638875014219,3.92371579007219,17.3945930612259));
#16264=CARTESIAN_POINT('Ctrl Pts',(4.3021577265176,3.93168449321862,17.4004480346498));
#16265=CARTESIAN_POINT('Ctrl Pts',(4.4182325190412,3.93452199832943,17.4063030080736));
#16266=CARTESIAN_POINT('Ctrl Pts',(4.5341253732997,3.93223327184222,17.4121579814974));
#16267=CARTESIAN_POINT('Ctrl Pts',(4.65014957722265,3.92994195137752,17.4180195907816));
#16268=CARTESIAN_POINT('Ctrl Pts',(4.76599101801497,3.92251281121624,17.4238812000657));
#16269=CARTESIAN_POINT('Ctrl Pts',(4.8811650992699,3.9100028533859,17.4297428093499));
#16270=CARTESIAN_POINT('Ctrl Pts',(4.99641684325361,3.89748445999913,17.4356083711602));
#16271=CARTESIAN_POINT('Ctrl Pts',(5.11099992429715,3.87987848954136,17.4414739329706));
#16272=CARTESIAN_POINT('Ctrl Pts',(5.22443971492151,3.85729311099999,17.4473394947809));
#16273=CARTESIAN_POINT('Ctrl Pts',(5.33804538234267,3.83467470709577,17.4532136334812));
#16274=CARTESIAN_POINT('Ctrl Pts',(5.45050402322474,3.8070624619667,17.4590877721816));
#16275=CARTESIAN_POINT('Ctrl Pts',(5.56135587029248,3.77461444899656,17.4649619108819));
#16276=CARTESIAN_POINT('Ctrl Pts',(5.58938849274594,3.76640887623419,17.4664473846632));
#16277=CARTESIAN_POINT('Ctrl Pts',(5.61731846126856,3.75789429531119,17.4679328584444));
#16278=CARTESIAN_POINT('Ctrl Pts',(5.64513855697309,3.74907374385224,17.4694183322257));
#16279=CARTESIAN_POINT('Ctrl Pts',(5.75514157624099,3.71419653485922,17.4752920216163));
#16280=CARTESIAN_POINT('Ctrl Pts',(5.86379148569802,3.6744156735816,17.4811657110068));
#16281=CARTESIAN_POINT('Ctrl Pts',(5.97061879934942,3.62985395116536,17.4870394003974));
#16282=CARTESIAN_POINT('Ctrl Pts',(6.07730818890302,3.58534976211912,17.4929055063032));
#16283=CARTESIAN_POINT('Ctrl Pts',(6.18217928446147,3.53607714469648,17.4987716122089));
#16284=CARTESIAN_POINT('Ctrl Pts',(6.28477745861988,3.48220871984125,17.5046377181147));
#16285=CARTESIAN_POINT('Ctrl Pts',(6.38727057355486,3.4283954555669,17.5104978172027));
#16286=CARTESIAN_POINT('Ctrl Pts',(6.48749503294883,3.36999593549452,17.5163579162907));
#16287=CARTESIAN_POINT('Ctrl Pts',(6.58501653870268,3.30723068860701,17.5222180153788));
#16288=CARTESIAN_POINT('Ctrl Pts',(6.68605639790208,3.24220101480216,17.5282895334729));
#16289=CARTESIAN_POINT('Ctrl Pts',(6.78419417148932,3.17248482959048,17.534361051567));
#16290=CARTESIAN_POINT('Ctrl Pts',(6.87897479145501,3.09837944819475,17.5404325696611));
#16291=CARTESIAN_POINT('Ctrl Pts',(6.97034986799851,3.02693673237615,17.5462859332579));
#16292=CARTESIAN_POINT('Ctrl Pts',(7.05860453609393,2.95141508308455,17.5521392968546));
#16293=CARTESIAN_POINT('Ctrl Pts',(7.14336157645623,2.87212427540636,17.5579926604514));
#16294=CARTESIAN_POINT('Ctrl Pts',(7.22810589083405,2.79284537297619,17.5638451451853));
#16295=CARTESIAN_POINT('Ctrl Pts',(7.30935332006476,2.70979871960462,17.5696976299192));
#16296=CARTESIAN_POINT('Ctrl Pts',(7.38676171131797,2.62333266066238,17.5755501146531));
#16297=CARTESIAN_POINT('Ctrl Pts',(7.4641771998814,2.53685867394338,17.5814031359812));
#16298=CARTESIAN_POINT('Ctrl Pts',(7.53775267516254,2.44696496624974,17.5872561573094));
#16299=CARTESIAN_POINT('Ctrl Pts',(7.60718514505177,2.35403429087964,17.5931091786376));
#16300=CARTESIAN_POINT('Ctrl Pts',(7.6766407720106,2.26107262133462,17.5989641520614));
#16301=CARTESIAN_POINT('Ctrl Pts',(7.74195039883708,2.16507230082249,17.6048191254852));
#16302=CARTESIAN_POINT('Ctrl Pts',(7.80285378256125,2.06644588555732,17.610674098909));
#16303=CARTESIAN_POINT('Ctrl Pts',(7.86382619244812,1.96770768991853,17.6165357081932));
#16304=CARTESIAN_POINT('Ctrl Pts',(7.92038217449507,1.86633781064922,17.6223973174773));
#16305=CARTESIAN_POINT('Ctrl Pts',(7.972306923632,1.762774359254,17.6282589267615));
#16306=CARTESIAN_POINT('Ctrl Pts',(8.02426668600853,1.65914107426309,17.6341244885718));
#16307=CARTESIAN_POINT('Ctrl Pts',(8.07158882890953,1.55331164806977,17.6399900503822));
#16308=CARTESIAN_POINT('Ctrl Pts',(8.11410694751338,1.44574355330601,17.6458556121925));
#16309=CARTESIAN_POINT('Ctrl Pts',(8.15668723803494,1.33801816760475,17.6517297508928));
#16310=CARTESIAN_POINT('Ctrl Pts',(8.19444935059135,1.2285494284808,17.6576038895932));
#16311=CARTESIAN_POINT('Ctrl Pts',(8.22727687127466,1.11780937506817,17.6634780282935));
#16312=CARTESIAN_POINT('Ctrl Pts',(8.23557841534231,1.08980502340459,17.6649635020748));
#16313=CARTESIAN_POINT('Ctrl Pts',(8.24356464775546,1.06171941638178,17.6664489758561));
#16314=CARTESIAN_POINT('Ctrl Pts',(8.25123420762655,1.03356026681257,17.6679344496374));
#16315=CARTESIAN_POINT('Ctrl Pts',(8.28989601302147,0.891611631032941,17.6754226366021));
#16316=CARTESIAN_POINT('Ctrl Pts',(8.32061081407376,0.747412562252989,17.6829108235669));
#16317=CARTESIAN_POINT('Ctrl Pts',(8.34316333708667,0.601744925806739,17.6903990105316));
#16318=CARTESIAN_POINT('Ctrl Pts',(8.36531050155811,0.458695516182177,17.6977526049923));
#16319=CARTESIAN_POINT('Ctrl Pts',(8.37958618475085,0.314229690772142,17.7051061994529));
#16320=CARTESIAN_POINT('Ctrl Pts',(8.38583177918674,0.169109385552526,17.7124597939135));
#16321=CARTESIAN_POINT('Ctrl Pts',(8.38820328930776,0.114005859999161,17.7152520219181));
#16322=CARTESIAN_POINT('Ctrl Pts',(8.38941749976572,0.0588082088045671,
17.7180442499227));
#16323=CARTESIAN_POINT('Ctrl Pts',(8.38946749588772,0.00355905287639466,
17.7208364779273));
#16324=CARTESIAN_POINT('',(8.38850524290982,-0.00312121602759044,15.2208368624451));
#16325=CARTESIAN_POINT('Ctrl Pts',(8.38601483107283,-0.00313894636463737,
15.2208378571301));
#16326=CARTESIAN_POINT('Ctrl Pts',(8.38918468738173,-0.431668147948809,
15.2424722516526));
#16327=CARTESIAN_POINT('Ctrl Pts',(8.12699578129889,-2.16714071178393,15.3302786853124));
#16328=CARTESIAN_POINT('Ctrl Pts',(5.59178989108131,-4.50829591265121,15.4842571581091));
#16329=CARTESIAN_POINT('Ctrl Pts',(1.28358086881555,-3.3980090573042,15.6827732755208));
#16330=CARTESIAN_POINT('Ctrl Pts',(-0.118957460370758,0.824109855735944,
15.8812893929325));
#16331=CARTESIAN_POINT('Ctrl Pts',(2.66859282628323,4.29152463912485,16.0798055103441));
#16332=CARTESIAN_POINT('Ctrl Pts',(7.04885138217592,3.83350581901215,16.2763209308836));
#16333=CARTESIAN_POINT('Ctrl Pts',(8.39253775623418,1.26226890306036,16.4066643122856));
#16334=CARTESIAN_POINT('Ctrl Pts',(8.3957692530271,-0.000714131161949812,
16.4708356545507));
#16335=CARTESIAN_POINT('',(8.38779848858743,0.00244925732166319,13.97083596737));
#16336=CARTESIAN_POINT('Ctrl Pts',(8.3894683492347,0.00244017049050211,
13.970836477965));
#16337=CARTESIAN_POINT('Ctrl Pts',(8.38954098951505,-0.114639422405106,
13.9767346357567));
#16338=CARTESIAN_POINT('Ctrl Pts',(8.38438136405865,-0.231739061658239,
13.9826327935484));
#16339=CARTESIAN_POINT('Ctrl Pts',(8.37401070864951,-0.348363019306455,
13.9885309513401));
#16340=CARTESIAN_POINT('Ctrl Pts',(8.36363894134007,-0.464999480910128,
13.9944297415087));
#16341=CARTESIAN_POINT('Ctrl Pts',(8.34805506770137,-0.581159756869867,
14.0003285316773));
#16342=CARTESIAN_POINT('Ctrl Pts',(8.32733222229877,-0.696353169424395,
14.0062273218459));
#16343=CARTESIAN_POINT('Ctrl Pts',(8.3066024391392,-0.811585147334493,14.0121280868579));
#16344=CARTESIAN_POINT('Ctrl Pts',(8.28073033206417,-0.925849220138849,
14.0180288518698));
#16345=CARTESIAN_POINT('Ctrl Pts',(8.24984005631773,-1.03866541048662,14.0239296168817));
#16346=CARTESIAN_POINT('Ctrl Pts',(8.21891015066804,-1.15162633553168,14.0298379521319));
#16347=CARTESIAN_POINT('Ctrl Pts',(8.18294932296882,-1.26313527712322,14.0357462873821));
#16348=CARTESIAN_POINT('Ctrl Pts',(8.14213163441006,-1.37272747779112,14.0416546226322));
#16349=CARTESIAN_POINT('Ctrl Pts',(8.10128765710371,-1.48239026162536,14.0475667631624));
#16350=CARTESIAN_POINT('Ctrl Pts',(8.0555807437954,-1.59013347291978,14.0534789036926));
#16351=CARTESIAN_POINT('Ctrl Pts',(8.00523238555656,-1.69551413654383,14.0593910442228));
#16352=CARTESIAN_POINT('Ctrl Pts',(7.95479113524709,-1.80108922613115,14.0653140925758));
#16353=CARTESIAN_POINT('Ctrl Pts',(7.89969151625316,-1.90429269979155,14.0712371409289));
#16354=CARTESIAN_POINT('Ctrl Pts',(7.8402004918376,-2.00470718808871,14.077160189282));
#16355=CARTESIAN_POINT('Ctrl Pts',(7.78166363993183,-2.10351113521166,14.0829882382639));
#16356=CARTESIAN_POINT('Ctrl Pts',(7.71887548050658,-2.19961464379018,14.0888162872457));
#16357=CARTESIAN_POINT('Ctrl Pts',(7.65212862443776,-2.29265113866306,14.0946443362276));
#16358=CARTESIAN_POINT('Ctrl Pts',(7.58485906277745,-2.38641621760638,14.1005180256182));
#16359=CARTESIAN_POINT('Ctrl Pts',(7.51334717067436,-2.47737427957379,14.1063917150087));
#16360=CARTESIAN_POINT('Ctrl Pts',(7.43785527256591,-2.56511705914385,14.1122654043993));
#16361=CARTESIAN_POINT('Ctrl Pts',(7.36246084159014,-2.65274655454233,14.118131510305));
#16362=CARTESIAN_POINT('Ctrl Pts',(7.28309689051695,-2.73716871266051,14.1239976162108));
#16363=CARTESIAN_POINT('Ctrl Pts',(7.20006850960705,-2.8180048462919,14.1298637221165));
#16364=CARTESIAN_POINT('Ctrl Pts',(7.11712514870153,-2.89875820475219,14.1357238212046));
#16365=CARTESIAN_POINT('Ctrl Pts',(7.03052511591363,-2.97593255623383,14.1415839202926));
#16366=CARTESIAN_POINT('Ctrl Pts',(6.9406127438482,-3.04918339684949,14.1474440193806));
#16367=CARTESIAN_POINT('Ctrl Pts',(6.84745653852143,-3.12507696068279,14.1535155374747));
#16368=CARTESIAN_POINT('Ctrl Pts',(6.75074477271872,-3.19675822350967,14.1595870555688));
#16369=CARTESIAN_POINT('Ctrl Pts',(6.6509012207872,-3.26388674658733,14.1656585736629));
#16370=CARTESIAN_POINT('Ctrl Pts',(6.5546451274696,-3.328603288183,14.1715119372597));
#16371=CARTESIAN_POINT('Ctrl Pts',(6.45547880226965,-3.38908837641713,14.1773653008564));
#16372=CARTESIAN_POINT('Ctrl Pts',(6.35381372451471,-3.44507944747599,14.1832186644532));
#16373=CARTESIAN_POINT('Ctrl Pts',(6.25216391142903,-3.50106211166396,14.1890711491871));
#16374=CARTESIAN_POINT('Ctrl Pts',(6.1480164535795,-3.55255190110159,14.194923633921));
#16375=CARTESIAN_POINT('Ctrl Pts',(6.04180862524011,-3.59933155036147,14.2007761186549));
#16376=CARTESIAN_POINT('Ctrl Pts',(5.93559105906875,-3.64611548868715,14.2066291399831));
#16377=CARTESIAN_POINT('Ctrl Pts',(5.82731312499075,-3.68818826180218,14.2124821613113));
#16378=CARTESIAN_POINT('Ctrl Pts',(5.71743266543329,-3.72538050436888,14.2183351826394));
#16379=CARTESIAN_POINT('Ctrl Pts',(5.60751555862045,-3.76258515126677,14.2241901560633));
#16380=CARTESIAN_POINT('Ctrl Pts',(5.49599525467625,-3.79490589851833,14.2300451294871));
#16381=CARTESIAN_POINT('Ctrl Pts',(5.38334467341555,-3.82222326440158,14.2359001029109));
#16382=CARTESIAN_POINT('Ctrl Pts',(5.27056641719066,-3.84957159101021,14.2417617121951));
#16383=CARTESIAN_POINT('Ctrl Pts',(5.15665572853512,-3.87190512047574,14.2476233214792));
#16384=CARTESIAN_POINT('Ctrl Pts',(5.04209573263636,-3.88915549373256,14.2534849307634));
#16385=CARTESIAN_POINT('Ctrl Pts',(4.92745848809112,-3.90641749904273,14.2593504925737));
#16386=CARTESIAN_POINT('Ctrl Pts',(4.81217147432536,-3.91858947974188,14.2652160543841));
#16387=CARTESIAN_POINT('Ctrl Pts',(4.69672121446205,-3.92565509494713,14.2710816161944));
#16388=CARTESIAN_POINT('Ctrl Pts',(4.58110213800274,-3.93273104181478,14.2769557548947));
#16389=CARTESIAN_POINT('Ctrl Pts',(4.46531975054712,-3.93468571446805,14.2828298935951));
#16390=CARTESIAN_POINT('Ctrl Pts',(4.34985892161933,-3.93155481566005,14.2887040322954));
#16391=CARTESIAN_POINT('Ctrl Pts',(4.32066076289567,-3.93076306246382,14.2901895060767));
#16392=CARTESIAN_POINT('Ctrl Pts',(4.29148313157325,-3.92964634388687,14.2916749798579));
#16393=CARTESIAN_POINT('Ctrl Pts',(4.26233378226808,-3.92820575784858,14.2931604536392));
#16394=CARTESIAN_POINT('Ctrl Pts',(4.14707478146079,-3.92250955840302,14.2990341430298));
#16395=CARTESIAN_POINT('Ctrl Pts',(4.03187473136373,-3.91172678479576,14.3049078324204));
#16396=CARTESIAN_POINT('Ctrl Pts',(3.91721890918676,-3.89585654574209,14.3107815218109));
#16397=CARTESIAN_POINT('Ctrl Pts',(3.8027111184477,-3.88000679665798,14.3166476277167));
#16398=CARTESIAN_POINT('Ctrl Pts',(3.68874656379495,-3.85908270064171,14.3225137336224));
#16399=CARTESIAN_POINT('Ctrl Pts',(3.57580885139183,-3.8331353374971,14.3283798395282));
#16400=CARTESIAN_POINT('Ctrl Pts',(3.46298678576733,-3.80721454412178,14.3342399386162));
#16401=CARTESIAN_POINT('Ctrl Pts',(3.35118987118612,-3.77628080694593,14.3401000377043));
#16402=CARTESIAN_POINT('Ctrl Pts',(3.24089426294817,-3.74043671252554,14.3459601367923));
#16403=CARTESIAN_POINT('Ctrl Pts',(3.12661944078964,-3.70329944495197,14.3520316548864));
#16404=CARTESIAN_POINT('Ctrl Pts',(3.01395674507062,-3.66089088357044,14.3581031729805));
#16405=CARTESIAN_POINT('Ctrl Pts',(2.90342198124228,-3.61338257420991,14.3641746910746));
#16406=CARTESIAN_POINT('Ctrl Pts',(2.79685881981555,-3.56758127637244,14.3700280546714));
#16407=CARTESIAN_POINT('Ctrl Pts',(2.69227371747094,-3.51704057673436,14.3758814182681));
#16408=CARTESIAN_POINT('Ctrl Pts',(2.59011037549847,-3.46196390626275,14.3817347818649));
#16409=CARTESIAN_POINT('Ctrl Pts',(2.48796237300794,-3.40689550536784,14.3875872665988));
#16410=CARTESIAN_POINT('Ctrl Pts',(2.38823577144503,-3.3472926838444,14.3934397513327));
#16411=CARTESIAN_POINT('Ctrl Pts',(2.29135019119615,-3.28340510504164,14.3992922360666));
#16412=CARTESIAN_POINT('Ctrl Pts',(2.19445572784055,-3.21951166860579,14.4051452573948));
#16413=CARTESIAN_POINT('Ctrl Pts',(2.10040314854254,-3.15133292138124,14.4109982787229));
#16414=CARTESIAN_POINT('Ctrl Pts',(2.00958297305876,-3.07916177739198,14.4168513000511));
#16415=CARTESIAN_POINT('Ctrl Pts',(1.91873250729247,-3.00696656293238,14.4227062734749));
#16416=CARTESIAN_POINT('Ctrl Pts',(1.83111691231099,-2.93077656089362,14.4285612468987));
#16417=CARTESIAN_POINT('Ctrl Pts',(1.7470929638725,-2.85092439732934,14.4344162203226));
#16418=CARTESIAN_POINT('Ctrl Pts',(1.66297378508079,-2.77098173159415,14.4402778296067));
#16419=CARTESIAN_POINT('Ctrl Pts',(1.58245467728933,-2.687368904774,14.4461394388909));
#16420=CARTESIAN_POINT('Ctrl Pts',(1.50585498991652,-2.60045483265542,14.452001048175));
#16421=CARTESIAN_POINT('Ctrl Pts',(1.42920365081196,-2.51348215373971,14.4578666099854));
#16422=CARTESIAN_POINT('Ctrl Pts',(1.35647725325612,-2.42320411789621,14.4637321717957));
#16423=CARTESIAN_POINT('Ctrl Pts',(1.28795327743338,-2.33002069577498,14.4695977336061));
#16424=CARTESIAN_POINT('Ctrl Pts',(1.21932910275137,-2.23670101663586,14.4754718723064));
#16425=CARTESIAN_POINT('Ctrl Pts',(1.15491984253505,-2.1404678145249,14.4813460110067));
#16426=CARTESIAN_POINT('Ctrl Pts',(1.09495834786145,-2.04174788391013,14.4872201497071));
#16427=CARTESIAN_POINT('Ctrl Pts',(1.07979506473727,-2.01678322507266,14.4887056234884));
#16428=CARTESIAN_POINT('Ctrl Pts',(1.06491598067201,-1.99165964874789,14.4901910972696));
#16429=CARTESIAN_POINT('Ctrl Pts',(1.05032437692652,-1.96638426639306,14.4916765710509));
#16430=CARTESIAN_POINT('Ctrl Pts',(0.99262793745291,-1.86644325965767,14.4975502604415));
#16431=CARTESIAN_POINT('Ctrl Pts',(0.939237743903457,-1.76379430943517,
14.503423949832));
#16432=CARTESIAN_POINT('Ctrl Pts',(0.89041761862265,-1.65884471479919,14.5092976392226));
#16433=CARTESIAN_POINT('Ctrl Pts',(0.841660524710002,-1.5540306199494,14.5151637451284));
#16434=CARTESIAN_POINT('Ctrl Pts',(0.797461937793022,-1.44692215891174,
14.5210298510341));
#16435=CARTESIAN_POINT('Ctrl Pts',(0.75804110261241,-1.33795340058767,14.5268959569399));
#16436=CARTESIAN_POINT('Ctrl Pts',(0.718660633864798,-1.22909622488385,
14.5327560560279));
#16437=CARTESIAN_POINT('Ctrl Pts',(0.684048325261163,-1.11838292713387,
14.538616155116));
#16438=CARTESIAN_POINT('Ctrl Pts',(0.6543761008303,-1.00626923752046,14.544476254204));
#16439=CARTESIAN_POINT('Ctrl Pts',(0.62363337023519,-0.890110741758223,
14.5505477722981));
#16440=CARTESIAN_POINT('Ctrl Pts',(0.59819409826764,-0.772449309985185,
14.5566192903922));
#16441=CARTESIAN_POINT('Ctrl Pts',(0.578193756662317,-0.65381137419503,
14.5626908084863));
#16442=CARTESIAN_POINT('Ctrl Pts',(0.558912043314759,-0.53943619425096,
14.5685441720831));
#16443=CARTESIAN_POINT('Ctrl Pts',(0.544685211133058,-0.424153918083215,
14.5743975356798));
#16444=CARTESIAN_POINT('Ctrl Pts',(0.535582850168585,-0.308447673229725,
14.5802508992765));
#16445=CARTESIAN_POINT('Ctrl Pts',(0.52648185589297,-0.192758801279415,
14.5861033840104));
#16446=CARTESIAN_POINT('Ctrl Pts',(0.522503835326865,-0.0766464989801795,
14.5919558687443));
#16447=CARTESIAN_POINT('Ctrl Pts',(0.523666474601265,0.0394012784882832,
14.5978083534783));
#16448=CARTESIAN_POINT('Ctrl Pts',(0.524829220474074,0.155459695979616,
14.6036613748064));
#16449=CARTESIAN_POINT('Ctrl Pts',(0.53113355900714,0.271453163732685,14.6095143961346));
#16450=CARTESIAN_POINT('Ctrl Pts',(0.542545056721865,0.386894733453194,
14.6153674174627));
#16451=CARTESIAN_POINT('Ctrl Pts',(0.553960360391488,0.502374805166933,
14.6212223908866));
#16452=CARTESIAN_POINT('Ctrl Pts',(0.570486169631157,0.617302201916618,
14.6270773643104));
#16453=CARTESIAN_POINT('Ctrl Pts',(0.5920363876896,0.731196802485668,14.6329323377342));
#16454=CARTESIAN_POINT('Ctrl Pts',(0.613611030152174,0.845220487955169,
14.6387939470184));
#16455=CARTESIAN_POINT('Ctrl Pts',(0.640221370504495,0.958208634743751,
14.6446555563025));
#16456=CARTESIAN_POINT('Ctrl Pts',(0.671730528273218,1.0696928982725,14.6505171655867));
#16457=CARTESIAN_POINT('Ctrl Pts',(0.703260932898381,1.18125233645872,14.656382727397));
#16458=CARTESIAN_POINT('Ctrl Pts',(0.73969660303148,1.29130548088959,14.6622482892074));
#16459=CARTESIAN_POINT('Ctrl Pts',(0.780851864843685,1.39940233489516,14.6681138510177));
#16460=CARTESIAN_POINT('Ctrl Pts',(0.822067305742706,1.50765725301394,14.673987989718));
#16461=CARTESIAN_POINT('Ctrl Pts',(0.868015948077903,1.61394979394547,14.6798621284184));
#16462=CARTESIAN_POINT('Ctrl Pts',(0.918465383892158,1.71785292176214,14.6857362671187));
#16463=CARTESIAN_POINT('Ctrl Pts',(0.931223222616284,1.74412832655552,14.6872217409));
#16464=CARTESIAN_POINT('Ctrl Pts',(0.9442686679649,1.77025106733085,14.6887072146812));
#16465=CARTESIAN_POINT('Ctrl Pts',(0.957597522927404,1.79621453163029,14.6901926884625));
#16466=CARTESIAN_POINT('Ctrl Pts',(1.01030094655475,1.89887627276679,14.6960663778531));
#16467=CARTESIAN_POINT('Ctrl Pts',(1.06761433321634,1.99938744358087,14.7019400672437));
#16468=CARTESIAN_POINT('Ctrl Pts',(1.1293384469066,2.09730555138455,14.7078137566342));
#16469=CARTESIAN_POINT('Ctrl Pts',(1.19098286896731,2.19509723771196,14.71367986254));
#16470=CARTESIAN_POINT('Ctrl Pts',(1.25702647493838,2.29030217257155,14.7195459684457));
#16471=CARTESIAN_POINT('Ctrl Pts',(1.32722336797488,2.38250081000735,14.7254120743515));
#16472=CARTESIAN_POINT('Ctrl Pts',(1.39734838028703,2.47460503721279,14.7312721734395));
#16473=CARTESIAN_POINT('Ctrl Pts',(1.47161797148397,2.56370876344736,14.7371322725275));
#16474=CARTESIAN_POINT('Ctrl Pts',(1.54974238956812,2.64942046393402,14.7429923716155));
#16475=CARTESIAN_POINT('Ctrl Pts',(1.63068535842668,2.73822444703484,14.7490638897097));
#16476=CARTESIAN_POINT('Ctrl Pts',(1.71576631157221,2.82338664813948,14.7551354078038));
#16477=CARTESIAN_POINT('Ctrl Pts',(1.80461632458522,2.90450784549555,14.7612069258979));
#16478=CARTESIAN_POINT('Ctrl Pts',(1.89027388562354,2.98271429340019,14.7670602894946));
#16479=CARTESIAN_POINT('Ctrl Pts',(1.97943398589382,3.05716483048471,14.7729136530914));
#16480=CARTESIAN_POINT('Ctrl Pts',(2.07172837496346,3.12753907164953,14.7787670166882));
#16481=CARTESIAN_POINT('Ctrl Pts',(2.1640089063411,3.1979027463588,14.7846195014221));
#16482=CARTESIAN_POINT('Ctrl Pts',(2.25942246233626,3.26419109167836,14.790471986156));
#16483=CARTESIAN_POINT('Ctrl Pts',(2.35756859820218,3.32612472066967,14.7963244708899));
#16484=CARTESIAN_POINT('Ctrl Pts',(2.45572373275119,3.38806402814333,14.8021774922181));
#16485=CARTESIAN_POINT('Ctrl Pts',(2.55661159580834,3.44564760508657,14.8080305135462));
#16486=CARTESIAN_POINT('Ctrl Pts',(2.65980433418451,3.49864040691994,14.8138835348744));
#16487=CARTESIAN_POINT('Ctrl Pts',(2.76303148933148,3.55165088287598,14.8197385082983));
#16488=CARTESIAN_POINT('Ctrl Pts',(2.86856468104479,3.60006735054383,14.8255934817221));
#16489=CARTESIAN_POINT('Ctrl Pts',(2.97595378583079,3.64370187942126,14.8314484551459));
#16490=CARTESIAN_POINT('Ctrl Pts',(3.08346460237365,3.68738586243261,14.8373100644301));
#16491=CARTESIAN_POINT('Ctrl Pts',(3.19283514735745,3.72627693362311,14.8431716737142));
#16492=CARTESIAN_POINT('Ctrl Pts',(3.30359766295086,3.76023622067798,14.8490332829984));
#16493=CARTESIAN_POINT('Ctrl Pts',(3.41443486652191,3.79421840672948,14.8548988448087));
#16494=CARTESIAN_POINT('Ctrl Pts',(3.52666551071602,3.82326208351088,14.8607644066191));
#16495=CARTESIAN_POINT('Ctrl Pts',(3.63981080425168,3.84727932672286,14.8666299684294));
#16496=CARTESIAN_POINT('Ctrl Pts',(3.75312154395694,3.87133168903498,14.8725041071297));
#16497=CARTESIAN_POINT('Ctrl Pts',(3.86734919622866,3.89034288170052,14.8783782458301));
#16498=CARTESIAN_POINT('Ctrl Pts',(3.98200892886182,3.90427669871167,14.8842523845304));
#16499=CARTESIAN_POINT('Ctrl Pts',(4.01100450341064,3.90780033356254,14.8857378583117));
#16500=CARTESIAN_POINT('Ctrl Pts',(4.04002770747369,3.91099952969375,14.887223332093));
#16501=CARTESIAN_POINT('Ctrl Pts',(4.06907070931136,3.91387422920998,14.8887088058742));
#16502=CARTESIAN_POINT('Ctrl Pts',(4.18390920320717,3.92524103504815,14.8945824952648));
#16503=CARTESIAN_POINT('Ctrl Pts',(4.29943966079135,3.93156820814744,14.9004561846554));
#16504=CARTESIAN_POINT('Ctrl Pts',(4.41518224425229,3.93278328859207,14.906329874046));
#16505=CARTESIAN_POINT('Ctrl Pts',(4.53077539316417,3.93399680025369,14.9121959799517));
#16506=CARTESIAN_POINT('Ctrl Pts',(4.64657971395735,3.93011134058083,14.9180620858574));
#16507=CARTESIAN_POINT('Ctrl Pts',(4.7621093558544,3.92110609876886,14.9239281917632));
#16508=CARTESIAN_POINT('Ctrl Pts',(4.87752069687014,3.91211007820977,14.9297882908512));
#16509=CARTESIAN_POINT('Ctrl Pts',(4.99265750900708,3.89800473537631,14.9356483899392));
#16510=CARTESIAN_POINT('Ctrl Pts',(5.10703371360898,3.87882130184036,14.9415084890273));
#16511=CARTESIAN_POINT('Ctrl Pts',(5.22553635073912,3.85894577378684,14.9475800071214));
#16512=CARTESIAN_POINT('Ctrl Pts',(5.34322201051843,3.83361882040822,14.9536515252155));
#16513=CARTESIAN_POINT('Ctrl Pts',(5.45955522633896,3.80293402988025,14.9597230433096));
#16514=CARTESIAN_POINT('Ctrl Pts',(5.57170849674366,3.77335176839867,14.9655764069064));
#16515=CARTESIAN_POINT('Ctrl Pts',(5.68260440564314,3.73879018073727,14.9714297705031));
#16516=CARTESIAN_POINT('Ctrl Pts',(5.79177409886216,3.69938502681463,14.9772831340998));
#16517=CARTESIAN_POINT('Ctrl Pts',(5.90092740061891,3.65998578944331,14.9831356188337));
#16518=CARTESIAN_POINT('Ctrl Pts',(6.00835461355294,3.61574457207778,14.9889881035676));
#16519=CARTESIAN_POINT('Ctrl Pts',(6.11360388172153,3.56684641326449,14.9948405883015));
#16520=CARTESIAN_POINT('Ctrl Pts',(6.21886279983567,3.51794377114619,15.0006936096297));
#16521=CARTESIAN_POINT('Ctrl Pts',(6.32194300152003,3.46438351287028,15.0065466309579));
#16522=CARTESIAN_POINT('Ctrl Pts',(6.42241503368695,3.40639774692699,15.0123996522861));
#16523=CARTESIAN_POINT('Ctrl Pts',(6.52292057521672,3.34839264161104,15.0182546257099));
#16524=CARTESIAN_POINT('Ctrl Pts',(6.62081585988714,3.28595930008577,15.0241095991338));
#16525=CARTESIAN_POINT('Ctrl Pts',(6.7156989519954,3.21937408574241,15.0299645725576));
#16526=CARTESIAN_POINT('Ctrl Pts',(6.81068958190116,3.15271340561123,15.0358261818417));
#16527=CARTESIAN_POINT('Ctrl Pts',(6.90266086686863,3.08189169799395,15.0416877911259));
#16528=CARTESIAN_POINT('Ctrl Pts',(6.99124253543272,3.00722673946418,15.0475494004101));
#16529=CARTESIAN_POINT('Ctrl Pts',(7.07988393526634,2.93251143380462,15.0534149622204));
#16530=CARTESIAN_POINT('Ctrl Pts',(7.16513086442159,2.85394799620938,15.0592805240307));
#16531=CARTESIAN_POINT('Ctrl Pts',(7.24664988211231,2.77189109415057,15.0651460858411));
#16532=CARTESIAN_POINT('Ctrl Pts',(7.32828810060065,2.68971420477527,15.0710202245414));
#16533=CARTESIAN_POINT('Ctrl Pts',(7.40618725169891,2.60403396056314,15.0768943632417));
#16534=CARTESIAN_POINT('Ctrl Pts',(7.48005407906505,2.51523814219947,15.082768501942));
#16535=CARTESIAN_POINT('Ctrl Pts',(7.49873379382105,2.49278312933778,15.0842539757233));
#16536=CARTESIAN_POINT('Ctrl Pts',(7.51715585839743,2.47012901786282,15.0857394495046));
#16537=CARTESIAN_POINT('Ctrl Pts',(7.53531597848376,2.44728235746121,15.0872249232859));
#16538=CARTESIAN_POINT('Ctrl Pts',(7.60699321998688,2.35710753552386,15.093088026749));
#16539=CARTESIAN_POINT('Ctrl Pts',(7.67483038428635,2.26362391034172,15.098951130212));
#16540=CARTESIAN_POINT('Ctrl Pts',(7.73850576221524,2.16719274377987,15.1048142336751));
#16541=CARTESIAN_POINT('Ctrl Pts',(7.80210141413587,2.07088231575513,15.1106699961242));
#16542=CARTESIAN_POINT('Ctrl Pts',(7.86154541167449,1.97163202414246,15.1165257585734));
#16543=CARTESIAN_POINT('Ctrl Pts',(7.91655588661019,1.86983648273238,15.1223815210225));
#16544=CARTESIAN_POINT('Ctrl Pts',(7.97151088479885,1.76814359968883,15.1282313780754));
#16545=CARTESIAN_POINT('Ctrl Pts',(8.0220410543321,1.66391093219982,15.1340812351284));
#16546=CARTESIAN_POINT('Ctrl Pts',(8.06790791255176,1.55756179591964,15.1399310921813));
#16547=CARTESIAN_POINT('Ctrl Pts',(8.11373968553886,1.45129400997222,15.1457764744652));
#16548=CARTESIAN_POINT('Ctrl Pts',(8.15491507826354,1.34291335396013,15.1516218567491));
#16549=CARTESIAN_POINT('Ctrl Pts',(8.19124197953134,1.23286681550144,15.157467239033));
#16550=CARTESIAN_POINT('Ctrl Pts',(8.22755295518617,1.12286852114066,15.1633100587175));
#16551=CARTESIAN_POINT('Ctrl Pts',(8.25901953475836,1.01120618864942,15.169152878402));
#16552=CARTESIAN_POINT('Ctrl Pts',(8.28549833137557,0.89834525261235,15.1749956980865));
#16553=CARTESIAN_POINT('Ctrl Pts',(8.31197003508108,0.785514548789573,15.1808369526468));
#16554=CARTESIAN_POINT('Ctrl Pts',(8.33345652218681,0.671486283928796,15.1866782072072));
#16555=CARTESIAN_POINT('Ctrl Pts',(8.34986493302147,0.556738660262869,15.1925194617675));
#16556=CARTESIAN_POINT('Ctrl Pts',(8.36627724229281,0.441963773972303,15.1983621041381));
#16557=CARTESIAN_POINT('Ctrl Pts',(8.37760900470372,0.326469597483212,15.2042047465087));
#16558=CARTESIAN_POINT('Ctrl Pts',(8.38381896595424,0.210741735856192,15.2100473888793));
#16559=CARTESIAN_POINT('Ctrl Pts',(8.38764142737385,0.139506945751002,15.2136437519079));
#16560=CARTESIAN_POINT('Ctrl Pts',(8.38952433087012,0.0681837294481043,
15.2172401149364));
#16561=CARTESIAN_POINT('Ctrl Pts',(8.38946787315746,-0.00311436263953271,
15.220836477965));
#16562=CARTESIAN_POINT('',(8.39488259067608,0.00183385008468958,12.720836477965));
#16563=CARTESIAN_POINT('Ctrl Pts',(8.39488259067608,0.00183385008468958,
12.720836477965));
#16564=CARTESIAN_POINT('Ctrl Pts',(8.38794844153403,-1.19755615080374,12.7817401958959));
#16565=CARTESIAN_POINT('Ctrl Pts',(7.16216767756852,-3.71234879616597,12.908815952964));
#16566=CARTESIAN_POINT('Ctrl Pts',(2.88215862231082,-4.37438359324252,13.1020637491693));
#16567=CARTESIAN_POINT('Ctrl Pts',(-0.0728084404743118,-1.04848949713193,
13.3005798665811));
#16568=CARTESIAN_POINT('Ctrl Pts',(1.12005071800708,3.23759133606708,13.4990959839926));
#16569=CARTESIAN_POINT('Ctrl Pts',(5.36833837100506,4.55874760921314,13.6976121014044));
#16570=CARTESIAN_POINT('Ctrl Pts',(8.07197562134217,2.29834034645692,13.8548584366129));
#16571=CARTESIAN_POINT('Ctrl Pts',(8.38739215187287,0.496171455525351,13.9459327326844));
#16572=CARTESIAN_POINT('Ctrl Pts',(8.38460083020223,0.00246665792446467,
13.9708349896186));
#16573=CARTESIAN_POINT('',(8.3894674945056,-0.00356057987879016,11.470836477965));
#16574=CARTESIAN_POINT('Ctrl Pts',(8.39010368535713,-0.00356115582826364,
11.470836477965));
#16575=CARTESIAN_POINT('Ctrl Pts',(8.39272718587054,-0.287370610773653,
11.485202588602));
#16576=CARTESIAN_POINT('Ctrl Pts',(8.23517039613131,-1.87555148934049,11.5657407383767));
#16577=CARTESIAN_POINT('Ctrl Pts',(6.07814237389157,-4.35704729530058,11.7124509272874));
#16578=CARTESIAN_POINT('Ctrl Pts',(1.67433257548842,-3.72470155112426,11.9109670446996));
#16579=CARTESIAN_POINT('Ctrl Pts',(-0.181649509920632,0.318655022234989,
12.1094831621109));
#16580=CARTESIAN_POINT('Ctrl Pts',(2.20986920695914,4.07019338769287,12.3079992795228));
#16581=CARTESIAN_POINT('Ctrl Pts',(6.65878137671893,4.09432607198936,12.5065153969342));
#16582=CARTESIAN_POINT('Ctrl Pts',(8.34470937675079,1.5118780642868,12.6441277964151));
#16583=CARTESIAN_POINT('Ctrl Pts',(8.39548241161008,0.105584031371379,12.7155681567587));
#16584=CARTESIAN_POINT('Ctrl Pts',(8.39488259067608,0.00183385008468958,
12.720836477965));
#16585=CARTESIAN_POINT('',(8.38701749039333,0.000299844226979141,10.2208363971417));
#16586=CARTESIAN_POINT('Ctrl Pts',(8.38946909489633,0.000298426274701803,
10.220836477965));
#16587=CARTESIAN_POINT('Ctrl Pts',(8.38947828962052,-0.120880079792136,
10.2269326063233));
#16588=CARTESIAN_POINT('Ctrl Pts',(8.38388277070175,-0.241964705586662,
10.2330287346816));
#16589=CARTESIAN_POINT('Ctrl Pts',(8.37273441684076,-0.362429326648316,
10.2391248630399));
#16590=CARTESIAN_POINT('Ctrl Pts',(8.36157285084987,-0.483036712663702,
10.2452282160379));
#16591=CARTESIAN_POINT('Ctrl Pts',(8.34484535990885,-0.603022269854458,
10.2513315690359));
#16592=CARTESIAN_POINT('Ctrl Pts',(8.3226552564171,-0.721868168026954,10.2574349220339));
#16593=CARTESIAN_POINT('Ctrl Pts',(8.30041592491439,-0.840977721895287,
10.2635518151187));
#16594=CARTESIAN_POINT('Ctrl Pts',(8.27268982620504,-0.958942208026926,
10.2696687082035));
#16595=CARTESIAN_POINT('Ctrl Pts',(8.23963100122632,-1.07525581893749,10.2757856012883));
#16596=CARTESIAN_POINT('Ctrl Pts',(8.20653266957785,-1.19170842944702,10.2819098043146));
#16597=CARTESIAN_POINT('Ctrl Pts',(8.16808901353143,-1.30650588770032,10.2880340073409));
#16598=CARTESIAN_POINT('Ctrl Pts',(8.12450272777354,-1.41916114347173,10.2941582103672));
#16599=CARTESIAN_POINT('Ctrl Pts',(8.08082011201351,-1.53206537849982,10.3002959484878));
#16600=CARTESIAN_POINT('Ctrl Pts',(8.03197229300387,-1.64281761691874,10.3064336866084));
#16601=CARTESIAN_POINT('Ctrl Pts',(7.97820906556213,-1.7509530715472,10.3125714247291));
#16602=CARTESIAN_POINT('Ctrl Pts',(7.94823223058556,-1.81124630230657,10.3159936516214));
#16603=CARTESIAN_POINT('Ctrl Pts',(7.91672806648528,-1.87072649483671,10.3194158785138));
#16604=CARTESIAN_POINT('Ctrl Pts',(7.88374568220558,-1.92931704799615,10.3228381054062));
#16605=CARTESIAN_POINT('Ctrl Pts',(7.82713684628902,-2.029878092399,10.3287117947967));
#16606=CARTESIAN_POINT('Ctrl Pts',(7.76600407727453,-2.12811303680096,10.3345854841873));
#16607=CARTESIAN_POINT('Ctrl Pts',(7.70056346489689,-2.22358736999233,10.3404591735779));
#16608=CARTESIAN_POINT('Ctrl Pts',(7.6352073424978,-2.31893843684999,10.3463252794836));
#16609=CARTESIAN_POINT('Ctrl Pts',(7.56555466883785,-2.41153564287309,10.3521913853894));
#16610=CARTESIAN_POINT('Ctrl Pts',(7.49186727841229,-2.50096919937873,10.3580574912951));
#16611=CARTESIAN_POINT('Ctrl Pts',(7.41825534293565,-2.59031117706201,10.3639175903832));
#16612=CARTESIAN_POINT('Ctrl Pts',(7.34061716974116,-2.67649563197447,10.3697776894712));
#16613=CARTESIAN_POINT('Ctrl Pts',(7.25925733950609,-2.7591424608641,10.3756377885592));
#16614=CARTESIAN_POINT('Ctrl Pts',(7.17496223220766,-2.84477099879243,10.3817093066534));
#16615=CARTESIAN_POINT('Ctrl Pts',(7.08667211532095,-2.9266014597789,10.3877808247475));
#16616=CARTESIAN_POINT('Ctrl Pts',(6.99477097921102,-3.00424909113099,10.3938523428416));
#16617=CARTESIAN_POINT('Ctrl Pts',(6.90617192436707,-3.07910678103417,10.3997057064383));
#16618=CARTESIAN_POINT('Ctrl Pts',(6.81421722071067,-3.15007676361715,10.4055590700351));
#16619=CARTESIAN_POINT('Ctrl Pts',(6.71928715616625,-3.2168530387367,10.4114124336318));
#16620=CARTESIAN_POINT('Ctrl Pts',(6.62437134505164,-3.28361928762319,10.4172649183657));
#16621=CARTESIAN_POINT('Ctrl Pts',(6.52648139916281,-3.34619284343324,10.4231174030996));
#16622=CARTESIAN_POINT('Ctrl Pts',(6.42602820179401,-3.40430991083872,10.4289698878335));
#16623=CARTESIAN_POINT('Ctrl Pts',(6.32556579421566,-3.46243230679904,10.4348229091617));
#16624=CARTESIAN_POINT('Ctrl Pts',(6.22254002559596,-3.51609719519072,10.4406759304899));
#16625=CARTESIAN_POINT('Ctrl Pts',(6.11738746377471,-3.56508614335361,10.446528951818));
#16626=CARTESIAN_POINT('Ctrl Pts',(6.01219983154318,-3.61409143027689,10.4523839252419));
#16627=CARTESIAN_POINT('Ctrl Pts',(5.90488436994082,-3.65841750156439,10.4582388986657));
#16628=CARTESIAN_POINT('Ctrl Pts',(5.79589809051774,-3.69789385948521,10.4640938720895));
#16629=CARTESIAN_POINT('Ctrl Pts',(5.68678828914592,-3.7374149587871,10.4699554813737));
#16630=CARTESIAN_POINT('Ctrl Pts',(5.57600427899261,-3.77207523320505,10.4758170906578));
#16631=CARTESIAN_POINT('Ctrl Pts',(5.4640188080805,-3.80175388449559,10.481678699942));
#16632=CARTESIAN_POINT('Ctrl Pts',(5.35195782454314,-3.8314525483186,10.4875442617523));
#16633=CARTESIAN_POINT('Ctrl Pts',(5.23869416970259,-3.85616281236641,10.4934098235627));
#16634=CARTESIAN_POINT('Ctrl Pts',(5.12470965943203,-3.87581521270565,10.499275385373));
#16635=CARTESIAN_POINT('Ctrl Pts',(5.01055847585061,-3.8954963496743,10.5051495240733));
#16636=CARTESIAN_POINT('Ctrl Pts',(4.8956847414542,-3.910104810783,10.5110236627737));
#16637=CARTESIAN_POINT('Ctrl Pts',(4.78057432153144,-3.91962304429989,10.516897801474));
#16638=CARTESIAN_POINT('Ctrl Pts',(4.75146477552493,-3.92203005016997,10.5183832752553));
#16639=CARTESIAN_POINT('Ctrl Pts',(4.72234008553406,-3.92411179532524,10.5198687490365));
#16640=CARTESIAN_POINT('Ctrl Pts',(4.69320807974027,-3.92586852281323,10.5213542228178));
#16641=CARTESIAN_POINT('Ctrl Pts',(4.57801765664793,-3.93281477237915,10.5272279122084));
#16642=CARTESIAN_POINT('Ctrl Pts',(4.46232940648016,-3.9346985245286,10.5331016015989));
#16643=CARTESIAN_POINT('Ctrl Pts',(4.34662559671664,-3.93146580850201,10.5389752909895));
#16644=CARTESIAN_POINT('Ctrl Pts',(4.23107117144161,-3.92823726621551,10.5448413968952));
#16645=CARTESIAN_POINT('Ctrl Pts',(4.11550163573292,-3.91990540403819,10.550707502801));
#16646=CARTESIAN_POINT('Ctrl Pts',(4.00040328120669,-3.90646809320856,10.5565736087067));
#16647=CARTESIAN_POINT('Ctrl Pts',(3.88542278592874,-3.89304454201398,10.5624337077948));
#16648=CARTESIAN_POINT('Ctrl Pts',(3.77091292005242,-3.87452598854507,10.5682938068828));
#16649=CARTESIAN_POINT('Ctrl Pts',(3.65735820340515,-3.85096231674697,10.5741539059709));
#16650=CARTESIAN_POINT('Ctrl Pts',(3.53970669164138,-3.82654852142781,10.580225424065));
#16651=CARTESIAN_POINT('Ctrl Pts',(3.42308100104176,-3.79671871456822,10.5862969421591));
#16652=CARTESIAN_POINT('Ctrl Pts',(3.30801260714209,-3.76158698819125,10.5923684602532));
#16653=CARTESIAN_POINT('Ctrl Pts',(3.19707871259567,-3.72771757281959,10.5982218238499));
#16654=CARTESIAN_POINT('Ctrl Pts',(3.0875925598812,-3.68892081630408,10.6040751874467));
#16655=CARTESIAN_POINT('Ctrl Pts',(2.98001744102106,-3.6453503919838,10.6099285510434));
#16656=CARTESIAN_POINT('Ctrl Pts',(2.87245847420294,-3.60178650961608,10.6157810357773));
#16657=CARTESIAN_POINT('Ctrl Pts',(2.76681035352976,-3.55345053966544,10.6216335205112));
#16658=CARTESIAN_POINT('Ctrl Pts',(2.66351749202751,-3.50054474463201,10.6274860052451));
#16659=CARTESIAN_POINT('Ctrl Pts',(2.56021515995673,-3.44763409884752,10.6333390265733));
#16660=CARTESIAN_POINT('Ctrl Pts',(2.45926888407418,-3.39015298341643,10.6391920479015));
#16661=CARTESIAN_POINT('Ctrl Pts',(2.36109888263643,-3.32834983529776,10.6450450692297));
#16662=CARTESIAN_POINT('Ctrl Pts',(2.26289613960697,-3.26652607463542,10.6509000426535));
#16663=CARTESIAN_POINT('Ctrl Pts',(2.16747186165528,-3.20037763495503,10.6567550160773));
#16664=CARTESIAN_POINT('Ctrl Pts',(2.07521706967055,-3.13019611820688,10.6626099895012));
#16665=CARTESIAN_POINT('Ctrl Pts',(1.9828577187291,-3.05993505972421,10.6684715987853));
#16666=CARTESIAN_POINT('Ctrl Pts',(1.89367535257766,-2.98563205106366,10.6743332080695));
#16667=CARTESIAN_POINT('Ctrl Pts',(1.80802776012755,-2.90761886022175,10.6801948173537));
#16668=CARTESIAN_POINT('Ctrl Pts',(1.72232241487705,-2.82955306451251,10.686060379164));
#16669=CARTESIAN_POINT('Ctrl Pts',(1.64015688155057,-2.74777239570676,10.6919259409743));
#16670=CARTESIAN_POINT('Ctrl Pts',(1.56185072820382,-2.66264407040466,10.6977915027846));
#16671=CARTESIAN_POINT('Ctrl Pts',(1.48343007205496,-2.57739126661179,10.703665641485));
#16672=CARTESIAN_POINT('Ctrl Pts',(1.40888032356853,-2.48878135186914,10.7095397801853));
#16673=CARTESIAN_POINT('Ctrl Pts',(1.33847962379658,-2.39721308763069,10.7154139188856));
#16674=CARTESIAN_POINT('Ctrl Pts',(1.32067643612444,-2.37405696846808,10.7168993926669));
#16675=CARTESIAN_POINT('Ctrl Pts',(1.30313835788537,-2.35071179676952,10.7183848664482));
#16676=CARTESIAN_POINT('Ctrl Pts',(1.28586942857625,-2.32718428237569,10.7198703402294));
#16677=CARTESIAN_POINT('Ctrl Pts',(1.21758661662196,-2.23415449388392,10.72574402962));
#16678=CARTESIAN_POINT('Ctrl Pts',(1.15328798418074,-2.1379619493952,10.7316177190106));
#16679=CARTESIAN_POINT('Ctrl Pts',(1.09328032509298,-2.03898264399506,10.7374914084011));
#16680=CARTESIAN_POINT('Ctrl Pts',(1.03335014153048,-1.94013113017675,10.7433575143069));
#16681=CARTESIAN_POINT('Ctrl Pts',(0.977700126209272,-1.83850036069192,
10.7492236202126));
#16682=CARTESIAN_POINT('Ctrl Pts',(0.926595691254537,-1.73449781617977,
10.7550897261184));
#16683=CARTESIAN_POINT('Ctrl Pts',(0.875543586590257,-1.63060176894848,
10.7609498252064));
#16684=CARTESIAN_POINT('Ctrl Pts',(0.829027984993367,-1.52433914610499,
10.7668099242945));
#16685=CARTESIAN_POINT('Ctrl Pts',(0.787269631400051,-1.41614413602353,
10.7726700233825));
#16686=CARTESIAN_POINT('Ctrl Pts',(0.744004731675103,-1.30404569681056,
10.7787415414766));
#16687=CARTESIAN_POINT('Ctrl Pts',(0.705847056357807,-1.18987319180386,
10.7848130595707));
#16688=CARTESIAN_POINT('Ctrl Pts',(0.672988850968731,-1.07413507443758,
10.7908845776648));
#16689=CARTESIAN_POINT('Ctrl Pts',(0.641311267158917,-0.962555520123894,
10.7967379412616));
#16690=CARTESIAN_POINT('Ctrl Pts',(0.614559001394734,-0.849521356134258,
10.8025913048583));
#16691=CARTESIAN_POINT('Ctrl Pts',(0.592854075775143,-0.735505198169326,
10.8084446684551));
#16692=CARTESIAN_POINT('Ctrl Pts',(0.571152409077104,-0.621506159346891,
10.814297153189));
#16693=CARTESIAN_POINT('Ctrl Pts',(0.55449665289178,-0.506525825468772,
10.8201496379229));
#16694=CARTESIAN_POINT('Ctrl Pts',(0.542957764981321,-0.391047288713175,
10.8260021226568));
#16695=CARTESIAN_POINT('Ctrl Pts',(0.531417819109705,-0.2755581641256,10.831855143985));
#16696=CARTESIAN_POINT('Ctrl Pts',(0.524995715215706,-0.159571156976264,
10.8377081653132));
#16697=CARTESIAN_POINT('Ctrl Pts',(0.523710494086693,-0.0435740600020554,
10.8435611866414));
#16698=CARTESIAN_POINT('Ctrl Pts',(0.522424844311616,0.0724617242438926,
10.8494161600652));
#16699=CARTESIAN_POINT('Ctrl Pts',(0.526279488596708,0.188507192109541,
10.8552711334891));
#16700=CARTESIAN_POINT('Ctrl Pts',(0.535241367677898,0.304075685482606,
10.8611261069129));
#16701=CARTESIAN_POINT('Ctrl Pts',(0.544213403897897,0.419775160898442,
10.8669877161971));
#16702=CARTESIAN_POINT('Ctrl Pts',(0.558304196241379,0.534996170699235,
10.8728493254812));
#16703=CARTESIAN_POINT('Ctrl Pts',(0.577428918229164,0.649258207468796,
10.8787109347654));
#16704=CARTESIAN_POINT('Ctrl Pts',(0.596566536157391,0.763597291968611,
10.8845764965757));
#16705=CARTESIAN_POINT('Ctrl Pts',(0.620744756811182,0.876975712768846,
10.890442058386));
#16706=CARTESIAN_POINT('Ctrl Pts',(0.649828246082207,0.988925862713038,
10.8963076201964));
#16707=CARTESIAN_POINT('Ctrl Pts',(0.678954262547775,1.10103971123416,10.9021817588967));
#16708=CARTESIAN_POINT('Ctrl Pts',(0.712999741548429,1.21172072744612,10.908055897597));
#16709=CARTESIAN_POINT('Ctrl Pts',(0.751780383614942,1.32051901486342,10.9139300362974));
#16710=CARTESIAN_POINT('Ctrl Pts',(0.761587374894654,1.3480323256054,10.9154155100786));
#16711=CARTESIAN_POINT('Ctrl Pts',(0.771696946848984,1.37542534998821,10.9169009838599));
#16712=CARTESIAN_POINT('Ctrl Pts',(0.782105650995835,1.40269105612248,10.9183864576411));
#16713=CARTESIAN_POINT('Ctrl Pts',(0.823262550490445,1.51050197198537,10.9242601470317));
#16714=CARTESIAN_POINT('Ctrl Pts',(0.869237000275695,1.6166795106457,10.9301338364222));
#16715=CARTESIAN_POINT('Ctrl Pts',(0.919879364589478,1.72076204031997,10.9360075258128));
#16716=CARTESIAN_POINT('Ctrl Pts',(0.970456344853387,1.8247101896705,10.9418736317186));
#16717=CARTESIAN_POINT('Ctrl Pts',(1.02568907537559,1.92656834099087,10.9477397376243));
#16718=CARTESIAN_POINT('Ctrl Pts',(1.08537902941477,2.02589256725946,10.9536058435301));
#16719=CARTESIAN_POINT('Ctrl Pts',(1.14500786170141,2.12511508678566,10.9594659426181));
#16720=CARTESIAN_POINT('Ctrl Pts',(1.20908462750555,2.22180849033333,10.9653260417062));
#16721=CARTESIAN_POINT('Ctrl Pts',(1.27736414285858,2.31555190655315,10.9711861407942));
#16722=CARTESIAN_POINT('Ctrl Pts',(1.34810702735494,2.41267737136708,10.9772576588883));
#16723=CARTESIAN_POINT('Ctrl Pts',(1.42336144053963,2.50663556622707,10.9833291769824));
#16724=CARTESIAN_POINT('Ctrl Pts',(1.50280434312715,2.59698930827102,10.9894006950765));
#16725=CARTESIAN_POINT('Ctrl Pts',(1.57939279873556,2.68409656815448,10.9952540586733));
#16726=CARTESIAN_POINT('Ctrl Pts',(1.65987363602657,2.76785360237434,11.00110742227));
#16727=CARTESIAN_POINT('Ctrl Pts',(1.74391586165861,2.84790166533695,11.0069607858668));
#16728=CARTESIAN_POINT('Ctrl Pts',(1.82794546863324,2.92793770935223,11.0128132706007));
#16729=CARTESIAN_POINT('Ctrl Pts',(1.91553510162423,3.00426560455017,11.0186657553346));
#16730=CARTESIAN_POINT('Ctrl Pts',(2.00631728136105,3.07656383570192,11.0245182400685));
#16731=CARTESIAN_POINT('Ctrl Pts',(2.09710778460494,3.14886869563082,11.0303712613967));
#16732=CARTESIAN_POINT('Ctrl Pts',(2.19109109328435,3.2171428996573,11.0362242827248));
#16733=CARTESIAN_POINT('Ctrl Pts',(2.28786763352659,3.28110601057625,11.042077304053));
#16734=CARTESIAN_POINT('Ctrl Pts',(2.38467645061428,3.34509045442816,11.0479322774768));
#16735=CARTESIAN_POINT('Ctrl Pts',(2.484280007223,3.40476071842671,11.0537872509007));
#16736=CARTESIAN_POINT('Ctrl Pts',(2.58625143898061,3.45988076053962,11.0596422243245));
#16737=CARTESIAN_POINT('Ctrl Pts',(2.68833844225797,3.51506327414014,11.0655038336087));
#16738=CARTESIAN_POINT('Ctrl Pts',(2.79279831350346,3.56568507604157,11.0713654428928));
#16739=CARTESIAN_POINT('Ctrl Pts',(2.89918129332347,3.61155695895959,11.077227052177));
#16740=CARTESIAN_POINT('Ctrl Pts',(3.00563600796784,3.65745977362504,11.0830926139873));
#16741=CARTESIAN_POINT('Ctrl Pts',(3.11401602804567,3.69860614533714,11.0889581757977));
#16742=CARTESIAN_POINT('Ctrl Pts',(3.22385505368668,3.73485630212218,11.094823737608));
#16743=CARTESIAN_POINT('Ctrl Pts',(3.33385469092331,3.77115946552747,11.1006978763083));
#16744=CARTESIAN_POINT('Ctrl Pts',(3.44531719535615,3.80255201393801,11.1065720150087));
#16745=CARTESIAN_POINT('Ctrl Pts',(3.55776460494286,3.82894492248026,11.112446153709));
#16746=CARTESIAN_POINT('Ctrl Pts',(3.58620071910883,3.83561925818295,11.1139316274902));
#16747=CARTESIAN_POINT('Ctrl Pts',(3.61469978756485,3.841974124591,11.1154171012715));
#16748=CARTESIAN_POINT('Ctrl Pts',(3.64325403190415,3.84800860743688,11.1169025750527));
#16749=CARTESIAN_POINT('Ctrl Pts',(3.75615993717776,3.87186946470475,11.1227762644433));
#16750=CARTESIAN_POINT('Ctrl Pts',(3.87030494260292,3.89079662734251,11.1286499538339));
#16751=CARTESIAN_POINT('Ctrl Pts',(3.98522001639962,3.90466558047487,11.1345236432244));
#16752=CARTESIAN_POINT('Ctrl Pts',(4.09998672404016,3.91851662748579,11.1403897491302));
#16753=CARTESIAN_POINT('Ctrl Pts',(4.21552111643121,3.92732240320993,11.1462558550359));
#16754=CARTESIAN_POINT('Ctrl Pts',(4.33134253497827,3.93100907416528,11.1521219609417));
#16755=CARTESIAN_POINT('Ctrl Pts',(4.4470453538682,3.93469197001653,11.1579820600297));
#16756=CARTESIAN_POINT('Ctrl Pts',(4.56303420381904,3.93326617460282,11.1638421591177));
#16757=CARTESIAN_POINT('Ctrl Pts',(4.67882250677198,3.92670955957558,11.1697022582058));
#16758=CARTESIAN_POINT('Ctrl Pts',(4.79878818754027,3.91991639683617,11.1757737762999));
#16759=CARTESIAN_POINT('Ctrl Pts',(4.91853812912318,3.9076151539711,11.181845294394));
#16760=CARTESIAN_POINT('Ctrl Pts',(5.03752984066193,3.88984028243934,11.1879168124881));
#16761=CARTESIAN_POINT('Ctrl Pts',(5.15224608490948,3.87270407624702,11.1937701760849));
#16762=CARTESIAN_POINT('Ctrl Pts',(5.26625720537262,3.85048088198621,11.1996235396816));
#16763=CARTESIAN_POINT('Ctrl Pts',(5.37908231067531,3.82325435656085,11.2054769032784));
#16764=CARTESIAN_POINT('Ctrl Pts',(5.49189047566793,3.7960319191067,11.2113293880123));
#16765=CARTESIAN_POINT('Ctrl Pts',(5.60351257807364,3.76380774111264,11.2171818727462));
#16766=CARTESIAN_POINT('Ctrl Pts',(5.71347923211499,3.72671632182986,11.2230343574801));
#16767=CARTESIAN_POINT('Ctrl Pts',(5.82345596862205,3.68962150176194,11.2288873788083));
#16768=CARTESIAN_POINT('Ctrl Pts',(5.93177656353831,3.64765868533166,11.2347404001365));
#16769=CARTESIAN_POINT('Ctrl Pts',(6.03798875048295,3.60101160992364,11.2405934214646));
#16770=CARTESIAN_POINT('Ctrl Pts',(6.14423636124303,3.55434897681516,11.2464483948885));
#16771=CARTESIAN_POINT('Ctrl Pts',(6.24837378769322,3.50299914422559,11.2523033683123));
#16772=CARTESIAN_POINT('Ctrl Pts',(6.34997127462551,3.44719284900584,11.2581583417361));
#16773=CARTESIAN_POINT('Ctrl Pts',(6.45168390925957,3.39132330451849,11.2640199510203));
#16774=CARTESIAN_POINT('Ctrl Pts',(6.55085049635795,3.33098741526809,11.2698815603044));
#16775=CARTESIAN_POINT('Ctrl Pts',(6.64706822470992,3.26646054653405,11.2757431695886));
#16776=CARTESIAN_POINT('Ctrl Pts',(6.74335083338242,3.20189016685876,11.2816087313989));
#16777=CARTESIAN_POINT('Ctrl Pts',(6.83668029210354,3.13312342495588,11.2874742932092));
#16778=CARTESIAN_POINT('Ctrl Pts',(6.92668636379225,3.06047638454924,11.2933398550196));
#16779=CARTESIAN_POINT('Ctrl Pts',(7.01682404643358,2.98772311635138,11.2992139937199));
#16780=CARTESIAN_POINT('Ctrl Pts',(7.10362833498062,2.91107849827556,11.3050881324202));
#16781=CARTESIAN_POINT('Ctrl Pts',(7.1867653133645,2.83089590434597,11.3109622711206));
#16782=CARTESIAN_POINT('Ctrl Pts',(7.20778929797644,2.81061903533184,11.3124477449019));
#16783=CARTESIAN_POINT('Ctrl Pts',(7.22857895815252,2.79011607799067,11.3139332186831));
#16784=CARTESIAN_POINT('Ctrl Pts',(7.24912930887828,2.76939307294556,11.3154186924644));
#16785=CARTESIAN_POINT('Ctrl Pts',(7.32927828383865,2.68857072423587,11.3212122286667));
#16786=CARTESIAN_POINT('Ctrl Pts',(7.40606706242935,2.6041132158985,11.3270057648691));
#16787=CARTESIAN_POINT('Ctrl Pts',(7.47914097595604,2.51633538462103,11.3327993010714));
#16788=CARTESIAN_POINT('Ctrl Pts',(7.55209911577413,2.42869662301384,11.3385836583597));
#16789=CARTESIAN_POINT('Ctrl Pts',(7.62135383077772,2.33774832840261,11.3443680156479));
#16790=CARTESIAN_POINT('Ctrl Pts',(7.68658655478061,2.24384274593675,11.3501523729362));
#16791=CARTESIAN_POINT('Ctrl Pts',(7.7517602556785,2.15002213001398,11.3559314964904));
#16792=CARTESIAN_POINT('Ctrl Pts',(7.81291895401834,2.05324988897331,11.3617106200447));
#16793=CARTESIAN_POINT('Ctrl Pts',(7.86978389785402,1.95391175164092,11.3674897435989));
#16794=CARTESIAN_POINT('Ctrl Pts',(7.9266120402158,1.85463790329963,11.3732651270586));
#16795=CARTESIAN_POINT('Ctrl Pts',(7.97915173944889,1.75280182648967,11.3790405105184));
#16796=CARTESIAN_POINT('Ctrl Pts',(8.02716768780263,1.6488179521922,11.3848158939781));
#16797=CARTESIAN_POINT('Ctrl Pts',(8.07516492791672,1.54487459266761,11.3905890272009));
#16798=CARTESIAN_POINT('Ctrl Pts',(8.11864174333495,1.43878548517782,11.3963621604238));
#16799=CARTESIAN_POINT('Ctrl Pts',(8.15740931008386,1.33098858275012,11.4021352936466));
#16800=CARTESIAN_POINT('Ctrl Pts',(8.19618594375124,1.22316646889425,11.4079097770839));
#16801=CARTESIAN_POINT('Ctrl Pts',(8.23025097372873,1.11363615900231,11.4136842605211));
#16802=CARTESIAN_POINT('Ctrl Pts',(8.25946432045127,1.00285412723924,11.4194587439584));
#16803=CARTESIAN_POINT('Ctrl Pts',(8.28867979540815,0.892064024845738,11.4252336480751));
#16804=CARTESIAN_POINT('Ctrl Pts',(8.31304278359162,0.780022433108546,11.4310085521918));
#16805=CARTESIAN_POINT('Ctrl Pts',(8.33246391806155,0.667198035491587,11.4367834563085));
#16806=CARTESIAN_POINT('Ctrl Pts',(8.35190402178076,0.55426343864161,11.4425640009606));
#16807=CARTESIAN_POINT('Ctrl Pts',(8.36639256469885,0.440544929944047,11.4483445456126));
#16808=CARTESIAN_POINT('Ctrl Pts',(8.37589186159069,0.326518398668027,11.4541250902647));
#16809=CARTESIAN_POINT('Ctrl Pts',(8.38504592594477,0.216635928706429,11.4596955528315));
#16810=CARTESIAN_POINT('Ctrl Pts',(8.38956710420808,0.106467789835327,11.4652660153982));
#16811=CARTESIAN_POINT('Ctrl Pts',(8.3894674945056,-0.00356057987879016,
11.470836477965));
#16812=CARTESIAN_POINT('',(8.38956893211207,0.00341085378143758,8.97083652763293));
#16813=CARTESIAN_POINT('Ctrl Pts',(8.39119799873609,0.00339649975582836,
8.97083732632742));
#16814=CARTESIAN_POINT('Ctrl Pts',(8.38152382860528,-1.0554250693434,9.02447201786367));
#16815=CARTESIAN_POINT('Ctrl Pts',(7.39472429574437,-3.43645618331368,9.14427874853716));
#16816=CARTESIAN_POINT('Ctrl Pts',(3.37012330303654,-4.52034712344961,9.33025751834786));
#16817=CARTESIAN_POINT('Ctrl Pts',(0.0690675541444807,-1.53765826549021,
9.52877363575949));
#16818=CARTESIAN_POINT('Ctrl Pts',(0.785910689414721,2.85318878264351,9.72728975317118));
#16819=CARTESIAN_POINT('Ctrl Pts',(4.86418140136913,4.63113981703775,9.9258058705828));
#16820=CARTESIAN_POINT('Ctrl Pts',(7.93452534716083,2.58985569568638,10.0903213748425));
#16821=CARTESIAN_POINT('Ctrl Pts',(8.38346869164466,0.638758348126131,10.1886648399649));
#16822=CARTESIAN_POINT('Ctrl Pts',(8.38303806571692,0.000302145835691118,
10.22083626595));
#16823=CARTESIAN_POINT('',(8.38946839700585,-0.00236191959998835,7.72083647791993));
#16824=CARTESIAN_POINT('Ctrl Pts',(8.38946839700532,-0.00236192048784542,
7.72083647796504));
#16825=CARTESIAN_POINT('Ctrl Pts',(8.38938451678962,-0.142036744660387,
7.7279338449949));
#16826=CARTESIAN_POINT('Ctrl Pts',(8.38186061236754,-0.281485965734069,
7.73503121202475));
#16827=CARTESIAN_POINT('Ctrl Pts',(8.36696529334037,-0.420129230717581,
7.7421285790546));
#16828=CARTESIAN_POINT('Ctrl Pts',(8.35463811947842,-0.53486860817727,7.74800226844517));
#16829=CARTESIAN_POINT('Ctrl Pts',(8.33723621668261,-0.64925607920517,7.75387595783574));
#16830=CARTESIAN_POINT('Ctrl Pts',(8.31478665350495,-0.762807121295797,
7.75974964722631));
#16831=CARTESIAN_POINT('Ctrl Pts',(8.29236607482239,-0.87621155832346,7.76561575313208));
#16832=CARTESIAN_POINT('Ctrl Pts',(8.26491087533944,-0.988781312399312,
7.77148185903784));
#16833=CARTESIAN_POINT('Ctrl Pts',(8.23249991209748,-1.10003652350777,7.7773479649436));
#16834=CARTESIAN_POINT('Ctrl Pts',(8.20012213726901,-1.21117781069729,7.78320806403164));
#16835=CARTESIAN_POINT('Ctrl Pts',(8.16279880742635,-1.3210068380762,7.78906816311968));
#16836=CARTESIAN_POINT('Ctrl Pts',(8.12065977154157,-1.42905415158329,7.79492826220772));
#16837=CARTESIAN_POINT('Ctrl Pts',(8.07700045537665,-1.54099956566621,7.80099978030183));
#16838=CARTESIAN_POINT('Ctrl Pts',(8.02817148082484,-1.65103183515718,7.80707129839594));
#16839=CARTESIAN_POINT('Ctrl Pts',(7.97437382595932,-1.75864589466542,7.81314281649004));
#16840=CARTESIAN_POINT('Ctrl Pts',(7.92250916382703,-1.86239329501268,7.8189961800868));
#16841=CARTESIAN_POINT('Ctrl Pts',(7.86602693437099,-1.96389286992841,7.82484954368356));
#16842=CARTESIAN_POINT('Ctrl Pts',(7.80515579369172,-2.06271337542034,7.83070290728031));
#16843=CARTESIAN_POINT('Ctrl Pts',(7.74429379260934,-2.16151904334598,7.83655539201423));
#16844=CARTESIAN_POINT('Ctrl Pts',(7.67904440722507,-2.25764609000753,7.84240787674815));
#16845=CARTESIAN_POINT('Ctrl Pts',(7.60968106185165,-2.35068997591145,7.84826036148206));
#16846=CARTESIAN_POINT('Ctrl Pts',(7.54031135679081,-2.44374239269039,7.85411338281024));
#16847=CARTESIAN_POINT('Ctrl Pts',(7.46682718885623,-2.53371075551174,7.85996640413843));
#16848=CARTESIAN_POINT('Ctrl Pts',(7.38954348461585,-2.62022206898338,7.86581942546661));
#16849=CARTESIAN_POINT('Ctrl Pts',(7.31223400476758,-2.70676223564879,7.87167439889044));
#16850=CARTESIAN_POINT('Ctrl Pts',(7.23112274390024,-2.78984275234918,7.87752937231428));
#16851=CARTESIAN_POINT('Ctrl Pts',(7.14656233055052,-2.86912659957723,7.88338434573811));
#16852=CARTESIAN_POINT('Ctrl Pts',(7.06190607883368,-2.94850030486245,7.88924595502227));
#16853=CARTESIAN_POINT('Ctrl Pts',(6.97379317372207,-3.02406846933132,7.89510756430643));
#16854=CARTESIAN_POINT('Ctrl Pts',(6.88261031695746,-3.09553352841685,7.9009691735906));
#16855=CARTESIAN_POINT('Ctrl Pts',(6.79136597492294,-3.16704677691652,7.90683473540094));
#16856=CARTESIAN_POINT('Ctrl Pts',(6.69704789452532,-3.23445117118951,7.91270029721129));
#16857=CARTESIAN_POINT('Ctrl Pts',(6.60007136856806,-3.2974927355263,7.91856585902163));
#16858=CARTESIAN_POINT('Ctrl Pts',(6.5029530391447,-3.36062648209218,7.92443999772197));
#16859=CARTESIAN_POINT('Ctrl Pts',(6.40316886072867,-3.41938445795923,7.93031413642231));
#16860=CARTESIAN_POINT('Ctrl Pts',(6.3011583341624,-3.4735587878006,7.93618827512266));
#16861=CARTESIAN_POINT('Ctrl Pts',(6.27536153732952,-3.48725859141418,7.93767374890386));
#16862=CARTESIAN_POINT('Ctrl Pts',(6.2494224605816,-3.50066551228908,7.93915922268506));
#16863=CARTESIAN_POINT('Ctrl Pts',(6.22334839260746,-3.51377668432824,7.94064469646626));
#16864=CARTESIAN_POINT('Ctrl Pts',(6.12024931515043,-3.56561937120619,7.94651838585683));
#16865=CARTESIAN_POINT('Ctrl Pts',(6.01469488860868,-3.61300695171493,7.9523920752474));
#16866=CARTESIAN_POINT('Ctrl Pts',(5.9071069351652,-3.65569950751263,7.95826576463797));
#16867=CARTESIAN_POINT('Ctrl Pts',(5.79965788787712,-3.69833694320997,7.96413187054372));
#16868=CARTESIAN_POINT('Ctrl Pts',(5.69018091540317,-3.73629125797423,7.96999797644947));
#16869=CARTESIAN_POINT('Ctrl Pts',(5.57912199703213,-3.76936857931766,7.97586408235522));
#16870=CARTESIAN_POINT('Ctrl Pts',(5.46817680157858,-3.80241202990545,7.98172418144326));
#16871=CARTESIAN_POINT('Ctrl Pts',(5.35565327593104,-3.83058830328179,7.9875842805313));
#16872=CARTESIAN_POINT('Ctrl Pts',(5.24201629838382,-3.85375201704531,7.99344437961934));
#16873=CARTESIAN_POINT('Ctrl Pts',(5.12427955793418,-3.87775142475651,7.99951589771344));
#16874=CARTESIAN_POINT('Ctrl Pts',(5.00534792691778,-3.89636959407862,8.00558741580755));
#16875=CARTESIAN_POINT('Ctrl Pts',(4.88575476787085,-3.90950160771159,8.01165893390166));
#16876=CARTESIAN_POINT('Ctrl Pts',(4.77045868660498,-3.92216177759987,8.01751229749841));
#16877=CARTESIAN_POINT('Ctrl Pts',(4.65454824352446,-3.9297232018855,8.02336566109515));
#16878=CARTESIAN_POINT('Ctrl Pts',(4.53850977298686,-3.93214424061429,8.0292190246919));
#16879=CARTESIAN_POINT('Ctrl Pts',(4.42248872523512,-3.93456491583226,8.0350715094258));
#16880=CARTESIAN_POINT('Ctrl Pts',(4.30634010119277,-3.93184673152903,8.0409239941597));
#16881=CARTESIAN_POINT('Ctrl Pts',(4.19055206449122,-3.92400014359316,8.0467764788936));
#16882=CARTESIAN_POINT('Ctrl Pts',(4.07475341158138,-3.91615283623053,8.05262950022177));
#16883=CARTESIAN_POINT('Ctrl Pts',(3.95931582395675,-3.90317621844521,8.05848252154994));
#16884=CARTESIAN_POINT('Ctrl Pts',(3.84472345726007,-3.8851327211539,8.06433554287811));
#16885=CARTESIAN_POINT('Ctrl Pts',(3.73009287179602,-3.86708320600778,8.07019051630193));
#16886=CARTESIAN_POINT('Ctrl Pts',(3.61630847569694,-3.8439635152872,8.07604548972575));
#16887=CARTESIAN_POINT('Ctrl Pts',(3.50384463238308,-3.81588726403837,8.08190046314957));
#16888=CARTESIAN_POINT('Ctrl Pts',(3.39125332574829,-3.78777919196502,8.08776207243372));
#16889=CARTESIAN_POINT('Ctrl Pts',(3.27998596024276,-3.75470344704791,8.09362368171788));
#16890=CARTESIAN_POINT('Ctrl Pts',(3.17050221639931,-3.71682366521327,8.09948529100203));
#16891=CARTESIAN_POINT('Ctrl Pts',(3.0609446468634,-3.67891834076357,8.10535085281237));
#16892=CARTESIAN_POINT('Ctrl Pts',(2.95317347697617,-3.63620268089148,8.1112164146227));
#16893=CARTESIAN_POINT('Ctrl Pts',(2.84762725869796,-3.58888797675095,8.11708197643304));
#16894=CARTESIAN_POINT('Ctrl Pts',(2.7419267059617,-3.54150408690825,8.12295611513337));
#16895=CARTESIAN_POINT('Ctrl Pts',(2.63845796558737,-3.48950791632374,8.1288302538337));
#16896=CARTESIAN_POINT('Ctrl Pts',(2.53763397443016,-3.43315608981237,8.13470439253403));
#16897=CARTESIAN_POINT('Ctrl Pts',(2.51213723303021,-3.41890563283795,8.13618986631532));
#16898=CARTESIAN_POINT('Ctrl Pts',(2.48680947199874,-3.40437684241615,8.13767534009662));
#16899=CARTESIAN_POINT('Ctrl Pts',(2.46165705100713,-3.38957428955088,8.13916081387791));
#16900=CARTESIAN_POINT('Ctrl Pts',(2.36220224393779,-3.33104373935695,8.14503450326848));
#16901=CARTESIAN_POINT('Ctrl Pts',(2.26516002961895,-3.26803478452421,8.15090819265904));
#16902=CARTESIAN_POINT('Ctrl Pts',(2.1709606871333,-3.20077182352816,8.15678188204961));
#16903=CARTESIAN_POINT('Ctrl Pts',(2.0768829648484,-3.13359570533381,8.16264798795536));
#16904=CARTESIAN_POINT('Ctrl Pts',(1.98564114830211,-3.06217674129319,8.16851409386112));
#16905=CARTESIAN_POINT('Ctrl Pts',(1.89763991968141,-2.98678459118283,8.17438019976687));
#16906=CARTESIAN_POINT('Ctrl Pts',(1.80972880319777,-2.91146964167377,8.1802402988549));
#16907=CARTESIAN_POINT('Ctrl Pts',(1.72505198610896,-2.83218986585914,8.18610039794294));
#16908=CARTESIAN_POINT('Ctrl Pts',(1.64398364933252,-2.74925709143511,8.19196049703097));
#16909=CARTESIAN_POINT('Ctrl Pts',(1.55999055191163,-2.66333229170977,8.19803201512508));
#16910=CARTESIAN_POINT('Ctrl Pts',(1.47987158979592,-2.57348619555289,8.20410353321919));
#16911=CARTESIAN_POINT('Ctrl Pts',(1.40400406671963,-2.48011011502285,8.2101750513133));
#16912=CARTESIAN_POINT('Ctrl Pts',(1.33086252437931,-2.3900891116906,8.21602841491005));
#16913=CARTESIAN_POINT('Ctrl Pts',(1.26167244659689,-2.29678777681905,8.22188177850679));
#16914=CARTESIAN_POINT('Ctrl Pts',(1.19673247023338,-2.20059220757005,8.22773514210354));
#16915=CARTESIAN_POINT('Ctrl Pts',(1.13180224438879,-2.10441108176206,8.23358762683744));
#16916=CARTESIAN_POINT('Ctrl Pts',(1.07112108220504,-2.00533692797377,8.23944011157134));
#16917=CARTESIAN_POINT('Ctrl Pts',(1.01494483566442,-1.90378562217202,8.24529259630524));
#16918=CARTESIAN_POINT('Ctrl Pts',(0.958763438516236,-1.802225005479,8.25114561763342));
#16919=CARTESIAN_POINT('Ctrl Pts',(0.907087978092209,-1.69818714681344,
8.25699863896159));
#16920=CARTESIAN_POINT('Ctrl Pts',(0.86012845858185,-1.59211273035492,8.26285166028976));
#16921=CARTESIAN_POINT('Ctrl Pts',(0.813153277164838,-1.48600293602997,
8.26870663371358));
#16922=CARTESIAN_POINT('Ctrl Pts',(0.770897331372616,-1.37785561086723,
8.27456160713741));
#16923=CARTESIAN_POINT('Ctrl Pts',(0.733522306512086,-1.26813095796831,
8.28041658056123));
#16924=CARTESIAN_POINT('Ctrl Pts',(0.69610492186153,-1.15828194626896,8.28627818984538));
#16925=CARTESIAN_POINT('Ctrl Pts',(0.663579632762124,-1.0468524299936,8.29213979912953));
#16926=CARTESIAN_POINT('Ctrl Pts',(0.636058131849826,-0.934317390893103,
8.29800140841368));
#16927=CARTESIAN_POINT('Ctrl Pts',(0.608518072987343,-0.821706468589274,
8.30386697022402));
#16928=CARTESIAN_POINT('Ctrl Pts',(0.585988600968007,-0.707988943344857,
8.30973253203436));
#16929=CARTESIAN_POINT('Ctrl Pts',(0.568529909365876,-0.593647876757686,
8.3155980938447));
#16930=CARTESIAN_POINT('Ctrl Pts',(0.551045688874598,-0.479139615487187,
8.32147223254503));
#16931=CARTESIAN_POINT('Ctrl Pts',(0.538647090792383,-0.364006402400335,
8.32734637124536));
#16932=CARTESIAN_POINT('Ctrl Pts',(0.531342328270057,-0.248734350329883,
8.33322050994569));
#16933=CARTESIAN_POINT('Ctrl Pts',(0.529495073079284,-0.219583930191329,
8.33470598372699));
#16934=CARTESIAN_POINT('Ctrl Pts',(0.527973309533415,-0.190424618373375,
8.33619145750828));
#16935=CARTESIAN_POINT('Ctrl Pts',(0.52677664422032,-0.161264236942484,
8.33767693128958));
#16936=CARTESIAN_POINT('Ctrl Pts',(0.522044928021695,-0.0459616141750869,
8.34355062068014));
#16937=CARTESIAN_POINT('Ctrl Pts',(0.522384339860266,0.0697414737208014,
8.34942431007071));
#16938=CARTESIAN_POINT('Ctrl Pts',(0.527839574319278,0.185361811307665,
8.35529799946128));
#16939=CARTESIAN_POINT('Ctrl Pts',(0.533287765558104,0.300832872176622,
8.36116410536703));
#16940=CARTESIAN_POINT('Ctrl Pts',(0.54383862492926,0.416220986286492,8.36703021127279));
#16941=CARTESIAN_POINT('Ctrl Pts',(0.559484937268936,0.531039910890344,
8.37289631717854));
#16942=CARTESIAN_POINT('Ctrl Pts',(0.575115227984102,0.645741262378132,
8.37875641626658));
#16943=CARTESIAN_POINT('Ctrl Pts',(0.595830537820032,0.759874176753978,
8.38461651535462));
#16944=CARTESIAN_POINT('Ctrl Pts',(0.621571682550897,0.872955182096708,
8.39047661444265));
#16945=CARTESIAN_POINT('Ctrl Pts',(0.648241509058696,0.990115892133119,
8.39654813253676));
#16946=CARTESIAN_POINT('Ctrl Pts',(0.680306637325,1.10614690796246,8.40261965063087));
#16947=CARTESIAN_POINT('Ctrl Pts',(0.717642784699322,1.22051904430748,8.40869116872498));
#16948=CARTESIAN_POINT('Ctrl Pts',(0.753637414460184,1.3307816983897,8.41454453232173));
#16949=CARTESIAN_POINT('Ctrl Pts',(0.7945306590742,1.43950220472268,8.42039789591848));
#16950=CARTESIAN_POINT('Ctrl Pts',(0.840159971949192,1.54622030946504,8.42625125951523));
#16951=CARTESIAN_POINT('Ctrl Pts',(0.88578243373641,1.65292239084311,8.43210374424913));
#16952=CARTESIAN_POINT('Ctrl Pts',(0.936139387461083,1.75762228866743,8.43795622898303));
#16953=CARTESIAN_POINT('Ctrl Pts',(0.991020069077824,1.85987955819255,8.44380871371694));
#16954=CARTESIAN_POINT('Ctrl Pts',(1.0459057825162,1.9621462033363,8.44966173504511));
#16955=CARTESIAN_POINT('Ctrl Pts',(1.10531585297771,2.06196941092612,8.45551475637329));
#16956=CARTESIAN_POINT('Ctrl Pts',(1.16899381535657,2.1589338137085,8.46136777770146));
#16957=CARTESIAN_POINT('Ctrl Pts',(1.23269301556566,2.25593055599182,8.46722275112528));
#16958=CARTESIAN_POINT('Ctrl Pts',(1.30066271144355,2.35006625239295,8.47307772454911));
#16959=CARTESIAN_POINT('Ctrl Pts',(1.37260384185533,2.44095555700136,8.47893269797293));
#16960=CARTESIAN_POINT('Ctrl Pts',(1.44462650829791,2.53194787296222,8.48479430725709));
#16961=CARTESIAN_POINT('Ctrl Pts',(1.52062933666531,2.61968612920501,8.49065591654124));
#16962=CARTESIAN_POINT('Ctrl Pts',(1.60027374570524,2.70381897740657,8.4965175258254));
#16963=CARTESIAN_POINT('Ctrl Pts',(1.67997185955514,2.78800855700561,8.50238308763574));
#16964=CARTESIAN_POINT('Ctrl Pts',(1.76331614732318,2.86858760114024,8.50824864944608));
#16965=CARTESIAN_POINT('Ctrl Pts',(1.84993332006699,2.94524365639124,8.51411421125643));
#16966=CARTESIAN_POINT('Ctrl Pts',(1.93667714836154,3.02201180159609,8.51998834995676));
#16967=CARTESIAN_POINT('Ctrl Pts',(2.02670309284885,3.09484525070625,8.5258624886571));
#16968=CARTESIAN_POINT('Ctrl Pts',(2.11960712152811,3.16347357575657,8.53173662735743));
#16969=CARTESIAN_POINT('Ctrl Pts',(2.14310103371124,3.18082855879583,8.53322210113869));
#16970=CARTESIAN_POINT('Ctrl Pts',(2.16677886975879,3.19791484891566,8.53470757491996));
#16971=CARTESIAN_POINT('Ctrl Pts',(2.19063384345448,3.21472853628673,8.53619304870123));
#16972=CARTESIAN_POINT('Ctrl Pts',(2.28495843381453,3.28121128298559,8.54206673809179));
#16973=CARTESIAN_POINT('Ctrl Pts',(2.38236864490508,3.3436498169556,8.54794042748236));
#16974=CARTESIAN_POINT('Ctrl Pts',(2.48248265636078,3.40174462530319,8.55381411687292));
#16975=CARTESIAN_POINT('Ctrl Pts',(2.58246741122243,3.45976442779545,8.55968022277868));
#16976=CARTESIAN_POINT('Ctrl Pts',(2.68514867019757,3.51345145198743,8.56554632868444));
#16977=CARTESIAN_POINT('Ctrl Pts',(2.7901139282814,3.56254816402011,8.57141243459019));
#16978=CARTESIAN_POINT('Ctrl Pts',(2.89497170327807,3.6115946016451,8.57727253367823));
#16979=CARTESIAN_POINT('Ctrl Pts',(3.00210845333796,3.65605990263494,8.58313263276627));
#16980=CARTESIAN_POINT('Ctrl Pts',(3.11108582888008,3.69573170523224,8.5889927318543));
#16981=CARTESIAN_POINT('Ctrl Pts',(3.2239948595146,3.7368347759614,8.59506424994841));
#16982=CARTESIAN_POINT('Ctrl Pts',(3.33887944364003,3.77279171431066,8.60113576804251));
#16983=CARTESIAN_POINT('Ctrl Pts',(3.45522752790838,3.80342007959462,8.60720728613662));
#16984=CARTESIAN_POINT('Ctrl Pts',(3.56739513252589,3.83294794323635,8.61306064973337));
#16985=CARTESIAN_POINT('Ctrl Pts',(3.68092244399082,3.85752344941429,8.61891401333012));
#16986=CARTESIAN_POINT('Ctrl Pts',(3.79533458933496,3.87703367932051,8.62476737692687));
#16987=CARTESIAN_POINT('Ctrl Pts',(3.90972955608043,3.89654097983135,8.63061986166077));
#16988=CARTESIAN_POINT('Ctrl Pts',(4.02500868538324,3.91098444686735,8.63647234639467));
#16989=CARTESIAN_POINT('Ctrl Pts',(4.14068761087392,3.92030241782418,8.64232483112857));
#16990=CARTESIAN_POINT('Ctrl Pts',(4.25637714256894,3.92962124311384,8.64817785245674));
#16991=CARTESIAN_POINT('Ctrl Pts',(4.37246613148667,3.93381360495587,8.65403087378492));
#16992=CARTESIAN_POINT('Ctrl Pts',(4.48846650909144,3.9328698384525,8.65988389511309));
#16993=CARTESIAN_POINT('Ctrl Pts',(4.60450557506257,3.93192575718477,8.66573886853692));
#16994=CARTESIAN_POINT('Ctrl Pts',(4.72045555804647,3.92584214471091,8.67159384196076));
#16995=CARTESIAN_POINT('Ctrl Pts',(4.83583052496501,3.91466140476625,8.67744881538459));
#16996=CARTESIAN_POINT('Ctrl Pts',(4.95133625458897,3.903467992889,8.68331042466874));
#16997=CARTESIAN_POINT('Ctrl Pts',(5.06626525593137,3.88716596299063,8.68917203395289));
#16998=CARTESIAN_POINT('Ctrl Pts',(5.18013874012203,3.86584935828669,8.69503364323705));
#16999=CARTESIAN_POINT('Ctrl Pts',(5.29408901003933,3.84451837963965,8.70089920504739));
#17000=CARTESIAN_POINT('Ctrl Pts',(5.40698194423309,3.81816618682185,8.70676476685773));
#17001=CARTESIAN_POINT('Ctrl Pts',(5.51835262215726,3.78693707349053,8.71263032866807));
#17002=CARTESIAN_POINT('Ctrl Pts',(5.62988615132805,3.75566229553606,8.7185044673684));
#17003=CARTESIAN_POINT('Ctrl Pts',(5.73989259089843,3.71949649341352,8.72437860606873));
#17004=CARTESIAN_POINT('Ctrl Pts',(5.84792566853679,3.67863257681175,8.73025274476906));
#17005=CARTESIAN_POINT('Ctrl Pts',(5.87524547021817,3.66829875941166,8.73173821855034));
#17006=CARTESIAN_POINT('Ctrl Pts',(5.90243919400706,3.65766472835785,8.73322369233161));
#17007=CARTESIAN_POINT('Ctrl Pts',(5.92949987557082,3.64673406660543,8.73470916611288));
#17008=CARTESIAN_POINT('Ctrl Pts',(6.0365001068818,3.6035133024449,8.74058285550345));
#17009=CARTESIAN_POINT('Ctrl Pts',(6.14177469884634,3.55550726078617,8.74645654489402));
#17010=CARTESIAN_POINT('Ctrl Pts',(6.24486497997806,3.50287441949021,8.75233023428459));
#17011=CARTESIAN_POINT('Ctrl Pts',(6.34782216187183,3.45030953213706,8.75819634019034));
#17012=CARTESIAN_POINT('Ctrl Pts',(6.44860027668607,3.39312991089164,8.76406244609609));
#17013=CARTESIAN_POINT('Ctrl Pts',(6.5467592938117,3.33154257539215,8.76992855200183));
#17014=CARTESIAN_POINT('Ctrl Pts',(6.64481779735428,3.27001830453962,8.77578865108987));
#17015=CARTESIAN_POINT('Ctrl Pts',(6.74026218989035,3.20409551531674,8.7816487501779));
#17016=CARTESIAN_POINT('Ctrl Pts',(6.83267638869174,3.13402743298778,8.78750884926594));
#17017=CARTESIAN_POINT('Ctrl Pts',(6.92842468095541,3.06143145409922,8.79358036736005));
#17018=CARTESIAN_POINT('Ctrl Pts',(7.02091960413443,2.98438563480163,8.79965188545415));
#17019=CARTESIAN_POINT('Ctrl Pts',(7.10973026289912,2.90322135471075,8.80572340354826));
#17020=CARTESIAN_POINT('Ctrl Pts',(7.19534988371865,2.82497337206843,8.81157676714501));
#17021=CARTESIAN_POINT('Ctrl Pts',(7.27754510971338,2.74289809700929,8.81743013074176));
#17022=CARTESIAN_POINT('Ctrl Pts',(7.35596362117029,2.65733335465519,8.82328349433851));
#17023=CARTESIAN_POINT('Ctrl Pts',(7.43437035835158,2.57178145955925,8.82913597907241));
#17024=CARTESIAN_POINT('Ctrl Pts',(7.50900122945863,2.4827414434393,8.83498846380631));
#17025=CARTESIAN_POINT('Ctrl Pts',(7.57954183930544,2.39058689527223,8.84084094854022));
#17026=CARTESIAN_POINT('Ctrl Pts',(7.65008891677911,2.29842389777034,8.84669396986839));
#17027=CARTESIAN_POINT('Ctrl Pts',(7.716544736349,2.20314612863679,8.85254699119657));
#17028=CARTESIAN_POINT('Ctrl Pts',(7.77863658993046,2.10515847625905,8.85840001252475));
#17029=CARTESIAN_POINT('Ctrl Pts',(7.84074915234425,2.00713814310682,8.86425498594858));
#17030=CARTESIAN_POINT('Ctrl Pts',(7.89849463361993,1.90640647833885,8.8701099593724));
#17031=CARTESIAN_POINT('Ctrl Pts',(7.95164523700569,1.80339480280214,8.87596493279623));
#17032=CARTESIAN_POINT('Ctrl Pts',(8.00485607977335,1.70026637676274,8.88182654208039));
#17033=CARTESIAN_POINT('Ctrl Pts',(8.0534614608428,1.59485314960669,8.88768815136454));
#17034=CARTESIAN_POINT('Ctrl Pts',(8.09728084946573,1.48760843310034,8.89354976064869));
#17035=CARTESIAN_POINT('Ctrl Pts',(8.14112978582425,1.38029140069397,8.89941532245903));
#17036=CARTESIAN_POINT('Ctrl Pts',(8.18018616476053,1.27114080783443,8.90528088426938));
#17037=CARTESIAN_POINT('Ctrl Pts',(8.21431919951715,1.16062555386887,8.91114644607972));
#17038=CARTESIAN_POINT('Ctrl Pts',(8.24850214514226,1.04994869949638,8.91702058478005));
#17039=CARTESIAN_POINT('Ctrl Pts',(8.27774727498152,0.937903599778417,8.92289472348039));
#17040=CARTESIAN_POINT('Ctrl Pts',(8.30197476408481,0.824969839034305,8.92876886218072));
#17041=CARTESIAN_POINT('Ctrl Pts',(8.30810150056227,0.796410734599732,8.930254335962));
#17042=CARTESIAN_POINT('Ctrl Pts',(8.31390761712603,0.767794825730547,8.93173980974327));
#17043=CARTESIAN_POINT('Ctrl Pts',(8.31939234913042,0.73912990696419,8.93322528352454));
#17044=CARTESIAN_POINT('Ctrl Pts',(8.35134129734664,0.572154746727596,8.94187827238096));
#17045=CARTESIAN_POINT('Ctrl Pts',(8.37247152198213,0.403048461862582,8.95053126123738));
#17046=CARTESIAN_POINT('Ctrl Pts',(8.38256404026409,0.232954005888667,8.9591842500938));
#17047=CARTESIAN_POINT('Ctrl Pts',(8.38709427926657,0.156603533486162,8.96306832605088));
#17048=CARTESIAN_POINT('Ctrl Pts',(8.3894011415604,0.0800542813425082,8.96695240200797));
#17049=CARTESIAN_POINT('Ctrl Pts',(8.38946762642983,0.00341174640567755,
8.97083647796505));
#17050=CARTESIAN_POINT('',(8.38749085931107,-0.00196533283241418,6.47083650547062));
#17051=CARTESIAN_POINT('Ctrl Pts',(8.38946861452844,-0.00196662954943281,
6.47083652098856));
#17052=CARTESIAN_POINT('Ctrl Pts',(8.38940224472119,-0.134697483397542,
6.47751946712156));
#17053=CARTESIAN_POINT('Ctrl Pts',(8.3826120138021,-0.267199067172086,6.48420241325457));
#17054=CARTESIAN_POINT('Ctrl Pts',(8.36919582435493,-0.398821550545337,
6.49088535938758));
#17055=CARTESIAN_POINT('Ctrl Pts',(8.35619499781929,-0.526369024532905,
6.49736140266085));
#17056=CARTESIAN_POINT('Ctrl Pts',(8.33697255677429,-0.653090823469789,
6.50383744593412));
#17057=CARTESIAN_POINT('Ctrl Pts',(8.31166870378154,-0.778411885153282,
6.51031348920739));
#17058=CARTESIAN_POINT('Ctrl Pts',(8.28515220303635,-0.909738763572521,
6.51709988677027));
#17059=CARTESIAN_POINT('Ctrl Pts',(8.25195718178392,-1.03952699090368,6.52388628433315));
#17060=CARTESIAN_POINT('Ctrl Pts',(8.21230166279796,-1.1671378697206,6.53067268189603));
#17061=CARTESIAN_POINT('Ctrl Pts',(8.17264614381199,-1.29474874853751,6.53745907945891));
#17062=CARTESIAN_POINT('Ctrl Pts',(8.12653032448532,-1.42018201414962,6.54424547702179));
#17063=CARTESIAN_POINT('Ctrl Pts',(8.07422738824537,-1.5428266308384,6.55103187458467));
#17064=CARTESIAN_POINT('Ctrl Pts',(8.02895871678309,-1.64897667247336,6.55690556397521));
#17065=CARTESIAN_POINT('Ctrl Pts',(7.9789388073681,-1.75330944973437,6.56277925336574));
#17066=CARTESIAN_POINT('Ctrl Pts',(7.92433492144924,-1.85536942077644,6.56865294275628));
#17067=CARTESIAN_POINT('Ctrl Pts',(7.86980153427699,-1.95729762280764,6.57451904866199));
#17068=CARTESIAN_POINT('Ctrl Pts',(7.8106961333658,-2.05695849323454,6.58038515456771));
#17069=CARTESIAN_POINT('Ctrl Pts',(7.74723415481786,-2.15391606032251,6.58625126047342));
#17070=CARTESIAN_POINT('Ctrl Pts',(7.68383716052746,-2.25077434409698,6.59211135956142));
#17071=CARTESIAN_POINT('Ctrl Pts',(7.61609268697309,-2.34493448698235,6.59797145864942));
#17072=CARTESIAN_POINT('Ctrl Pts',(7.54426190722241,-2.43598534849183,6.60383155773742));
#17073=CARTESIAN_POINT('Ctrl Pts',(7.46983963680992,-2.53032111736513,6.60990307583154));
#17074=CARTESIAN_POINT('Ctrl Pts',(7.39103085717528,-2.62131861918634,6.61597459392566));
#17075=CARTESIAN_POINT('Ctrl Pts',(7.30817516591715,-2.70855340524727,6.62204611201978));
#17076=CARTESIAN_POINT('Ctrl Pts',(7.22829654586318,-2.79265377572805,6.6278994756165));
#17077=CARTESIAN_POINT('Ctrl Pts',(7.14465713571739,-2.87325684652984,6.63375283921322));
#17078=CARTESIAN_POINT('Ctrl Pts',(7.05760146765486,-2.95001685389883,6.63960620280993));
#17079=CARTESIAN_POINT('Ctrl Pts',(6.97055887070799,-3.02676533601099,6.6454586875438));
#17080=CARTESIAN_POINT('Ctrl Pts',(6.88010134556457,-3.09967162886433,6.65131117227766));
#17081=CARTESIAN_POINT('Ctrl Pts',(6.78660845297658,-3.16842857339228,6.65716365701153));
#17082=CARTESIAN_POINT('Ctrl Pts',(6.69310698834552,-3.23719182200896,6.66301667833968));
#17083=CARTESIAN_POINT('Ctrl Pts',(6.59656993587893,-3.30180472123734,6.66886969966782));
#17084=CARTESIAN_POINT('Ctrl Pts',(6.49740734899187,-3.36200239279869,6.67472272099596));
#17085=CARTESIAN_POINT('Ctrl Pts',(6.39821168946716,-3.42222014144598,6.68057769441975));
#17086=CARTESIAN_POINT('Ctrl Pts',(6.2963891072718,-3.47801952002286,6.68643266784353));
#17087=CARTESIAN_POINT('Ctrl Pts',(6.19237522048142,-3.52918106116189,6.69228764126732));
#17088=CARTESIAN_POINT('Ctrl Pts',(6.08824344731042,-3.58040058733635,6.69814925055144));
#17089=CARTESIAN_POINT('Ctrl Pts',(5.98191578343647,-3.62697160217744,6.70401085983556));
#17090=CARTESIAN_POINT('Ctrl Pts',(5.87384892563323,-3.66872231812591,6.70987246911968));
#17091=CARTESIAN_POINT('Ctrl Pts',(5.7657091975541,-3.71050118688877,6.71573803092999));
#17092=CARTESIAN_POINT('Ctrl Pts',(5.6558283309636,-3.74745315320136,6.72160359274029));
#17093=CARTESIAN_POINT('Ctrl Pts',(5.54467765156527,-3.7794564638098,6.7274691545506));
#17094=CARTESIAN_POINT('Ctrl Pts',(5.43336444261215,-3.81150657110769,6.7333432932509));
#17095=CARTESIAN_POINT('Ctrl Pts',(5.32077811532862,-3.83859348489971,6.7392174319512));
#17096=CARTESIAN_POINT('Ctrl Pts',(5.20739969924563,-3.86064660963103,6.7450915706515));
#17097=CARTESIAN_POINT('Ctrl Pts',(5.17872814872826,-3.86622348485688,6.74657704443311));
#17098=CARTESIAN_POINT('Ctrl Pts',(5.15000596460422,-3.8714787079246,6.74806251821472));
#17099=CARTESIAN_POINT('Ctrl Pts',(5.12124095466385,-3.87641166409274,6.74954799199633));
#17100=CARTESIAN_POINT('Ctrl Pts',(5.00750166434592,-3.89591699139477,6.75542168138689));
#17101=CARTESIAN_POINT('Ctrl Pts',(4.89271374425863,-3.91044465986001,6.76129537077745));
#17102=CARTESIAN_POINT('Ctrl Pts',(4.77735066381133,-3.91988826702964,6.76716906016801));
#17103=CARTESIAN_POINT('Ctrl Pts',(4.66213652793885,-3.92931968161522,6.77303516607376));
#17104=CARTESIAN_POINT('Ctrl Pts',(4.54634911647336,-3.93368005515109,6.7789012719795));
#17105=CARTESIAN_POINT('Ctrl Pts',(4.43047156984463,-3.93291407586061,6.78476737788524));
#17106=CARTESIAN_POINT('Ctrl Pts',(4.31471268034736,-3.93214888092316,6.79062747697327));
#17107=CARTESIAN_POINT('Ctrl Pts',(4.19886424995417,-3.92626777720655,6.79648757606131));
#17108=CARTESIAN_POINT('Ctrl Pts',(4.08341334764641,-3.91526734732079,6.80234767514934));
#17109=CARTESIAN_POINT('Ctrl Pts',(3.96379724016887,-3.90387004702073,6.80841919324345));
#17110=CARTESIAN_POINT('Ctrl Pts',(3.84460833632183,-3.88697702228025,6.81449071133756));
#17111=CARTESIAN_POINT('Ctrl Pts',(3.72638740277365,-3.86464354194477,6.82056222943167));
#17112=CARTESIAN_POINT('Ctrl Pts',(3.61241424184788,-3.84311252140626,6.82641559302841));
#17113=CARTESIAN_POINT('Ctrl Pts',(3.49934112920872,-3.81652536002302,6.83226895662515));
#17114=CARTESIAN_POINT('Ctrl Pts',(3.38764538702075,-3.78498412906591,6.8381223202219));
#17115=CARTESIAN_POINT('Ctrl Pts',(3.27596641557261,-3.75344763391849,6.84397480495579));
#17116=CARTESIAN_POINT('Ctrl Pts',(3.16566480085435,-3.71695866046953,6.84982728968969));
#17117=CARTESIAN_POINT('Ctrl Pts',(3.05720441453362,-3.67566964274603,6.85567977442358));
#17118=CARTESIAN_POINT('Ctrl Pts',(2.94873408385168,-3.63437683937396,6.86153279575175));
#17119=CARTESIAN_POINT('Ctrl Pts',(2.84210570329225,-3.58828326384537,6.86738581707992));
#17120=CARTESIAN_POINT('Ctrl Pts',(2.73776414600782,-3.53758989422856,6.87323883840809));
#17121=CARTESIAN_POINT('Ctrl Pts',(2.633387788799,-3.486879617394,6.8790938118319));
#17122=CARTESIAN_POINT('Ctrl Pts',(2.53130014286779,-3.43156667638692,6.88494878525572));
#17123=CARTESIAN_POINT('Ctrl Pts',(2.43192178106723,-3.37189814914743,6.89080375867953));
#17124=CARTESIAN_POINT('Ctrl Pts',(2.33243078665827,-3.31216199529646,6.89666536796368));
#17125=CARTESIAN_POINT('Ctrl Pts',(2.23565555956539,-3.2480606150503,6.90252697724783));
#17126=CARTESIAN_POINT('Ctrl Pts',(2.14198803388732,-3.17988464662193,6.90838858653197));
#17127=CARTESIAN_POINT('Ctrl Pts',(2.04825734750881,-3.11166270663737,6.91425414834231));
#17128=CARTESIAN_POINT('Ctrl Pts',(1.95763885738999,-3.0393609645716,6.92011971015264));
#17129=CARTESIAN_POINT('Ctrl Pts',(1.87049038389219,-2.96330947551498,6.92598527196297));
#17130=CARTESIAN_POINT('Ctrl Pts',(1.78321447795156,-2.8871467805285,6.93185941066329));
#17131=CARTESIAN_POINT('Ctrl Pts',(1.69941901290558,-2.80722367981402,6.93773354936362));
#17132=CARTESIAN_POINT('Ctrl Pts',(1.61942408143677,-2.72390611573943,6.94360768806394));
#17133=CARTESIAN_POINT('Ctrl Pts',(1.5991946691944,-2.70283646395339,6.94509316184529));
#17134=CARTESIAN_POINT('Ctrl Pts',(1.57920809482474,-2.68154989365626,6.94657863562664));
#17135=CARTESIAN_POINT('Ctrl Pts',(1.55946910757725,-2.66005263253832,6.94806410940799));
#17136=CARTESIAN_POINT('Ctrl Pts',(1.48141947692606,-2.57505063779408,6.95393779879857));
#17137=CARTESIAN_POINT('Ctrl Pts',(1.40698413988467,-2.48646903502784,6.95981148818915));
#17138=CARTESIAN_POINT('Ctrl Pts',(1.33650917954418,-2.39464800251476,6.96568517757973));
#17139=CARTESIAN_POINT('Ctrl Pts',(1.26612520899834,-2.30294551958089,6.9715512834855));
#17140=CARTESIAN_POINT('Ctrl Pts',(1.1996916958887,-2.20801224908382,6.97741738939126));
#17141=CARTESIAN_POINT('Ctrl Pts',(1.13751703415736,-2.11022419267781,6.98328349529703));
#17142=CARTESIAN_POINT('Ctrl Pts',(1.07540603848755,-2.01253626999577,6.98914359438508));
#17143=CARTESIAN_POINT('Ctrl Pts',(1.01754544013918,-1.9119997225896,6.99500369347313));
#17144=CARTESIAN_POINT('Ctrl Pts',(0.964202155499195,-1.80902198574683,
7.00086379256118));
#17145=CARTESIAN_POINT('Ctrl Pts',(0.908934366845095,-1.70232904708896,
7.00693531065528));
#17146=CARTESIAN_POINT('Ctrl Pts',(0.858516269715577,-1.59301580650514,
7.01300682874938));
#17147=CARTESIAN_POINT('Ctrl Pts',(0.813194576020285,-1.48156663623706,
7.01907834684348));
#17148=CARTESIAN_POINT('Ctrl Pts',(0.769501326999528,-1.37412192372434,
7.02493171044025));
#17149=CARTESIAN_POINT('Ctrl Pts',(0.730544717543736,-1.2646925468088,7.03078507403701));
#17150=CARTESIAN_POINT('Ctrl Pts',(0.696497737248281,-1.15373493685772,
7.03663843763377));
#17151=CARTESIAN_POINT('Ctrl Pts',(0.662455868992337,-1.04279398681836,
7.04249092236769));
#17152=CARTESIAN_POINT('Ctrl Pts',(0.633322285299647,-0.930325654857197,
7.04834340710161));
#17153=CARTESIAN_POINT('Ctrl Pts',(0.60922036390406,-0.816802371912494,
7.05419589183553));
#17154=CARTESIAN_POINT('Ctrl Pts',(0.585116232685891,-0.703268680406987,
7.06004891316371));
#17155=CARTESIAN_POINT('Ctrl Pts',(0.566044766663728,-0.588680249797354,
7.0659019344919));
#17156=CARTESIAN_POINT('Ctrl Pts',(0.552078252356837,-0.473519862606984,
7.07175495582009));
#17157=CARTESIAN_POINT('Ctrl Pts',(0.538107079947701,-0.358321067203494,
7.07760992924392));
#17158=CARTESIAN_POINT('Ctrl Pts',(0.529244294512347,-0.242550345822682,
7.08346490266776));
#17159=CARTESIAN_POINT('Ctrl Pts',(0.525510271062557,-0.126695052434562,
7.08931987609159));
#17160=CARTESIAN_POINT('Ctrl Pts',(0.521772015576805,-0.0107084519524598,
7.09518148537576));
#17161=CARTESIAN_POINT('Ctrl Pts',(0.523174137377517,0.105362498689283,
7.10104309465992));
#17162=CARTESIAN_POINT('Ctrl Pts',(0.529684882096246,0.221030896452396,
7.10690470394409));
#17163=CARTESIAN_POINT('Ctrl Pts',(0.536200017057955,0.336777290265595,
7.11277026575444));
#17164=CARTESIAN_POINT('Ctrl Pts',(0.547830592916088,0.452120180650977,
7.1186358275648));
#17165=CARTESIAN_POINT('Ctrl Pts',(0.564493239609307,0.566579962347384,
7.12450138937515));
#17166=CARTESIAN_POINT('Ctrl Pts',(0.581180251178772,0.681207112317725,
7.1303755280755));
#17167=CARTESIAN_POINT('Ctrl Pts',(0.602913941301662,0.794948172202939,
7.13624966677584));
#17168=CARTESIAN_POINT('Ctrl Pts',(0.629560331022235,0.907335784771954,
7.14212380547619));
#17169=CARTESIAN_POINT('Ctrl Pts',(0.636298767976385,0.935756777246556,
7.14360927925734));
#17170=CARTESIAN_POINT('Ctrl Pts',(0.64335112797796,0.964091304739122,7.14509475303849));
#17171=CARTESIAN_POINT('Ctrl Pts',(0.650714752463244,0.992332000327921,
7.14658022681964));
#17172=CARTESIAN_POINT('Ctrl Pts',(0.679831148568076,1.10399810724073,7.1524539162102));
#17173=CARTESIAN_POINT('Ctrl Pts',(0.713914860325132,1.21456763442555,7.15832760560076));
#17174=CARTESIAN_POINT('Ctrl Pts',(0.752867648195629,1.32356535166675,7.16420129499132));
#17175=CARTESIAN_POINT('Ctrl Pts',(0.791770144357513,1.43242234261505,7.17006740089707));
#17176=CARTESIAN_POINT('Ctrl Pts',(0.835529077210374,1.53971117384574,7.17593350680282));
#17177=CARTESIAN_POINT('Ctrl Pts',(0.883995672902733,1.64496886543632,7.18179961270856));
#17178=CARTESIAN_POINT('Ctrl Pts',(0.932412639418556,1.75011877449166,7.1876597117966));
#17179=CARTESIAN_POINT('Ctrl Pts',(0.985527508457297,1.85324130788033,7.19351981088463));
#17180=CARTESIAN_POINT('Ctrl Pts',(1.04314260686162,1.95389129912333,7.19937990997266));
#17181=CARTESIAN_POINT('Ctrl Pts',(1.10283632657537,2.0581725124311,7.20545142806677));
#17182=CARTESIAN_POINT('Ctrl Pts',(1.16736097046048,2.15979898249002,7.21152294616088));
#17183=CARTESIAN_POINT('Ctrl Pts',(1.236443261594,2.25830081254732,7.21759446425499));
#17184=CARTESIAN_POINT('Ctrl Pts',(1.30304337079782,2.35326339312984,7.22344782785173));
#17185=CARTESIAN_POINT('Ctrl Pts',(1.37387898643177,2.4453216437655,7.22930119144848));
#17186=CARTESIAN_POINT('Ctrl Pts',(1.44866034494117,2.53408276415449,7.23515455504522));
#17187=CARTESIAN_POINT('Ctrl Pts',(1.52343047528123,2.62283055735992,7.24100703977912));
#17188=CARTESIAN_POINT('Ctrl Pts',(1.6021449043803,2.70828188879732,7.24685952451301));
#17189=CARTESIAN_POINT('Ctrl Pts',(1.68447352905669,2.79007697388383,7.25271200924691));
#17190=CARTESIAN_POINT('Ctrl Pts',(1.76680970216264,2.87187955848148,7.25856503057508));
#17191=CARTESIAN_POINT('Ctrl Pts',(1.852760436483,2.95002493912258,7.26441805190325));
#17192=CARTESIAN_POINT('Ctrl Pts',(1.94195923328449,3.02419065188005,7.27027107323143));
#17193=CARTESIAN_POINT('Ctrl Pts',(2.03118777960722,3.09838110033492,7.27612604665524));
#17194=CARTESIAN_POINT('Ctrl Pts',(2.12366622498109,3.1685889776411,7.28198102007905));
#17195=CARTESIAN_POINT('Ctrl Pts',(2.21899608752842,3.23453296329393,7.28783599350286));
#17196=CARTESIAN_POINT('Ctrl Pts',(2.31443399423034,3.30055168798435,7.29369760278701));
#17197=CARTESIAN_POINT('Ctrl Pts',(2.41272942845047,3.36229664032718,7.29955921207116));
#17198=CARTESIAN_POINT('Ctrl Pts',(2.51345602739979,3.41953054899944,7.30542082135531));
#17199=CARTESIAN_POINT('Ctrl Pts',(2.61425054703449,3.47680305091663,7.31128638316564));
#17200=CARTESIAN_POINT('Ctrl Pts',(2.71747912873537,3.52955826466073,7.31715194497597));
#17201=CARTESIAN_POINT('Ctrl Pts',(2.82269356073474,3.5776062481749,7.32301750678631));
#17202=CARTESIAN_POINT('Ctrl Pts',(2.92806184203923,3.62572448962551,7.32889164548664));
#17203=CARTESIAN_POINT('Ctrl Pts',(3.03542138733468,3.66912160962264,7.33476578418696));
#17204=CARTESIAN_POINT('Ctrl Pts',(3.14430684140617,3.70765683293414,7.34063992288729));
#17205=CARTESIAN_POINT('Ctrl Pts',(3.1718421951735,3.71740176181774,7.34212539666862));
#17206=CARTESIAN_POINT('Ctrl Pts',(3.19947507240767,3.72683602521197,7.34361087044995));
#17207=CARTESIAN_POINT('Ctrl Pts',(3.22719784139387,3.73595786345043,7.34509634423129));
#17208=CARTESIAN_POINT('Ctrl Pts',(3.33681602255434,3.77202638593596,7.35097003362186));
#17209=CARTESIAN_POINT('Ctrl Pts',(3.44820556822354,3.80332636779926,7.35684372301242));
#17210=CARTESIAN_POINT('Ctrl Pts',(3.56091388213373,3.82968273367585,7.36271741240299));
#17211=CARTESIAN_POINT('Ctrl Pts',(3.67347667902218,3.85600507100802,7.36858351830874));
#17212=CARTESIAN_POINT('Ctrl Pts',(3.78735445951403,3.8773963921816,7.3744496242145));
#17213=CARTESIAN_POINT('Ctrl Pts',(3.90207752622745,3.89373072721205,7.38031573012025));
#17214=CARTESIAN_POINT('Ctrl Pts',(4.01668311798205,3.91004833609152,7.38617582920829));
#17215=CARTESIAN_POINT('Ctrl Pts',(4.13213186769417,3.92131920098428,7.39203592829633));
#17216=CARTESIAN_POINT('Ctrl Pts',(4.24794253797954,3.92746809921336,7.39789602738437));
#17217=CARTESIAN_POINT('Ctrl Pts',(4.36793139304236,3.93383883566267,7.40396754547847));
#17218=CARTESIAN_POINT('Ctrl Pts',(4.48830833646111,3.93471094705703,7.41003906357258));
#17219=CARTESIAN_POINT('Ctrl Pts',(4.608530364288,3.93005933464041,7.41611058166669));
#17220=CARTESIAN_POINT('Ctrl Pts',(4.724432718576,3.9255748583754,7.42196394526344));
#17221=CARTESIAN_POINT('Ctrl Pts',(4.84019064993848,3.91595678793296,7.42781730886019));
#17222=CARTESIAN_POINT('Ctrl Pts',(4.95531700162222,3.90123567312346,7.43367067245694));
#17223=CARTESIAN_POINT('Ctrl Pts',(5.07042606747164,3.88651676863981,7.43952315719084));
#17224=CARTESIAN_POINT('Ctrl Pts',(5.18490333250089,3.8666963956801,7.44537564192474));
#17225=CARTESIAN_POINT('Ctrl Pts',(5.29826751482728,3.84185689989402,7.45122812665864));
#17226=CARTESIAN_POINT('Ctrl Pts',(5.41164209112713,3.81701512665969,7.45708114798682));
#17227=CARTESIAN_POINT('Ctrl Pts',(5.52390297825591,3.78715340422412,7.46293416931499));
#17228=CARTESIAN_POINT('Ctrl Pts',(5.63458052479618,3.75240489358708,7.46878719064317));
#17229=CARTESIAN_POINT('Ctrl Pts',(5.74529498443553,3.71764479365072,7.47464216406698));
#17230=CARTESIAN_POINT('Ctrl Pts',(5.85442465947203,3.67799478834106,7.4804971374908));
#17231=CARTESIAN_POINT('Ctrl Pts',(5.96151713326215,3.63363721858571,7.48635211091462));
#17232=CARTESIAN_POINT('Ctrl Pts',(6.06873098261585,3.58922937522253,7.49221372019877));
#17233=CARTESIAN_POINT('Ctrl Pts',(6.17390264037431,3.54010347642467,7.49807532948292));
#17234=CARTESIAN_POINT('Ctrl Pts',(6.2766015902598,3.48648917114864,7.50393693876707));
#17235=CARTESIAN_POINT('Ctrl Pts',(6.37936979080141,3.43283871335283,7.50980250057741));
#17236=CARTESIAN_POINT('Ctrl Pts',(6.47966160683954,3.37469402921962,7.51566806238775));
#17237=CARTESIAN_POINT('Ctrl Pts',(6.57707444871111,3.31232878521906,7.52153362419809));
#17238=CARTESIAN_POINT('Ctrl Pts',(6.67462973204956,3.24987234793569,7.52740776289841));
#17239=CARTESIAN_POINT('Ctrl Pts',(6.76929730313146,3.1831832710523,7.53328190159875));
#17240=CARTESIAN_POINT('Ctrl Pts',(6.86070659393655,3.11257628061546,7.53915604029908));
#17241=CARTESIAN_POINT('Ctrl Pts',(6.88382251131349,3.0947209254016,7.54064151408037));
#17242=CARTESIAN_POINT('Ctrl Pts',(6.90673024244077,3.07661520573675,7.54212698786166));
#17243=CARTESIAN_POINT('Ctrl Pts',(6.92942417143176,3.05826458067886,7.54361246164295));
#17244=CARTESIAN_POINT('Ctrl Pts',(7.01799445038805,2.98664542733415,7.54940999574309));
#17245=CARTESIAN_POINT('Ctrl Pts',(7.10361700632803,2.91104090485563,7.55520752984322));
#17246=CARTESIAN_POINT('Ctrl Pts',(7.18590465504607,2.83172572555942,7.56100506394336));
#17247=CARTESIAN_POINT('Ctrl Pts',(7.26808555473045,2.752513439211,7.56679507709506));
#17248=CARTESIAN_POINT('Ctrl Pts',(7.34693984312148,2.66960035561418,7.57258509024676));
#17249=CARTESIAN_POINT('Ctrl Pts',(7.42211184837868,2.5833025618133,7.57837510339846));
#17250=CARTESIAN_POINT('Ctrl Pts',(7.49917778727706,2.49483052383362,7.58431099400353));
#17251=CARTESIAN_POINT('Ctrl Pts',(7.57237304629976,2.40280120236074,7.59024688460859));
#17252=CARTESIAN_POINT('Ctrl Pts',(7.64135273563583,2.30759729308818,7.59618277521365));
#17253=CARTESIAN_POINT('Ctrl Pts',(7.70851969504273,2.21489526483849,7.60196267545894));
#17254=CARTESIAN_POINT('Ctrl Pts',(7.77168962164127,2.11918379008929,7.60774257570424));
#17255=CARTESIAN_POINT('Ctrl Pts',(7.83058414359826,2.02085049286832,7.61352247594953));
#17256=CARTESIAN_POINT('Ctrl Pts',(7.88945761009809,1.92255235091234,7.61930030981517));
#17257=CARTESIAN_POINT('Ctrl Pts',(7.94405849151773,1.82163461327772,7.62507814368081));
#17258=CARTESIAN_POINT('Ctrl Pts',(7.99415212720601,1.71851326530083,7.63085597754645));
#17259=CARTESIAN_POINT('Ctrl Pts',(8.04424071635473,1.6154023059882,7.6366332293408));
#17260=CARTESIAN_POINT('Ctrl Pts',(8.0898227776142,1.51008856014189,7.64241048113515));
#17261=CARTESIAN_POINT('Ctrl Pts',(8.13071034258294,1.40301116780918,7.6481877329295));
#17262=CARTESIAN_POINT('Ctrl Pts',(8.17355698758577,1.2908032869873,7.65424179501204));
#17263=CARTESIAN_POINT('Ctrl Pts',(8.21124789224062,1.1766590224032,7.66029585709457));
#17264=CARTESIAN_POINT('Ctrl Pts',(8.24362463857504,1.0611041295459,7.66634991917711));
#17265=CARTESIAN_POINT('Ctrl Pts',(8.27455419731127,0.950714351370795,7.67213337458799));
#17266=CARTESIAN_POINT('Ctrl Pts',(8.30063436669227,0.839037768841426,7.67791682999887));
#17267=CARTESIAN_POINT('Ctrl Pts',(8.32177926695921,0.726544122041247,7.68370028540975));
#17268=CARTESIAN_POINT('Ctrl Pts',(8.34293597481183,0.613987657334305,7.68948697037691));
#17269=CARTESIAN_POINT('Ctrl Pts',(8.35915186896831,0.500613639988626,7.69527365534406));
#17270=CARTESIAN_POINT('Ctrl Pts',(8.370392900461,0.386897315654267,7.70106034031121));
#17271=CARTESIAN_POINT('Ctrl Pts',(8.38164815637142,0.273037094516247,7.70685434775802));
#17272=CARTESIAN_POINT('Ctrl Pts',(8.38791597036706,0.158834124771027,7.71264835520482));
#17273=CARTESIAN_POINT('Ctrl Pts',(8.38921435632238,0.0447637999217728,
7.71844236265162));
#17274=CARTESIAN_POINT('Ctrl Pts',(8.38939318969279,0.0290523078391149,
7.71924040107439));
#17275=CARTESIAN_POINT('Ctrl Pts',(8.38947782861755,0.0133433237550547,
7.72003843949716));
#17276=CARTESIAN_POINT('Ctrl Pts',(8.38946839700585,-0.00236191960000097,
7.72083647791993));
#17277=CARTESIAN_POINT('',(8.38897355277412,0.00337481364521056,5.22083644943854));
#17278=CARTESIAN_POINT('Ctrl Pts',(8.38695162751728,0.00337251368749724,
5.22083647796503));
#17279=CARTESIAN_POINT('Ctrl Pts',(8.37945749364734,-0.914486619189309,
5.2672027086816));
#17280=CARTESIAN_POINT('Ctrl Pts',(7.6012952590149,-3.15372830043783,5.37974097853539));
#17281=CARTESIAN_POINT('Ctrl Pts',(3.87112667961493,-4.61205589356117,5.55845128752638));
#17282=CARTESIAN_POINT('Ctrl Pts',(0.263602650510944,-2.00837153064666,
5.75696740493805));
#17283=CARTESIAN_POINT('Ctrl Pts',(0.495825964855193,2.43454127651753,5.95548352234969));
#17284=CARTESIAN_POINT('Ctrl Pts',(4.35513092859251,4.64794749265716,6.15399963976136));
#17285=CARTESIAN_POINT('Ctrl Pts',(7.77505612682836,2.87997114683924,6.32578395829981));
#17286=CARTESIAN_POINT('Ctrl Pts',(8.38045329723552,0.780274519420981,6.43139623770103));
#17287=CARTESIAN_POINT('Ctrl Pts',(8.38398528402403,-0.00196303439876837,
6.47083647796504));
#17288=CARTESIAN_POINT('Ctrl Pts',(7.19731080507723,-2.82068711164422,4.12982512801404));
#17289=CARTESIAN_POINT('Ctrl Pts',(7.11420835835676,-2.90143717084377,4.13568811753562));
#17290=CARTESIAN_POINT('Ctrl Pts',(7.02761824116375,-2.97843011948875,4.1415511070572));
#17291=CARTESIAN_POINT('Ctrl Pts',(6.93792639155195,-3.05136997774185,4.14741409657878));
#17292=CARTESIAN_POINT('Ctrl Pts',(6.84810427325219,-3.12441577404479,4.1532856015224));
#17293=CARTESIAN_POINT('Ctrl Pts',(6.75517176325591,-3.19339648709836,4.15915710646601));
#17294=CARTESIAN_POINT('Ctrl Pts',(6.65954368229696,-3.25805945498783,4.16502861140963));
#17295=CARTESIAN_POINT('Ctrl Pts',(6.63886022591221,-3.27204544804174,4.16629856282135));
#17296=CARTESIAN_POINT('Ctrl Pts',(6.61805075562464,-3.28582962195859,4.16756851423307));
#17297=CARTESIAN_POINT('Ctrl Pts',(6.59711961001077,-3.29940970790425,4.1688384656448));
#17298=CARTESIAN_POINT('Ctrl Pts',(6.50031035698119,-3.36221936011964,4.1747121550176));
#17299=CARTESIAN_POINT('Ctrl Pts',(6.40057314255717,-3.42086923425397,4.1805858443904));
#17300=CARTESIAN_POINT('Ctrl Pts',(6.29830101265205,-3.47507470832534,4.1864595337632));
#17301=CARTESIAN_POINT('Ctrl Pts',(6.19616092567059,-3.52921019803947,4.19232563965145));
#17302=CARTESIAN_POINT('Ctrl Pts',(6.09149279346964,-3.57891250725582,4.19819174553969));
#17303=CARTESIAN_POINT('Ctrl Pts',(5.98471871108655,-3.6239401409543,4.20405785142794));
#17304=CARTESIAN_POINT('Ctrl Pts',(5.878053963999,-3.66892166693144,4.20991795049874));
#17305=CARTESIAN_POINT('Ctrl Pts',(5.76928793453597,-3.70923787916653,4.21577804956954));
#17306=CARTESIAN_POINT('Ctrl Pts',(5.65886680768961,-3.74469341435269,4.22163814864034));
#17307=CARTESIAN_POINT('Ctrl Pts',(5.54446193803734,-3.7814281045091,4.22770966674101));
#17308=CARTESIAN_POINT('Ctrl Pts',(5.42828069101142,-3.81294455993941,4.23378118484168));
#17309=CARTESIAN_POINT('Ctrl Pts',(5.31084175137267,-3.83908014805784,4.23985270294235));
#17310=CARTESIAN_POINT('Ctrl Pts',(5.19762248713018,-3.86427666351018,4.24570606652268));
#17311=CARTESIAN_POINT('Ctrl Pts',(5.08323479251593,-3.88447223731615,4.251559430103));
#17312=CARTESIAN_POINT('Ctrl Pts',(4.96815752828476,-3.89957227894587,4.25741279368332));
#17313=CARTESIAN_POINT('Ctrl Pts',(4.85309754251115,-3.91467005335599,4.26326527840112));
#17314=CARTESIAN_POINT('Ctrl Pts',(4.73734860251363,-3.92467376311349,4.26911776311893));
#17315=CARTESIAN_POINT('Ctrl Pts',(4.62139708614469,-3.92954040078956,4.27497024783673));
#17316=CARTESIAN_POINT('Ctrl Pts',(4.50543493857151,-3.93440748467126,4.28082326914916));
#17317=CARTESIAN_POINT('Ctrl Pts',(4.38927059050865,-3.93413654283997,4.28667629046159));
#17318=CARTESIAN_POINT('Ctrl Pts',(4.27339212145814,-3.92873666942074,4.29252931177402));
#17319=CARTESIAN_POINT('Ctrl Pts',(4.15747500469308,-3.92333499503909,4.29838428518246));
#17320=CARTESIAN_POINT('Ctrl Pts',(4.04184436900636,-3.91280100684266,4.3042392585909));
#17321=CARTESIAN_POINT('Ctrl Pts',(3.92698415951086,-3.89719574709948,4.31009423199933));
#17322=CARTESIAN_POINT('Ctrl Pts',(3.81199377070867,-3.8815728007971,4.31595584126872));
#17323=CARTESIAN_POINT('Ctrl Pts',(3.69777596052368,-3.86086716666494,4.32181745053811));
#17324=CARTESIAN_POINT('Ctrl Pts',(3.58480555111573,-3.83519121383876,4.3276790598075));
#17325=CARTESIAN_POINT('Ctrl Pts',(3.47175896492413,-3.80949794752744,4.33354462160343));
#17326=CARTESIAN_POINT('Ctrl Pts',(3.35996185182716,-3.77882779792911,4.33941018339935));
#17327=CARTESIAN_POINT('Ctrl Pts',(3.24987324524777,-3.74334281468969,4.34527574519528));
#17328=CARTESIAN_POINT('Ctrl Pts',(3.13962366211244,-3.70780594369759,4.35114988388182));
#17329=CARTESIAN_POINT('Ctrl Pts',(3.03108795712803,-3.6674403315217,4.35702402256836));
#17330=CARTESIAN_POINT('Ctrl Pts',(2.92470466141453,-3.62245589146854,4.36289816125491));
#17331=CARTESIAN_POINT('Ctrl Pts',(2.89780205982261,-3.61108005976048,4.36438363518876));
#17332=CARTESIAN_POINT('Ctrl Pts',(2.87103697745075,-3.59940907998768,4.36586910912261));
#17333=CARTESIAN_POINT('Ctrl Pts',(2.84441623583233,-3.58744680003488,4.36735458305646));
#17334=CARTESIAN_POINT('Ctrl Pts',(2.73915557606051,-3.5401469352056,4.37322827239962));
#17335=CARTESIAN_POINT('Ctrl Pts',(2.63580313467552,-3.48813162622624,4.37910196174278));
#17336=CARTESIAN_POINT('Ctrl Pts',(2.53481115568846,-3.43157685636875,4.38497565108594));
#17337=CARTESIAN_POINT('Ctrl Pts',(2.43394956684899,-3.3750951040406,4.39084175694348));
#17338=CARTESIAN_POINT('Ctrl Pts',(2.33544273695223,-3.31408574620366,4.39670786280102));
#17339=CARTESIAN_POINT('Ctrl Pts',(2.23972241789224,-3.24877255587332,4.40257396865856));
#17340=CARTESIAN_POINT('Ctrl Pts',(2.14410011523251,-3.18352624542667,4.40843406769764));
#17341=CARTESIAN_POINT('Ctrl Pts',(2.05125898709741,-3.11398509999038,4.41429416673671));
#17342=CARTESIAN_POINT('Ctrl Pts',(1.96160507993493,-3.04041814399884,4.42015426577579));
#17343=CARTESIAN_POINT('Ctrl Pts',(1.86871666328278,-2.96419705920454,4.42622578388797));
#17344=CARTESIAN_POINT('Ctrl Pts',(1.77925017913452,-2.88365441584827,4.43229730200015));
#17345=CARTESIAN_POINT('Ctrl Pts',(1.69362347288065,-2.79913790413179,4.43836882011233));
#17346=CARTESIAN_POINT('Ctrl Pts',(1.61107340357164,-2.71765813917078,4.44422218365858));
#17347=CARTESIAN_POINT('Ctrl Pts',(1.53209224749404,-2.6324854749879,4.45007554720482));
#17348=CARTESIAN_POINT('Ctrl Pts',(1.45701908478339,-2.5439710235996,4.45592891075106));
#17349=CARTESIAN_POINT('Ctrl Pts',(1.38195719406189,-2.45546986236586,4.46178139543397));
#17350=CARTESIAN_POINT('Ctrl Pts',(1.31080239714504,-2.36362822660573,4.46763388011688));
#17351=CARTESIAN_POINT('Ctrl Pts',(1.24385450357439,-2.2688315087021,4.47348636479978));
#17352=CARTESIAN_POINT('Ctrl Pts',(1.17690047178557,-2.17402609921901,4.47933938607654));
#17353=CARTESIAN_POINT('Ctrl Pts',(1.11415434845501,-2.07626540647684,4.48519240735329));
#17354=CARTESIAN_POINT('Ctrl Pts',(1.05587308426051,-1.97596449751639,4.49104542863004));
#17355=CARTESIAN_POINT('Ctrl Pts',(0.997572382142501,-1.87563013627202,
4.49690040200206));
#17356=CARTESIAN_POINT('Ctrl Pts',(0.943739707656872,-1.77275423119346,
4.50275537537409));
#17357=CARTESIAN_POINT('Ctrl Pts',(0.894586117757878,-1.66777653674484,
4.5086103487461));
#17358=CARTESIAN_POINT('Ctrl Pts',(0.845376818580375,-1.56267986356792,
4.51447195797815));
#17359=CARTESIAN_POINT('Ctrl Pts',(0.800857364030778,-1.4554770208464,4.52033356721019));
#17360=CARTESIAN_POINT('Ctrl Pts',(0.761190735054206,-1.34662792173904,
4.52619517644224));
#17361=CARTESIAN_POINT('Ctrl Pts',(0.721497358579749,-1.23770542488845,
4.53206073820023));
#17362=CARTESIAN_POINT('Ctrl Pts',(0.686663447379408,-1.12713485430877,
4.53792629995823));
#17363=CARTESIAN_POINT('Ctrl Pts',(0.656801676251452,-1.01538978803684,
4.54379186171623));
#17364=CARTESIAN_POINT('Ctrl Pts',(0.626896239889432,-0.903481323068519,
4.54966600036426));
#17365=CARTESIAN_POINT('Ctrl Pts',(0.601977542229545,-0.790395336822605,
4.55554013901229));
#17366=CARTESIAN_POINT('Ctrl Pts',(0.582106923367081,-0.676614126435978,
4.56141427766032));
#17367=CARTESIAN_POINT('Ctrl Pts',(0.577081966551582,-0.647840706112964,
4.56289975192959));
#17368=CARTESIAN_POINT('Ctrl Pts',(0.572379575594817,-0.619022841674758,
4.56438522619885));
#17369=CARTESIAN_POINT('Ctrl Pts',(0.568000215107508,-0.590168351289692,
4.56587070046812));
#17370=CARTESIAN_POINT('Ctrl Pts',(0.550683857697303,-0.476075284540527,
4.57174438989032));
#17371=CARTESIAN_POINT('Ctrl Pts',(0.538364388507258,-0.361029421583703,
4.57761807931251));
#17372=CARTESIAN_POINT('Ctrl Pts',(0.531139093181675,-0.245506188830913,
4.58349176873471));
#17373=CARTESIAN_POINT('Ctrl Pts',(0.523923126390626,-0.130132107416246,
4.58935787467247));
#17374=CARTESIAN_POINT('Ctrl Pts',(0.521788279408659,-0.0142822904555608,
4.59522398061024));
#17375=CARTESIAN_POINT('Ctrl Pts',(0.524780570811782,0.101559148053415,
4.601090086548));
#17376=CARTESIAN_POINT('Ctrl Pts',(0.527769798146824,0.217281966412697,
4.6069501856684));
#17377=CARTESIAN_POINT('Ctrl Pts',(0.535875710330134,0.33299601283302,4.6128102847888));
#17378=CARTESIAN_POINT('Ctrl Pts',(0.549092365648309,0.448214242581623,
4.6186703839092));
#17379=CARTESIAN_POINT('Ctrl Pts',(0.562785847635657,0.567589282309495,
4.62474190199131));
#17380=CARTESIAN_POINT('Ctrl Pts',(0.58196583128496,0.686431603246408,4.63081342007342));
#17381=CARTESIAN_POINT('Ctrl Pts',(0.606566667743219,0.804201600485852,
4.63688493815552));
#17382=CARTESIAN_POINT('Ctrl Pts',(0.630283576667667,0.917740028469782,
4.64273830178528));
#17383=CARTESIAN_POINT('Ctrl Pts',(0.659038399718432,1.03028142638004,4.64859166541504));
#17384=CARTESIAN_POINT('Ctrl Pts',(0.692719913269095,1.14135052134503,4.6544450290448));
#17385=CARTESIAN_POINT('Ctrl Pts',(0.726396369654919,1.25240293966273,4.6602975138119));
#17386=CARTESIAN_POINT('Ctrl Pts',(0.764997925825997,1.36198309932832,4.666149998579));
#17387=CARTESIAN_POINT('Ctrl Pts',(0.808363263132728,1.46963014314666,4.6720024833461));
#17388=CARTESIAN_POINT('Ctrl Pts',(0.851732576459734,1.57728705675629,4.67785550470761));
#17389=CARTESIAN_POINT('Ctrl Pts',(0.899866384803132,1.68301011894143,4.68370852606913));
#17390=CARTESIAN_POINT('Ctrl Pts',(0.952555199468043,1.78635840023286,4.68956154743065));
#17391=CARTESIAN_POINT('Ctrl Pts',(1.00526158687103,1.88974115017363,4.69541652088792));
#17392=CARTESIAN_POINT('Ctrl Pts',(1.06252581387436,1.99074717642117,4.70127149434519));
#17393=CARTESIAN_POINT('Ctrl Pts',(1.12409276732383,2.08896073107578,4.70712646780246));
#17394=CARTESIAN_POINT('Ctrl Pts',(1.18572949900678,2.18728559817907,4.71298807712008));
#17395=CARTESIAN_POINT('Ctrl Pts',(1.25167847095215,2.28281132647617,4.71884968643769));
#17396=CARTESIAN_POINT('Ctrl Pts',(1.32164156803488,2.37515163849536,4.72471129575531));
#17397=CARTESIAN_POINT('Ctrl Pts',(1.3916518417479,2.46755421626525,4.73057685759914));
#17398=CARTESIAN_POINT('Ctrl Pts',(1.4656813671716,2.55676678356299,4.73644241944298));
#17399=CARTESIAN_POINT('Ctrl Pts',(1.54339327503609,2.64243792770661,4.74230798128681));
#17400=CARTESIAN_POINT('Ctrl Pts',(1.6212188167669,2.72823434407179,4.74818212002045));
#17401=CARTESIAN_POINT('Ctrl Pts',(1.70273719741743,2.81047871013839,4.7540562587541));
#17402=CARTESIAN_POINT('Ctrl Pts',(1.78757639195902,2.88885802347121,4.75993039748774));
#17403=CARTESIAN_POINT('Ctrl Pts',(1.80903083454441,2.90867886791542,4.76141587095175));
#17404=CARTESIAN_POINT('Ctrl Pts',(1.83069748965618,2.92825275158177,4.76290134441576));
#17405=CARTESIAN_POINT('Ctrl Pts',(1.85257003950644,2.94757504575836,4.76438681787977));
#17406=CARTESIAN_POINT('Ctrl Pts',(1.93905597614796,3.02397705290271,4.77026050726535));
#17407=CARTESIAN_POINT('Ctrl Pts',(2.02905141551935,3.09669665561652,4.77613419665092));
#17408=CARTESIAN_POINT('Ctrl Pts',(2.12220959255693,3.1653943708299,4.7820078860365));
#17409=CARTESIAN_POINT('Ctrl Pts',(2.21524749363605,3.23400339083902,4.78787399193727));
#17410=CARTESIAN_POINT('Ctrl Pts',(2.31143968238032,3.29860060683084,4.79374009783804));
#17411=CARTESIAN_POINT('Ctrl Pts',(2.41040430111351,3.35888490623179,4.7996062037388));
#17412=CARTESIAN_POINT('Ctrl Pts',(2.50926758133778,3.41910747527808,4.80546630282185));
#17413=CARTESIAN_POINT('Ctrl Pts',(2.61089729393848,3.47502569860976,4.8113264019049));
#17414=CARTESIAN_POINT('Ctrl Pts',(2.7148809503522,3.52638053751252,4.81718650098795));
#17415=CARTESIAN_POINT('Ctrl Pts',(2.82261609998951,3.57958814190542,4.82325801908393));
#17416=CARTESIAN_POINT('Ctrl Pts',(2.93287788661398,3.62789660396052,4.82932953717991));
#17417=CARTESIAN_POINT('Ctrl Pts',(3.04517728711491,3.67106856396499,4.83540105527589));
#17418=CARTESIAN_POINT('Ctrl Pts',(3.1534416802838,3.71268932089643,4.8412544188677));
#17419=CARTESIAN_POINT('Ctrl Pts',(3.2635993624148,3.74953617963213,4.84710778245952));
#17420=CARTESIAN_POINT('Ctrl Pts',(3.37519066260441,3.78144495231334,4.85296114605134));
#17421=CARTESIAN_POINT('Ctrl Pts',(3.48676520773655,3.81334893399992,4.85881363078035));
#17422=CARTESIAN_POINT('Ctrl Pts',(3.59977254580557,3.84031619033397,4.86466611550936));
#17423=CARTESIAN_POINT('Ctrl Pts',(3.71373796252527,3.86223244357308,4.87051860023837));
#17424=CARTESIAN_POINT('Ctrl Pts',(3.82771382834356,3.88415070623837,4.87637162156165));
#17425=CARTESIAN_POINT('Ctrl Pts',(3.94264754170268,3.90101696716596,4.88222464288493));
#17426=CARTESIAN_POINT('Ctrl Pts',(4.05805502030093,3.91276822929019,4.88807766420822));
#17427=CARTESIAN_POINT('Ctrl Pts',(4.17350098952296,3.92452341068737,4.89393263762719));
#17428=CARTESIAN_POINT('Ctrl Pts',(4.28942062738185,3.93116015924477,4.89978761104616));
#17429=CARTESIAN_POINT('Ctrl Pts',(4.40532627839294,3.93266746765628,4.90564258446514));
#17430=CARTESIAN_POINT('Ctrl Pts',(4.52136329357403,3.93417648440828,4.91150419374455));
#17431=CARTESIAN_POINT('Ctrl Pts',(4.637385876926,3.93054445212009,4.91736580302396));
#17432=CARTESIAN_POINT('Ctrl Pts',(4.75290782541861,3.92181247457841,4.92322741230336));
#17433=CARTESIAN_POINT('Ctrl Pts',(4.86850767121012,3.91307460900011,4.92909297410899));
#17434=CARTESIAN_POINT('Ctrl Pts',(4.98360580076896,3.8992299997122,4.93495853591461));
#17435=CARTESIAN_POINT('Ctrl Pts',(5.09772429923083,3.88037121644752,4.94082409772024));
#17436=CARTESIAN_POINT('Ctrl Pts',(5.21200966692894,3.86148485701594,4.94669823641595));
#17437=CARTESIAN_POINT('Ctrl Pts',(5.32531214201382,3.83756977586982,4.95257237511167));
#17438=CARTESIAN_POINT('Ctrl Pts',(5.43716702778179,3.80876890696206,4.95844651380739));
#17439=CARTESIAN_POINT('Ctrl Pts',(5.46545330325994,3.80148563715814,4.9599319876354));
#17440=CARTESIAN_POINT('Ctrl Pts',(5.49364709804283,3.79389016356313,4.96141746146341));
#17441=CARTESIAN_POINT('Ctrl Pts',(5.52174109764923,3.78598528579717,4.96290293529143));
#17442=CARTESIAN_POINT('Ctrl Pts',(5.63282715258497,3.75472872930564,4.96877662467622));
#17443=CARTESIAN_POINT('Ctrl Pts',(5.74272138899312,3.71852684366733,4.97465031406101));
#17444=CARTESIAN_POINT('Ctrl Pts',(5.85095055194696,3.67748698128469,4.9805240034458));
#17445=CARTESIAN_POINT('Ctrl Pts',(5.95903998088213,3.63650010522052,4.9863901093457));
#17446=CARTESIAN_POINT('Ctrl Pts',(6.06546822876711,3.59068781936645,4.9922562152456));
#17447=CARTESIAN_POINT('Ctrl Pts',(6.16977525966529,3.5402077657336,4.9981223211455));
#17448=CARTESIAN_POINT('Ctrl Pts',(6.27397548149021,3.48977940303377,5.00398242022755));
#17449=CARTESIAN_POINT('Ctrl Pts',(6.37605843714023,3.43469295874976,5.00984251930961));
#17450=CARTESIAN_POINT('Ctrl Pts',(6.47558284037743,3.37515462290689,5.01570261839166));
#17451=CARTESIAN_POINT('Ctrl Pts',(6.57869785717465,3.31346827965012,5.02177413648797));
#17452=CARTESIAN_POINT('Ctrl Pts',(6.67906580016466,3.24700291184717,5.02784565458427));
#17453=CARTESIAN_POINT('Ctrl Pts',(6.7762221100382,3.17604077449713,5.03391717268058));
#17454=CARTESIAN_POINT('Ctrl Pts',(6.86988751591982,3.10762836355058,5.03977053627116));
#17455=CARTESIAN_POINT('Ctrl Pts',(6.96056774764238,3.03503703141585,5.04562389986173));
#17456=CARTESIAN_POINT('Ctrl Pts',(7.04787564489083,2.95856403535989,5.05147726345231));
#17457=CARTESIAN_POINT('Ctrl Pts',(7.13517043315111,2.882102521468,5.05732974817995));
#17458=CARTESIAN_POINT('Ctrl Pts',(7.21909358303961,2.80176077466077,5.0631822329076));
#17459=CARTESIAN_POINT('Ctrl Pts',(7.29929171894275,2.71787575002653,5.06903471763525));
#17460=CARTESIAN_POINT('Ctrl Pts',(7.3794972079375,2.63398303426251,5.07488773895712));
#17461=CARTESIAN_POINT('Ctrl Pts',(7.45597671849276,2.54654669350122,5.08074076027899));
#17462=CARTESIAN_POINT('Ctrl Pts',(7.52841488805971,2.45593935459052,5.08659378160086));
#17463=CARTESIAN_POINT('Ctrl Pts',(7.60087721715508,2.36530179638255,5.09244875501837));
#17464=CARTESIAN_POINT('Ctrl Pts',(7.66929526724543,2.2714914595771,5.09830372843588));
#17465=CARTESIAN_POINT('Ctrl Pts',(7.73339542612834,2.1749121577389,5.10415870185339));
#17466=CARTESIAN_POINT('Ctrl Pts',(7.79756823430694,2.0782233956688,5.11002031113113));
#17467=CARTESIAN_POINT('Ctrl Pts',(7.8574131550048,1.97875974919543,5.11588192040887));
#17468=CARTESIAN_POINT('Ctrl Pts',(7.91270115276907,1.87695206129382,5.12174352968661));
#17469=CARTESIAN_POINT('Ctrl Pts',(7.96802643163604,1.77507572372099,5.12760909149051));
#17470=CARTESIAN_POINT('Ctrl Pts',(8.01878848855072,1.67085256789871,5.13347465329441));
#17471=CARTESIAN_POINT('Ctrl Pts',(8.06480602839219,1.56473437237006,5.13934021509831));
#17472=CARTESIAN_POINT('Ctrl Pts',(8.1108908571634,1.45846100601245,5.14521435379218));
#17473=CARTESIAN_POINT('Ctrl Pts',(8.15221717618438,1.35028745415923,5.15108849248606));
#17474=CARTESIAN_POINT('Ctrl Pts',(8.18865317747412,1.24068169095217,5.15696263117993));
#17475=CARTESIAN_POINT('Ctrl Pts',(8.19786724775897,1.21296418161894,5.15844810502098));
#17476=CARTESIAN_POINT('Ctrl Pts',(8.20676883607817,1.18515513589334,5.15993357886203));
#17477=CARTESIAN_POINT('Ctrl Pts',(8.21535632972457,1.15726221789226,5.16141905270308));
#17478=CARTESIAN_POINT('Ctrl Pts',(8.25675564365641,1.02279368535541,5.16858035033138));
#17479=CARTESIAN_POINT('Ctrl Pts',(8.29096263526288,0.886013494682714,5.17574164795968));
#17480=CARTESIAN_POINT('Ctrl Pts',(8.31775870655057,0.747617296727038,5.18290294558798));
#17481=CARTESIAN_POINT('Ctrl Pts',(8.34421505075933,0.610975719273807,5.18997345055125));
#17482=CARTESIAN_POINT('Ctrl Pts',(8.36344717827975,0.472758846995365,5.19704395551452));
#17483=CARTESIAN_POINT('Ctrl Pts',(8.37529061117875,0.333657027888083,5.20411446047779));
#17484=CARTESIAN_POINT('Ctrl Pts',(8.3846273168625,0.22399686802106,5.20968845447433));
#17485=CARTESIAN_POINT('Ctrl Pts',(8.38937290030595,0.113787124790175,5.21526244847088));
#17486=CARTESIAN_POINT('Ctrl Pts',(8.38946765781205,0.00337537569402483,
5.22083644246742));
#17487=CARTESIAN_POINT('Origin',(4.45646910621825,0.,0.));
#17488=CARTESIAN_POINT('Ctrl Pts',(6.97215211287823,3.02321484681493,3.97983001953316));
#17489=CARTESIAN_POINT('Ctrl Pts',(6.88323273247801,3.09720660246909,3.97396457891235));
#17490=CARTESIAN_POINT('Ctrl Pts',(6.79116193806773,3.16717580965372,3.96809913829154));
#17491=CARTESIAN_POINT('Ctrl Pts',(6.69635098528666,3.23286531854035,3.96223369767072));
#17492=CARTESIAN_POINT('Ctrl Pts',(6.66972216368927,3.25131502463075,3.96058631656864));
#17493=CARTESIAN_POINT('Ctrl Pts',(6.64287733814909,3.26942741083934,3.95893893546656));
#17494=CARTESIAN_POINT('Ctrl Pts',(6.61582595255236,3.28719744009848,3.95729155436448));
#17495=CARTESIAN_POINT('Ctrl Pts',(6.51937502447031,3.35055596226958,3.95141786498793));
#17496=CARTESIAN_POINT('Ctrl Pts',(6.41997255439171,3.40977140450338,3.94554417561138));
#17497=CARTESIAN_POINT('Ctrl Pts',(6.31800996521393,3.46455691687835,3.93967048623484));
#17498=CARTESIAN_POINT('Ctrl Pts',(6.21617901932698,3.51927169600501,3.93380438034361));
#17499=CARTESIAN_POINT('Ctrl Pts',(6.11179488822022,3.56956772563459,3.92793827445239));
#17500=CARTESIAN_POINT('Ctrl Pts',(6.005278288411,3.61520111711028,3.92207216856116));
#17501=CARTESIAN_POINT('Ctrl Pts',(5.89887076025228,3.66078778057049,3.91621206948815));
#17502=CARTESIAN_POINT('Ctrl Pts',(5.79033548429857,3.70172114098933,3.91035197041514));
#17503=CARTESIAN_POINT('Ctrl Pts',(5.68011752866518,3.73780330384614,3.90449187134213));
#17504=CARTESIAN_POINT('Ctrl Pts',(5.56592316024469,3.77518722895164,3.89842035324257));
#17505=CARTESIAN_POINT('Ctrl Pts',(5.4499228031593,3.80736309347115,3.89234883514302));
#17506=CARTESIAN_POINT('Ctrl Pts',(5.33263421003588,3.83416532127297,3.88627731704346));
#17507=CARTESIAN_POINT('Ctrl Pts',(5.21955989021131,3.86000452351564,3.88042395346285));
#17508=CARTESIAN_POINT('Ctrl Pts',(5.10528875315441,3.88084950155849,3.87457058988224));
#17509=CARTESIAN_POINT('Ctrl Pts',(4.9902991146134,3.89660294643127,3.86871722630163));
#17510=CARTESIAN_POINT('Ctrl Pts',(4.87532674138706,3.9123540259763,3.86286474158424));
#17511=CARTESIAN_POINT('Ctrl Pts',(4.7596364903955,3.92301503635694,3.85701225686685));
#17512=CARTESIAN_POINT('Ctrl Pts',(4.64371448735941,3.92854020817419,3.85115977214946));
#17513=CARTESIAN_POINT('Ctrl Pts',(4.52778185583898,3.93406588657518,3.84530675083815));
#17514=CARTESIAN_POINT('Ctrl Pts',(4.41161784273307,3.93445477066279,3.83945372952684));
#17515=CARTESIAN_POINT('Ctrl Pts',(4.29571057132544,3.92971318208583,3.83360070821553));
#17516=CARTESIAN_POINT('Ctrl Pts',(4.1797646426111,3.92497001209778,3.82774573480892));
#17517=CARTESIAN_POINT('Ctrl Pts',(4.06407603843998,3.91509298385434,3.8218907614023));
#17518=CARTESIAN_POINT('Ctrl Pts',(3.94912904284302,3.90014038979296,3.81603578799569));
#17519=CARTESIAN_POINT('Ctrl Pts',(3.83405176959896,3.88517084888785,3.81017417872917));
#17520=CARTESIAN_POINT('Ctrl Pts',(3.71971819247475,3.86511431384181,3.80431256946265));
#17521=CARTESIAN_POINT('Ctrl Pts',(3.60660376423607,3.84008045495111,3.79845096019613));
#17522=CARTESIAN_POINT('Ctrl Pts',(3.4934130621126,3.81502971554659,3.79258539840369));
#17523=CARTESIAN_POINT('Ctrl Pts',(3.38144354387121,3.78499507604044,3.78671983661125));
#17524=CARTESIAN_POINT('Ctrl Pts',(3.27115515598469,3.75013597611896,3.78085427481881));
#17525=CARTESIAN_POINT('Ctrl Pts',(3.16070549942915,3.71522590364493,3.77498013613662));
#17526=CARTESIAN_POINT('Ctrl Pts',(3.05194226577884,3.67547743292736,3.76910599745443));
#17527=CARTESIAN_POINT('Ctrl Pts',(2.9453051714037,3.63109798299575,3.76323185877225));
#17528=CARTESIAN_POINT('Ctrl Pts',(2.91833838813867,3.61987514337564,3.76174638483244));
#17529=CARTESIAN_POINT('Ctrl Pts',(2.89150744541438,3.60835637932971,3.76026091089263));
#17530=CARTESIAN_POINT('Ctrl Pts',(2.86481918651057,3.59654549993387,3.75877543695282));
#17531=CARTESIAN_POINT('Ctrl Pts',(2.7592915532681,3.54984428373059,3.75290174733985));
#17532=CARTESIAN_POINT('Ctrl Pts',(2.65564532388516,3.49841686024048,3.74702805772688));
#17533=CARTESIAN_POINT('Ctrl Pts',(2.55433373469968,3.44243664116246,3.74115436811391));
#17534=CARTESIAN_POINT('Ctrl Pts',(2.45315294827605,3.38652869779667,3.73528826198502));
#17535=CARTESIAN_POINT('Ctrl Pts',(2.35430116602657,3.32607984641507,3.72942215585613));
#17536=CARTESIAN_POINT('Ctrl Pts',(2.25821140394823,3.26131140408433,3.72355604972724));
#17537=CARTESIAN_POINT('Ctrl Pts',(2.16222003655062,3.19660928380567,3.7176959504156));
#17538=CARTESIAN_POINT('Ctrl Pts',(2.06898540420516,3.12759660024554,3.71183585110395));
#17539=CARTESIAN_POINT('Ctrl Pts',(1.97891507490576,3.05454006716678,3.7059757517923));
#17540=CARTESIAN_POINT('Ctrl Pts',(1.88559521845507,2.9788478249742,3.69990423378184));
#17541=CARTESIAN_POINT('Ctrl Pts',(1.79567269252324,2.89881465737932,3.69383271577137));
#17542=CARTESIAN_POINT('Ctrl Pts',(1.70956731060431,2.81478587556015,3.68776119776091));
#17543=CARTESIAN_POINT('Ctrl Pts',(1.62655575955935,2.73377631081778,3.68190783394074));
#17544=CARTESIAN_POINT('Ctrl Pts',(1.54709208861569,2.64905363449789,3.67605447012057));
#17545=CARTESIAN_POINT('Ctrl Pts',(1.47151736679682,2.56096702698902,3.67020110630041));
#17546=CARTESIAN_POINT('Ctrl Pts',(1.39595399227351,2.47289364539414,3.66434862134354));
#17547=CARTESIAN_POINT('Ctrl Pts',(1.32427867478326,2.38145765037765,3.65849613638667));
#17548=CARTESIAN_POINT('Ctrl Pts',(1.25679340810317,2.28704272520033,3.6526436514298));
#17549=CARTESIAN_POINT('Ctrl Pts',(1.18930195393846,2.19261914345359,3.64679062987935));
#17550=CARTESIAN_POINT('Ctrl Pts',(1.12600155453702,2.09521642472481,3.64093760832891));
#17551=CARTESIAN_POINT('Ctrl Pts',(1.06715151405735,1.99524816989482,3.63508458677846));
#17552=CARTESIAN_POINT('Ctrl Pts',(1.0082818459628,1.89524657373847,3.6292296131333));
#17553=CARTESIAN_POINT('Ctrl Pts',(0.953865697693562,1.79267809588955,3.62337463948814));
#17554=CARTESIAN_POINT('Ctrl Pts',(0.90411662065121,1.68798128493348,3.61751966584299));
#17555=CARTESIAN_POINT('Ctrl Pts',(0.854311159443263,1.58316581363882,3.61165805633998));
#17556=CARTESIAN_POINT('Ctrl Pts',(0.809183504447205,1.47621756801684,3.60579644683696));
#17557=CARTESIAN_POINT('Ctrl Pts',(0.768899246333945,1.36759552809771,3.59993483733395));
#17558=CARTESIAN_POINT('Ctrl Pts',(0.728587824258648,1.25890024356375,3.59406927530593));
#17559=CARTESIAN_POINT('Ctrl Pts',(0.693126428336241,1.14852930970523,3.5882037132779));
#17560=CARTESIAN_POINT('Ctrl Pts',(0.662630421520099,1.03695565695347,3.58233815124987));
#17561=CARTESIAN_POINT('Ctrl Pts',(0.632089822081742,0.925218856227082,
3.57646401233526));
#17562=CARTESIAN_POINT('Ctrl Pts',(0.606529192953198,0.812276228151098,
3.57058987342065));
#17563=CARTESIAN_POINT('Ctrl Pts',(0.58601261273831,0.698609713702123,3.56471573450604));
#17564=CARTESIAN_POINT('Ctrl Pts',(0.580824312153497,0.669865350011271,
3.56323026285108));
#17565=CARTESIAN_POINT('Ctrl Pts',(0.575958318644603,0.641074710892202,
3.56174479119612));
#17566=CARTESIAN_POINT('Ctrl Pts',(0.571415141220305,0.612245611706398,
3.56025931954116));
#17567=CARTESIAN_POINT('Ctrl Pts',(0.553451007686799,0.498252751851379,
3.55438563056146));
#17568=CARTESIAN_POINT('Ctrl Pts',(0.54047826906871,0.383278728455498,3.54851194158175));
#17569=CARTESIAN_POINT('Ctrl Pts',(0.532596909919817,0.267798407605622,
3.54263825260205));
#17570=CARTESIAN_POINT('Ctrl Pts',(0.524725726346264,0.152467182702637,
3.53677214710681));
#17571=CARTESIAN_POINT('Ctrl Pts',(0.521932877680621,0.0366313687176008,
3.53090604161158));
#17572=CARTESIAN_POINT('Ctrl Pts',(0.524267131582289,-0.0792251896119151,
3.52503993611635));
#17573=CARTESIAN_POINT('Ctrl Pts',(0.526598995237857,-0.194963112309522,
3.51917983743802));
#17574=CARTESIAN_POINT('Ctrl Pts',(0.53404751032907,-0.310721326493507,
3.51331973875968));
#17575=CARTESIAN_POINT('Ctrl Pts',(0.546609501711141,-0.426012761597005,
3.50745964008135));
#17576=CARTESIAN_POINT('Ctrl Pts',(0.559624702323609,-0.545463660036011,
3.50138812183336));
#17577=CARTESIAN_POINT('Ctrl Pts',(0.578129342378842,-0.664413012117803,
3.49531660358536));
#17578=CARTESIAN_POINT('Ctrl Pts',(0.602060839081441,-0.782320848646783,
3.48924508533737));
#17579=CARTESIAN_POINT('Ctrl Pts',(0.625132455800145,-0.89599215163021,
3.48339172214579));
#17580=CARTESIAN_POINT('Ctrl Pts',(0.65324756792712,-1.00869505654769,3.47753835895422));
#17581=CARTESIAN_POINT('Ctrl Pts',(0.686297653232049,-1.11995366649157,
3.47168499576264));
#17582=CARTESIAN_POINT('Ctrl Pts',(0.719342776190778,-1.23119557137296,
3.46583251143157));
#17583=CARTESIAN_POINT('Ctrl Pts',(0.757321281390588,-1.34099321653664,
3.4599800271005));
#17584=CARTESIAN_POINT('Ctrl Pts',(0.800074470503964,-1.44888483597551,
3.45412754276943));
#17585=CARTESIAN_POINT('Ctrl Pts',(0.842831579531272,-1.55678634767906,
3.44827452184131));
#17586=CARTESIAN_POINT('Ctrl Pts',(0.890364090523692,-1.66278110214558,
3.44242150091319));
#17587=CARTESIAN_POINT('Ctrl Pts',(0.942465022694893,-1.76642698716397,
3.43656847998508));
#17588=CARTESIAN_POINT('Ctrl Pts',(0.994583331562293,-1.8701074401446,3.43071350695817));
#17589=CARTESIAN_POINT('Ctrl Pts',(1.05127290588136,-1.97143709699979,3.42485853393127));
#17590=CARTESIAN_POINT('Ctrl Pts',(1.11228099811018,-2.06999876753311,3.41900356090437));
#17591=CARTESIAN_POINT('Ctrl Pts',(1.17335823525027,-2.16867214518124,3.41314195201039));
#17592=CARTESIAN_POINT('Ctrl Pts',(1.23876354184247,-2.26457092343504,3.40728034311642));
#17593=CARTESIAN_POINT('Ctrl Pts',(1.30820100167465,-2.35730713779801,3.40141873422244));
#17594=CARTESIAN_POINT('Ctrl Pts',(1.37768528373957,-2.45010588492963,3.39555317279886));
#17595=CARTESIAN_POINT('Ctrl Pts',(1.45120687163467,-2.53973750316626,3.38968761137527));
#17596=CARTESIAN_POINT('Ctrl Pts',(1.52843089759619,-2.62584867211522,3.38382204995169));
#17597=CARTESIAN_POINT('Ctrl Pts',(1.6057678441364,-2.71208575683858,3.37794791163015));
#17598=CARTESIAN_POINT('Ctrl Pts',(1.68681774542571,-2.79479182468583,3.37207377330861));
#17599=CARTESIAN_POINT('Ctrl Pts',(1.77121036033838,-2.87365176520671,3.36619963498708));
#17600=CARTESIAN_POINT('Ctrl Pts',(1.79255193144471,-2.89359420957591,3.36471415736789));
#17601=CARTESIAN_POINT('Ctrl Pts',(1.81410711560377,-2.91329090116227,3.3632286797487));
#17602=CARTESIAN_POINT('Ctrl Pts',(1.83586962136719,-2.93273717540429,3.36174320212951));
#17603=CARTESIAN_POINT('Ctrl Pts',(1.92192019416297,-3.00962919581136,3.35586951270257));
#17604=CARTESIAN_POINT('Ctrl Pts',(2.01150112941559,-3.08285880546186,3.34999582327562));
#17605=CARTESIAN_POINT('Ctrl Pts',(2.10426759595503,-3.15208455710113,3.34412213384868));
#17606=CARTESIAN_POINT('Ctrl Pts',(2.19691429221737,-3.22122093175143,3.33825602790999));
#17607=CARTESIAN_POINT('Ctrl Pts',(2.29273801262315,-3.28636348371889,3.33238992197131));
#17608=CARTESIAN_POINT('Ctrl Pts',(2.39135861600727,-3.34720893629611,3.32652381603263));
#17609=CARTESIAN_POINT('Ctrl Pts',(2.48987823309264,-3.40799208386971,3.32066371691511));
#17610=CARTESIAN_POINT('Ctrl Pts',(2.59118868695411,-3.46448666872914,3.31480361779758));
#17611=CARTESIAN_POINT('Ctrl Pts',(2.69487896704929,-3.51643131336056,3.30894351868005));
#17612=CARTESIAN_POINT('Ctrl Pts',(2.80231015513581,-3.57025000188531,3.3028720005983));
#17613=CARTESIAN_POINT('Ctrl Pts',(2.9122957669345,-3.61918397868074,3.29680048251654));
#17614=CARTESIAN_POINT('Ctrl Pts',(3.02434813546215,-3.66299311016559,3.29072896443478));
#17615=CARTESIAN_POINT('Ctrl Pts',(3.13237437344265,-3.70522814478098,3.2848756008172));
#17616=CARTESIAN_POINT('Ctrl Pts',(3.24232098597441,-3.74270011224495,3.27902223719963));
#17617=CARTESIAN_POINT('Ctrl Pts',(3.3537292421731,-3.7752422163678,3.27316887358205));
#17618=CARTESIAN_POINT('Ctrl Pts',(3.46512077073589,-3.80777943438538,3.26731638883054));
#17619=CARTESIAN_POINT('Ctrl Pts',(3.57797311012667,-3.83538814506056,3.26146390407902));
#17620=CARTESIAN_POINT('Ctrl Pts',(3.69181220282584,-3.85795137606662,3.25561141932751));
#17621=CARTESIAN_POINT('Ctrl Pts',(3.80566173297885,-3.88051667580563,3.24975839798493));
#17622=CARTESIAN_POINT('Ctrl Pts',(3.92049779100541,-3.89803549594168,3.24390537664236));
#17623=CARTESIAN_POINT('Ctrl Pts',(4.0358366602414,-3.91044209078609,3.23805235529978));
#17624=CARTESIAN_POINT('Ctrl Pts',(4.15121399715382,-3.92285282346262,3.2321973818648));
#17625=CARTESIAN_POINT('Ctrl Pts',(4.26709406817998,-3.93014789632348,3.22634240842981));
#17626=CARTESIAN_POINT('Ctrl Pts',(4.38298928822251,-3.93231353230478,3.22048743499483));
#17627=CARTESIAN_POINT('Ctrl Pts',(4.49901586051564,-3.93448162275452,3.2146258257043));
#17628=CARTESIAN_POINT('Ctrl Pts',(4.61505720279046,-3.93150866509864,3.20876421641378));
#17629=CARTESIAN_POINT('Ctrl Pts',(4.73062688638383,-3.92343300077555,3.20290260712326));
#17630=CARTESIAN_POINT('Ctrl Pts',(4.84627449940883,-3.91535189097653,3.19703704530932));
#17631=CARTESIAN_POINT('Ctrl Pts',(4.96144941101277,-3.90216127002637,3.19117148349538));
#17632=CARTESIAN_POINT('Ctrl Pts',(5.07567318823202,-3.88395099155711,3.18530592168144));
#17633=CARTESIAN_POINT('Ctrl Pts',(5.19006398855021,-3.8657140852069,3.17943178298154));
#17634=CARTESIAN_POINT('Ctrl Pts',(5.30350047565371,-3.84244295531576,3.17355764428164));
#17635=CARTESIAN_POINT('Ctrl Pts',(5.41551714845178,-3.81427789400406,3.16768350558174));
#17636=CARTESIAN_POINT('Ctrl Pts',(5.4438443332678,-3.80715541056296,3.16619803196044));
#17637=CARTESIAN_POINT('Ctrl Pts',(5.47208081224791,-3.79972020315359,3.16471255833915));
#17638=CARTESIAN_POINT('Ctrl Pts',(5.50021925512976,-3.7919750298027,3.16322708471785));
#17639=CARTESIAN_POINT('Ctrl Pts',(5.61148308992333,-3.76134939455417,3.15735328806591));
#17640=CARTESIAN_POINT('Ctrl Pts',(5.72158317202569,-3.72577155942982,3.15147949141397));
#17641=CARTESIAN_POINT('Ctrl Pts',(5.83004561867318,-3.68534619329475,3.14560569476203));
#17642=CARTESIAN_POINT('Ctrl Pts',(5.93835150618608,-3.64497917878768,3.13974037658857));
#17643=CARTESIAN_POINT('Ctrl Pts',(6.0450240781394,-3.59977869882972,3.13387505841512));
#17644=CARTESIAN_POINT('Ctrl Pts',(6.14960259571522,-3.5498997150263,3.12800974024167));
#17645=CARTESIAN_POINT('Ctrl Pts',(6.22734497102816,-3.51282029595477,3.12364953532253));
#17646=CARTESIAN_POINT('Ctrl Pts',(6.30393031702241,-3.47315647915035,3.11928933040339));
#17647=CARTESIAN_POINT('Ctrl Pts',(6.37917532067789,-3.43098962587739,3.11492912548425));
#17648=CARTESIAN_POINT('Ctrl Pts',(6.37998521093114,-3.43053564256519,2.93155396442585));
#17649=CARTESIAN_POINT('Ctrl Pts',(6.27882394601473,-3.48725719934643,2.93741792315029));
#17650=CARTESIAN_POINT('Ctrl Pts',(6.17524123718123,-3.53945011573742,2.94328188187473));
#17651=CARTESIAN_POINT('Ctrl Pts',(6.06968549222072,-3.58692373656496,2.94914584059916));
#17652=CARTESIAN_POINT('Ctrl Pts',(5.963964485873,-3.63447168358324,2.95501898012142));
#17653=CARTESIAN_POINT('Ctrl Pts',(5.85626465769322,-3.67728542650477,2.96089211964368));
#17654=CARTESIAN_POINT('Ctrl Pts',(5.74705199721677,-3.71522338513607,2.96676525916594));
#17655=CARTESIAN_POINT('Ctrl Pts',(5.67901496281762,-3.73885788122078,2.97042409316892));
#17656=CARTESIAN_POINT('Ctrl Pts',(5.61039108120681,-3.76060107992407,2.97408292717189));
#17657=CARTESIAN_POINT('Ctrl Pts',(5.54129499694641,-3.78042878345907,2.97774176117487));
#17658=CARTESIAN_POINT('Ctrl Pts',(5.43037195465575,-3.81225908500628,2.9836154514598));
#17659=CARTESIAN_POINT('Ctrl Pts',(5.31786206639191,-3.83925630756806,2.98948914174473));
#17660=CARTESIAN_POINT('Ctrl Pts',(5.20422432099473,-3.86126289428402,2.99536283202965));
#17661=CARTESIAN_POINT('Ctrl Pts',(5.0907332918741,-3.88324106857019,3.00122893886627));
#17662=CARTESIAN_POINT('Ctrl Pts',(4.97611770335411,-3.90024134288557,3.00709504570289));
#17663=CARTESIAN_POINT('Ctrl Pts',(4.86085174606983,-3.91215588653963,3.0129611525395));
#17664=CARTESIAN_POINT('Ctrl Pts',(4.74570381894656,-3.92405822992624,3.01882125259363));
#17665=CARTESIAN_POINT('Ctrl Pts',(4.62990725623192,-3.93088515895652,3.02468135264775));
#17666=CARTESIAN_POINT('Ctrl Pts',(4.51394583026764,-3.93257999615933,3.03054145270187));
#17667=CARTESIAN_POINT('Ctrl Pts',(4.39380080731622,-3.93433597883148,3.03661297044707));
#17668=CARTESIAN_POINT('Ctrl Pts',(4.27347924425192,-3.93058248633172,3.04268448819226));
#17669=CARTESIAN_POINT('Ctrl Pts',(4.15352470819547,-3.92131530123588,3.04875600593745));
#17670=CARTESIAN_POINT('Ctrl Pts',(4.03788020712725,-3.91238109139314,3.05460937058253));
#17671=CARTESIAN_POINT('Ctrl Pts',(3.92257725922248,-3.89832262491659,3.06046273522761));
#17672=CARTESIAN_POINT('Ctrl Pts',(3.80810148792087,-3.87918914614167,3.06631609987269));
#17673=CARTESIAN_POINT('Ctrl Pts',(3.69364290420577,-3.86005854009972,3.07216858568367));
#17674=CARTESIAN_POINT('Ctrl Pts',(3.5800116575329,-3.83585450493382,3.07802107149465));
#17675=CARTESIAN_POINT('Ctrl Pts',(3.4676855107552,-3.80667781685595,3.08387355730563));
#17676=CARTESIAN_POINT('Ctrl Pts',(3.35534906464776,-3.77749845352979,3.08972657973861));
#17677=CARTESIAN_POINT('Ctrl Pts',(3.24431835621806,-3.74334563478088,3.09557960217159));
#17678=CARTESIAN_POINT('Ctrl Pts',(3.13505757406079,-3.70437046779628,3.10143262460457));
#17679=CARTESIAN_POINT('Ctrl Pts',(3.02576035083068,-3.66538230166533,3.10728759915991));
#17680=CARTESIAN_POINT('Ctrl Pts',(2.91823461660142,-3.62156872786435,3.11314257371526));
#17681=CARTESIAN_POINT('Ctrl Pts',(2.81292544837541,-3.57312933501777,3.11899754827061));
#17682=CARTESIAN_POINT('Ctrl Pts',(2.7074969251424,-3.52463504206924,3.12485915872044));
#17683=CARTESIAN_POINT('Ctrl Pts',(2.60429035767502,-3.4715046385104,3.13072076917027));
#17684=CARTESIAN_POINT('Ctrl Pts',(2.50372712116051,-3.41398414463113,3.13658237962011));
#17685=CARTESIAN_POINT('Ctrl Pts',(2.40309607376402,-3.35642486405846,3.1424479426175));
#17686=CARTESIAN_POINT('Ctrl Pts',(2.30511225485916,-3.29446981882981,3.14831350561488));
#17687=CARTESIAN_POINT('Ctrl Pts',(2.21016744244267,-3.22840794127989,3.15417906861227));
#17688=CARTESIAN_POINT('Ctrl Pts',(2.11508379709062,-3.16224946483051,3.16005320852196));
#17689=CARTESIAN_POINT('Ctrl Pts',(2.02304835400144,-3.09197242093831,3.16592734843165));
#17690=CARTESIAN_POINT('Ctrl Pts',(1.93441931562576,-3.01790554089627,3.17180148834134));
#17691=CARTESIAN_POINT('Ctrl Pts',(1.91200663972036,-2.99917537064811,3.1732869517564));
#17692=CARTESIAN_POINT('Ctrl Pts',(1.88981161247733,-2.98020302289591,3.17477241517146));
#17693=CARTESIAN_POINT('Ctrl Pts',(1.86783963578063,-2.9609941683127,3.17625787858652));
#17694=CARTESIAN_POINT('Ctrl Pts',(1.78096001147519,-2.88504023423732,3.18213156511009));
#17695=CARTESIAN_POINT('Ctrl Pts',(1.69728140969937,-2.80513280674074,3.18800525163367));
#17696=CARTESIAN_POINT('Ctrl Pts',(1.61718504894668,-2.72157216368103,3.19387893815724));
#17697=CARTESIAN_POINT('Ctrl Pts',(1.53719210076511,-2.63811940593424,3.19974504115243));
#17698=CARTESIAN_POINT('Ctrl Pts',(1.46077247920051,-2.55102310807291,3.20561114414763));
#17699=CARTESIAN_POINT('Ctrl Pts',(1.38827385857003,-2.46062327923412,3.21147724714282));
#17700=CARTESIAN_POINT('Ctrl Pts',(1.31584947613255,-2.37031601932813,3.21733734328046));
#17701=CARTESIAN_POINT('Ctrl Pts',(1.24733836523732,-2.27671227749517,3.22319743941811));
#17702=CARTESIAN_POINT('Ctrl Pts',(1.18305041014706,-2.18018784516647,3.22905753555575));
#17703=CARTESIAN_POINT('Ctrl Pts',(1.11644304679787,-2.08018096320598,3.23512905474085));
#17704=CARTESIAN_POINT('Ctrl Pts',(1.05436963498423,-1.97703898989284,3.24120057392596));
#17705=CARTESIAN_POINT('Ctrl Pts',(0.997128392570591,-1.87121640301161,
3.24727209311106));
#17706=CARTESIAN_POINT('Ctrl Pts',(0.94194391223764,-1.76919617741396,3.25312545367651));
#17707=CARTESIAN_POINT('Ctrl Pts',(0.891250537100192,-1.66468505426169,
3.25897881424196));
#17708=CARTESIAN_POINT('Ctrl Pts',(0.845270148035759,-1.55811780184352,
3.2648321748074));
#17709=CARTESIAN_POINT('Ctrl Pts',(0.799296662970429,-1.45156655059955,
3.2706846564852));
#17710=CARTESIAN_POINT('Ctrl Pts',(0.758034920515486,-1.34296016320006,
3.276537138163));
#17711=CARTESIAN_POINT('Ctrl Pts',(0.721659237634693,-1.23275473859599,
3.2823896198408));
#17712=CARTESIAN_POINT('Ctrl Pts',(0.685280219724785,-1.12253921003591,
3.28824263809126));
#17713=CARTESIAN_POINT('Ctrl Pts',(0.653788281410874,-1.01072474518332,
3.29409565634172));
#17714=CARTESIAN_POINT('Ctrl Pts',(0.627308087424881,-0.897783321382907,
3.29994867459217));
#17715=CARTESIAN_POINT('Ctrl Pts',(0.600819061861613,-0.784804229772644,
3.30580364491983));
#17716=CARTESIAN_POINT('Ctrl Pts',(0.57934519858409,-0.670697833855755,
3.31165861524749));
#17717=CARTESIAN_POINT('Ctrl Pts',(0.562960062424372,-0.55594633364676,
3.31751358557514));
#17718=CARTESIAN_POINT('Ctrl Pts',(0.546556355840786,-0.441064777515275,
3.32337519175127));
#17719=CARTESIAN_POINT('Ctrl Pts',(0.535252946213132,-0.325537067002251,
3.3292367979274));
#17720=CARTESIAN_POINT('Ctrl Pts',(0.529071532504052,-0.209850656381681,
3.33509840410352));
#17721=CARTESIAN_POINT('Ctrl Pts',(0.522885950631409,-0.0940862377351004,
3.34096396279512));
#17722=CARTESIAN_POINT('Ctrl Pts',(0.521829245699624,0.0218366819985692,
3.34682952148671));
#17723=CARTESIAN_POINT('Ctrl Pts',(0.525871012423307,0.137432256241249,
3.3526950801783));
#17724=CARTESIAN_POINT('Ctrl Pts',(0.52991868921005,0.253196859816847,3.3585692157681));
#17725=CARTESIAN_POINT('Ctrl Pts',(0.539079683852553,0.368632752348954,
3.36444335135789));
#17726=CARTESIAN_POINT('Ctrl Pts',(0.553271946061515,0.483260725638233,
3.37031748694768));
#17727=CARTESIAN_POINT('Ctrl Pts',(0.556861010019064,0.512248854620215,
3.37180298996452));
#17728=CARTESIAN_POINT('Ctrl Pts',(0.560771584283068,0.541185375824925,
3.37328849298135));
#17729=CARTESIAN_POINT('Ctrl Pts',(0.56500183200524,0.570062675264016,3.37477399599818));
#17730=CARTESIAN_POINT('Ctrl Pts',(0.581728265213222,0.684243747394415,
3.380647686766));
#17731=CARTESIAN_POINT('Ctrl Pts',(0.603512162472252,0.797878197613152,
3.38652137753381));
#17732=CARTESIAN_POINT('Ctrl Pts',(0.630307859347065,0.91048290096033,3.39239506830163));
#17733=CARTESIAN_POINT('Ctrl Pts',(0.657068960535059,1.02294222137272,3.39826117559934));
#17734=CARTESIAN_POINT('Ctrl Pts',(0.68882889848895,1.13437404059641,3.40412728289704));
#17735=CARTESIAN_POINT('Ctrl Pts',(0.725490437660223,1.24430188248872,3.40999339019475));
#17736=CARTESIAN_POINT('Ctrl Pts',(0.762114435972227,1.3541171599406,3.41585349068769));
#17737=CARTESIAN_POINT('Ctrl Pts',(0.803629922034241,1.46243113375427,3.42171359118062));
#17738=CARTESIAN_POINT('Ctrl Pts',(0.849889105824581,1.56877968522046,3.42757369167355));
#17739=CARTESIAN_POINT('Ctrl Pts',(0.89781719982298,1.678965013919,3.4336452092459));
#17740=CARTESIAN_POINT('Ctrl Pts',(0.950837629724561,1.78703998878236,3.43971672681824));
#17741=CARTESIAN_POINT('Ctrl Pts',(1.00873016092378,1.89250763937686,3.44578824439059));
#17742=CARTESIAN_POINT('Ctrl Pts',(1.0645425856255,1.99418578654608,3.45164160941561));
#17743=CARTESIAN_POINT('Ctrl Pts',(1.12488280723949,2.09344035657259,3.45749497444064));
#17744=CARTESIAN_POINT('Ctrl Pts',(1.18950576965194,2.18984920885697,3.46334833946566));
#17745=CARTESIAN_POINT('Ctrl Pts',(1.25411902921493,2.28624358578236,3.46920082563404));
#17746=CARTESIAN_POINT('Ctrl Pts',(1.32301352100993,2.3797927514542,3.47505331180243));
#17747=CARTESIAN_POINT('Ctrl Pts',(1.39590047977422,2.47010297008576,3.48090579797081));
#17748=CARTESIAN_POINT('Ctrl Pts',(1.46879412135073,2.5604214690221,3.48675882073815));
#17749=CARTESIAN_POINT('Ctrl Pts',(1.5456806980991,2.64750010905138,3.49261184350549));
#17750=CARTESIAN_POINT('Ctrl Pts',(1.6262311850929,2.73097826974585,3.49846486627283));
#17751=CARTESIAN_POINT('Ctrl Pts',(1.70680853726662,2.81448427205731,3.50431984113898));
#17752=CARTESIAN_POINT('Ctrl Pts',(1.79105194282877,2.89438711009113,3.51017481600513));
#17753=CARTESIAN_POINT('Ctrl Pts',(1.87859608494008,2.97036356127767,3.51602979087128));
#17754=CARTESIAN_POINT('Ctrl Pts',(1.96623944702887,3.04642612195816,3.52189140159519));
#17755=CARTESIAN_POINT('Ctrl Pts',(2.05719070019636,3.11855314280891,3.52775301231909));
#17756=CARTESIAN_POINT('Ctrl Pts',(2.15105199544097,3.18646213618416,3.533614623043));
#17757=CARTESIAN_POINT('Ctrl Pts',(2.24497658203479,3.25441692108407,3.53948018629335));
#17758=CARTESIAN_POINT('Ctrl Pts',(2.34181477374659,3.31814778842023,3.54534574954369));
#17759=CARTESIAN_POINT('Ctrl Pts',(2.4411418263325,3.37741690570594,3.55121131279404));
#17760=CARTESIAN_POINT('Ctrl Pts',(2.54061411921397,3.43677268884842,3.55708545292368));
#17761=CARTESIAN_POINT('Ctrl Pts',(2.64258217373584,3.49165350630103,3.56295959305331));
#17762=CARTESIAN_POINT('Ctrl Pts',(2.74659882669214,3.5418685220083,3.56883373318295));
#17763=CARTESIAN_POINT('Ctrl Pts',(2.77290269104623,3.55456695946195,3.57031919325857));
#17764=CARTESIAN_POINT('Ctrl Pts',(2.79933747508719,3.56696726943899,3.5718046533342));
#17765=CARTESIAN_POINT('Ctrl Pts',(2.82589578559808,3.57906686806516,3.57329011340983));
#17766=CARTESIAN_POINT('Ctrl Pts',(2.93091056805809,3.62691014925051,3.57916380280099));
#17767=CARTESIAN_POINT('Ctrl Pts',(3.03820771881232,3.6702072774082,3.58503749219215));
#17768=CARTESIAN_POINT('Ctrl Pts',(3.14735650930925,3.70873471801559,3.59091118158331));
#17769=CARTESIAN_POINT('Ctrl Pts',(3.25636437852917,3.74721241610082,3.59677728749319));
#17770=CARTESIAN_POINT('Ctrl Pts',(3.36721874726458,3.78093253684036,3.60264339340306));
#17771=CARTESIAN_POINT('Ctrl Pts',(3.47946651680597,3.80971848569966,3.60850949931294));
#17772=CARTESIAN_POINT('Ctrl Pts',(3.59159934612842,3.83847495813125,3.61436959840861));
#17773=CARTESIAN_POINT('Ctrl Pts',(3.70512234036981,3.86230720655599,3.62022969750427));
#17774=CARTESIAN_POINT('Ctrl Pts',(3.81956537878968,3.88108781683533,3.62608979659993));
#17775=CARTESIAN_POINT('Ctrl Pts',(3.93813726076493,3.90054598865784,3.6321613146925));
#17776=CARTESIAN_POINT('Ctrl Pts',(4.05769640058846,3.91458098686229,3.63823283278506));
#17777=CARTESIAN_POINT('Ctrl Pts',(4.17770579854166,3.92310846374316,3.64430435087763));
#17778=CARTESIAN_POINT('Ctrl Pts',(4.29340316327078,3.93132954158983,3.65015771449077));
#17779=CARTESIAN_POINT('Ctrl Pts',(4.40951853927424,3.93443203428057,3.65601107810392));
#17780=CARTESIAN_POINT('Ctrl Pts',(4.5255643514418,3.93239301788205,3.66186444171707));
#17781=CARTESIAN_POINT('Ctrl Pts',(4.64159273978531,3.93035430763386,3.6677169264706));
#17782=CARTESIAN_POINT('Ctrl Pts',(4.75755117209072,3.92317563053372,3.67356941122413));
#17783=CARTESIAN_POINT('Ctrl Pts',(4.87295224688062,3.91088619030828,3.67942189597767));
#17784=CARTESIAN_POINT('Ctrl Pts',(4.98836390246322,3.8985956232994,3.6852749173287));
#17785=CARTESIAN_POINT('Ctrl Pts',(5.10321768809874,3.88119340540197,3.69112793867973));
#17786=CARTESIAN_POINT('Ctrl Pts',(5.2170322042534,3.85876052300569,3.69698096003076));
#17787=CARTESIAN_POINT('Ctrl Pts',(5.33088467980967,3.8363201587976,3.70283593348066));
#17788=CARTESIAN_POINT('Ctrl Pts',(5.443696791525,3.80884587365829,3.70869090693055));
#17789=CARTESIAN_POINT('Ctrl Pts',(5.55499889138541,3.77646942409185,3.71454588038045));
#17790=CARTESIAN_POINT('Ctrl Pts',(5.66642713796823,3.7440562799527,3.72040748969536));
#17791=CARTESIAN_POINT('Ctrl Pts',(5.77634155990948,3.70672999745012,3.72626909901028));
#17792=CARTESIAN_POINT('Ctrl Pts',(5.88428910307584,3.66467175290961,3.73213070832519));
#17793=CARTESIAN_POINT('Ctrl Pts',(5.99230943611389,3.62258514816623,3.73799627016906));
#17794=CARTESIAN_POINT('Ctrl Pts',(6.0983598724473,3.57576039425805,3.74386183201292));
#17795=CARTESIAN_POINT('Ctrl Pts',(6.20201030185977,3.52442547577877,3.74972739385679));
#17796=CARTESIAN_POINT('Ctrl Pts',(6.30581229368861,3.47301549302495,3.75560153259447));
#17797=CARTESIAN_POINT('Ctrl Pts',(6.40720691435273,3.41708238258832,3.76147567133214));
#17798=CARTESIAN_POINT('Ctrl Pts',(6.50579139157662,3.35689844510279,3.76734981006982));
#17799=CARTESIAN_POINT('Ctrl Pts',(6.5307217929916,3.341678911942,3.76883528365371));
#17800=CARTESIAN_POINT('Ctrl Pts',(6.55547264511292,3.32618774324588,3.7703207572376));
#17801=CARTESIAN_POINT('Ctrl Pts',(6.58003776858831,3.31042975098398,3.77180623082149));
#17802=CARTESIAN_POINT('Ctrl Pts',(6.59622194482155,3.30004795403904,3.77278490150863));
#17803=CARTESIAN_POINT('Ctrl Pts',(6.61233446581222,3.28954459824748,3.77376357219578));
#17804=CARTESIAN_POINT('Ctrl Pts',(6.62837333988161,3.27892070654281,3.77474224288293));
#17805=CARTESIAN_POINT('Origin',(4.45646910621825,0.,0.));
#17806=CARTESIAN_POINT('Ctrl Pts',(6.37692902980906,3.42691262734843,2.69315322924027));
#17807=CARTESIAN_POINT('Ctrl Pts',(5.65097596260216,3.82742863485321,2.6513283969878));
#17808=CARTESIAN_POINT('Ctrl Pts',(3.45307807194487,4.29849211691197,2.54333152559812));
#17809=CARTESIAN_POINT('Ctrl Pts',(0.275078285875853,2.03215589035587,2.36916261507124));
#17810=CARTESIAN_POINT('Ctrl Pts',(0.482062492976864,-2.41200736048335,
2.17064649765957));
#17811=CARTESIAN_POINT('Ctrl Pts',(3.73790413319295,-4.3039644467813,2.00262135099753));
#17812=CARTESIAN_POINT('Ctrl Pts',(5.75771551529821,-3.77032809480342,1.90076824347269));
#17813=CARTESIAN_POINT('Ctrl Pts',(6.37611478183885,-3.42549916664848,1.86508717508508));
#17814=CARTESIAN_POINT('Ctrl Pts',(6.37607929534711,-3.42544344211231,1.6817486560154));
#17815=CARTESIAN_POINT('Ctrl Pts',(5.77024621859546,-3.76371820199713,1.71671412291191));
#17816=CARTESIAN_POINT('Ctrl Pts',(3.77067693841887,-4.30358028239296,1.81785162894564));
#17817=CARTESIAN_POINT('Ctrl Pts',(0.508467943610061,-2.45499576926686,
1.98516117411659));
#17818=CARTESIAN_POINT('Ctrl Pts',(0.253275128055896,1.9866819812542,2.18367729152824));
#17819=CARTESIAN_POINT('Ctrl Pts',(3.41948173903076,4.29681960175239,2.35856292813192));
#17820=CARTESIAN_POINT('Ctrl Pts',(5.63863432548647,3.83414340656477,2.46727652559838));
#17821=CARTESIAN_POINT('Ctrl Pts',(6.3770723437125,3.42716806216871,2.50981808392762));
#17822=CARTESIAN_POINT('Origin',(4.45646910621825,0.,0.));
#17823=CARTESIAN_POINT('Ctrl Pts',(6.37730370004212,3.42771650614551,1.44343144191858));
#17824=CARTESIAN_POINT('Ctrl Pts',(5.99388198929395,3.64655365578385,1.42114830395004));
#17825=CARTESIAN_POINT('Ctrl Pts',(4.33567752240144,4.26502542083611,1.33269312684427));
#17826=CARTESIAN_POINT('Ctrl Pts',(1.04993737828694,3.16381092564229,1.17806591060129));
#17827=CARTESIAN_POINT('Ctrl Pts',(-0.0487366697561428,-1.1475464932117,
0.979549793189644));
#17828=CARTESIAN_POINT('Ctrl Pts',(2.81174385334673,-4.22821688899241,0.791955857486359));
#17829=CARTESIAN_POINT('Ctrl Pts',(5.42295440143473,-3.95757168087368,0.670533960920302));
#17830=CARTESIAN_POINT('Ctrl Pts',(6.37917532067772,-3.43420595741613,0.615284103491462));
#17831=CARTESIAN_POINT('Ctrl Pts',(6.38006015424921,-3.4304936204481,0.431770922268101));
#17832=CARTESIAN_POINT('Ctrl Pts',(6.27895466275247,-3.48718680803797,0.437639464367201));
#17833=CARTESIAN_POINT('Ctrl Pts',(6.17523350067364,-3.53946657277982,0.443508006466302));
#17834=CARTESIAN_POINT('Ctrl Pts',(6.06931927524152,-3.58708841991407,0.449376548565403));
#17835=CARTESIAN_POINT('Ctrl Pts',(5.95939934748487,-3.63651133714051,0.455467040384969));
#17836=CARTESIAN_POINT('Ctrl Pts',(5.8471175673446,-3.68091679339533,0.461557532204536));
#17837=CARTESIAN_POINT('Ctrl Pts',(5.73297491792037,-3.72008358947628,0.467648024024102));
#17838=CARTESIAN_POINT('Ctrl Pts',(5.62312163480198,-3.75777853663603,0.473509641268489));
#17839=CARTESIAN_POINT('Ctrl Pts',(5.51154524410124,-3.79062130430239,0.479371258512876));
#17840=CARTESIAN_POINT('Ctrl Pts',(5.39871211440115,-3.8184639730565,0.485232875757263));
#17841=CARTESIAN_POINT('Ctrl Pts',(5.28589743439592,-3.84630208916952,0.491093534550441));
#17842=CARTESIAN_POINT('Ctrl Pts',(5.17182682369662,-3.86914163356721,0.49695419334362));
#17843=CARTESIAN_POINT('Ctrl Pts',(5.05697990829913,-3.88688509948315,0.502814852136798));
#17844=CARTESIAN_POINT('Ctrl Pts',(4.94212422200554,-3.90462992047333,0.508675958510386));
#17845=CARTESIAN_POINT('Ctrl Pts',(4.82649252014119,-3.91727782647895,0.514537064883973));
#17846=CARTESIAN_POINT('Ctrl Pts',(4.71057198396183,-3.92478288922106,0.52039817125756));
#17847=CARTESIAN_POINT('Ctrl Pts',(4.59461478773703,-3.93229032545065,0.526261131214931));
#17848=CARTESIAN_POINT('Ctrl Pts',(4.47836898628299,-3.93465165759226,0.532124091172302));
#17849=CARTESIAN_POINT('Ctrl Pts',(4.3623235183463,-3.93187304071282,0.537987051129672));
#17850=CARTESIAN_POINT('Ctrl Pts',(4.24614968162425,-3.92909135014441,0.543856496657412));
#17851=CARTESIAN_POINT('Ctrl Pts',(4.13017703269396,-3.92115837136354,0.549725942185151));
#17852=CARTESIAN_POINT('Ctrl Pts',(4.01489124968035,-3.90813229006074,0.555595387712891));
#17853=CARTESIAN_POINT('Ctrl Pts',(3.8995298288338,-3.89509766247811,0.561468684124309));
#17854=CARTESIAN_POINT('Ctrl Pts',(3.78485657719902,-3.87696334197444,0.567341980535728));
#17855=CARTESIAN_POINT('Ctrl Pts',(3.67134713414353,-3.85383866929656,0.573215276947146));
#17856=CARTESIAN_POINT('Ctrl Pts',(3.55767425096559,-3.83068069983533,0.579097030208134));
#17857=CARTESIAN_POINT('Ctrl Pts',(3.44516891911741,-3.80251813613975,0.584978783469122));
#17858=CARTESIAN_POINT('Ctrl Pts',(3.33429186531407,-3.76951021221547,0.59086053673011));
#17859=CARTESIAN_POINT('Ctrl Pts',(3.30483516258775,-3.76074099830421,0.592423141898406));
#17860=CARTESIAN_POINT('Ctrl Pts',(3.27549327419337,-3.75163005928345,0.593985747066702));
#17861=CARTESIAN_POINT('Ctrl Pts',(3.24627458536827,-3.74218094454353,0.595548352234998));
#17862=CARTESIAN_POINT('Ctrl Pts',(3.13625460306234,-3.7066012700853,0.601432182067205));
#17863=CARTESIAN_POINT('Ctrl Pts',(3.02762898411309,-3.66610869725488,0.607316011899411));
#17864=CARTESIAN_POINT('Ctrl Pts',(2.9208675596608,-3.62083096681002,0.613199841731618));
#17865=CARTESIAN_POINT('Ctrl Pts',(2.81424037276223,-3.57561016677616,0.619076273471047));
#17866=CARTESIAN_POINT('Ctrl Pts',(2.7094730940747,-3.52561633477818,0.624952705210476));
#17867=CARTESIAN_POINT('Ctrl Pts',(2.60702018232466,-3.47102689098037,0.630829136949905));
#17868=CARTESIAN_POINT('Ctrl Pts',(2.50466900473832,-3.41649165365962,0.636699733483107));
#17869=CARTESIAN_POINT('Ctrl Pts',(2.40462798357623,-3.35737007477141,0.64257033001631));
#17870=CARTESIAN_POINT('Ctrl Pts',(2.30733077539245,-3.29388728328328,0.648440926549512));
#17871=CARTESIAN_POINT('Ctrl Pts',(2.20676771144991,-3.22827364298628,0.65450857417856));
#17872=CARTESIAN_POINT('Ctrl Pts',(2.10913631219929,-3.15800103645049,0.660576221807607));
#17873=CARTESIAN_POINT('Ctrl Pts',(2.0148871533803,-3.08336935309022,0.666643869436655));
#17874=CARTESIAN_POINT('Ctrl Pts',(1.92379782053678,-3.01123979425424,0.672508091265106));
#17875=CARTESIAN_POINT('Ctrl Pts',(1.83586791850928,-2.93503904215122,0.678372313093558));
#17876=CARTESIAN_POINT('Ctrl Pts',(1.75147329799903,-2.85508085306116,0.68423653492201));
#17877=CARTESIAN_POINT('Ctrl Pts',(1.66708967288883,-2.77513308136821,0.690099992727061));
#17878=CARTESIAN_POINT('Ctrl Pts',(1.58624071202294,-2.69142912907891,0.695963450532113));
#17879=CARTESIAN_POINT('Ctrl Pts',(1.50926687912181,-2.60432103101707,0.701826908337165));
#17880=CARTESIAN_POINT('Ctrl Pts',(1.43228464761449,-2.5172034286005,0.707691005903433));
#17881=CARTESIAN_POINT('Ctrl Pts',(1.35917865723167,-2.42668125024711,0.713555103469702));
#17882=CARTESIAN_POINT('Ctrl Pts',(1.29024994083508,-2.33314062944356,0.719419201035971));
#17883=CARTESIAN_POINT('Ctrl Pts',(1.22129720254228,-2.23956740940994,0.725285342260536));
#17884=CARTESIAN_POINT('Ctrl Pts',(1.15652487732791,-2.14297398598627,0.731151483485101));
#17885=CARTESIAN_POINT('Ctrl Pts',(1.09619102868573,-2.04377597638643,0.737017624709665));
#17886=CARTESIAN_POINT('Ctrl Pts',(1.03578811269634,-1.94446440957907,0.742890481216312));
#17887=CARTESIAN_POINT('Ctrl Pts',(0.979834028691006,-1.84254265710323,
0.748763337722959));
#17888=CARTESIAN_POINT('Ctrl Pts',(0.92854122569731,-1.73845157247564,0.754636194229606));
#17889=CARTESIAN_POINT('Ctrl Pts',(0.877213378961228,-1.63428937180561,
0.760513063128995));
#17890=CARTESIAN_POINT('Ctrl Pts',(0.830553320027273,-1.52795526336591,
0.766389932028385));
#17891=CARTESIAN_POINT('Ctrl Pts',(0.788724972113124,-1.41990914031055,
0.772266800927774));
#17892=CARTESIAN_POINT('Ctrl Pts',(0.746835572580654,-1.31170531581597,
0.778152247559129));
#17893=CARTESIAN_POINT('Ctrl Pts',(0.7097920897946,-1.20178487800983,0.784037694190484));
#17894=CARTESIAN_POINT('Ctrl Pts',(0.677708366468663,-1.09062196554404,
0.78992314082184));
#17895=CARTESIAN_POINT('Ctrl Pts',(0.670183066830447,-1.06454848845837,
0.791303583763444));
#17896=CARTESIAN_POINT('Ctrl Pts',(0.662930403658656,-1.03840669499931,
0.792684026705048));
#17897=CARTESIAN_POINT('Ctrl Pts',(0.655951435417046,-1.01220276324844,
0.794064469646653));
#17898=CARTESIAN_POINT('Ctrl Pts',(0.626295337403964,-0.900853013338637,
0.799930458681192));
#17899=CARTESIAN_POINT('Ctrl Pts',(0.601486334207142,-0.788008674215623,
0.805796447715731));
#17900=CARTESIAN_POINT('Ctrl Pts',(0.581673949443585,-0.674130175140967,
0.81166243675027));
#17901=CARTESIAN_POINT('Ctrl Pts',(0.561887502550487,-0.560400762902271,
0.817520746181091));
#17902=CARTESIAN_POINT('Ctrl Pts',(0.547084736594483,-0.445640287361216,
0.823379055611912));
#17903=CARTESIAN_POINT('Ctrl Pts',(0.537365211052586,-0.330323566972319,
0.829237365042733));
#17904=CARTESIAN_POINT('Ctrl Pts',(0.527655794716167,-0.21512678663773,
0.835089581289938));
#17905=CARTESIAN_POINT('Ctrl Pts',(0.523019137769456,-0.0993753225297563,
0.840941797537144));
#17906=CARTESIAN_POINT('Ctrl Pts',(0.523503496516046,0.0164472763632276,
0.846794013784349));
#17907=CARTESIAN_POINT('Ctrl Pts',(0.524006247659929,0.136667969167399,
0.852868454337431));
#17908=CARTESIAN_POINT('Ctrl Pts',(0.530026726470097,0.256964858772304,
0.858942894890512));
#17909=CARTESIAN_POINT('Ctrl Pts',(0.541559615467651,0.376792620987839,
0.865017335443594));
#17910=CARTESIAN_POINT('Ctrl Pts',(0.552657486269063,0.492100504708243,
0.870862649350912));
#17911=CARTESIAN_POINT('Ctrl Pts',(0.568859397830202,0.606973561036211,
0.87670796325823));
#17912=CARTESIAN_POINT('Ctrl Pts',(0.590107572941103,0.720928216950054,
0.882553277165548));
#17913=CARTESIAN_POINT('Ctrl Pts',(0.611352377896869,0.834864798612026,
0.888397663952556));
#17914=CARTESIAN_POINT('Ctrl Pts',(0.637641779113809,0.947882862223743,
0.894242050739565));
#17915=CARTESIAN_POINT('Ctrl Pts',(0.668866615925173,1.05950760994232,0.900086437526574));
#17916=CARTESIAN_POINT('Ctrl Pts',(0.700094106349606,1.17114184398394,0.905931320993237));
#17917=CARTESIAN_POINT('Ctrl Pts',(0.736257754424545,1.28138212767146,0.911776204459899));
#17918=CARTESIAN_POINT('Ctrl Pts',(0.777198322519407,1.38976814621004,0.917621087926562));
#17919=CARTESIAN_POINT('Ctrl Pts',(0.818152342803302,1.49818977806026,0.923467891896064));
#17920=CARTESIAN_POINT('Ctrl Pts',(0.863886257564295,1.60475554589305,0.929314695865567));
#17921=CARTESIAN_POINT('Ctrl Pts',(0.914192707903539,1.70902513672051,0.935161499835069));
#17922=CARTESIAN_POINT('Ctrl Pts',(0.964556201126772,1.81341295966598,0.941014933542075));
#17923=CARTESIAN_POINT('Ctrl Pts',(1.01950239820608,1.91549903551455,0.946868367249082));
#17924=CARTESIAN_POINT('Ctrl Pts',(1.0787779588869,2.01486761680251,0.952721800956089));
#17925=CARTESIAN_POINT('Ctrl Pts',(1.13809340619642,2.11430306338302,0.958579173448898));
#17926=CARTESIAN_POINT('Ctrl Pts',(1.20174379031527,2.2110170292401,0.964436545941708));
#17927=CARTESIAN_POINT('Ctrl Pts',(1.26943343021391,2.30462417757766,0.970293918434517));
#17928=CARTESIAN_POINT('Ctrl Pts',(1.33722268194242,2.39836907785702,0.976159910615556));
#17929=CARTESIAN_POINT('Ctrl Pts',(1.40906279582494,2.48899771280837,0.982025902796595));
#17930=CARTESIAN_POINT('Ctrl Pts',(1.48461894191781,2.57615907912292,0.987891894977633));
#17931=CARTESIAN_POINT('Ctrl Pts',(1.50474963722611,2.59938179492657,0.989454792337859));
#17932=CARTESIAN_POINT('Ctrl Pts',(1.52514392806353,2.62235859143156,0.991017689698084));
#17933=CARTESIAN_POINT('Ctrl Pts',(1.54579507190206,2.64508330038158,0.99258058705831));
#17934=CARTESIAN_POINT('Ctrl Pts',(1.62342757052777,2.73051081713931,0.998455885207339));
#17935=CARTESIAN_POINT('Ctrl Pts',(1.70495298987006,2.81265945630749,1.00433118335637));
#17936=CARTESIAN_POINT('Ctrl Pts',(1.79006349645624,2.89115377042275,1.0102064815054));
#17937=CARTESIAN_POINT('Ctrl Pts',(1.87506423519424,2.96954684965761,1.01607420222526));
#17938=CARTESIAN_POINT('Ctrl Pts',(1.96364056522896,3.04429469924159,1.02194192294512));
#17939=CARTESIAN_POINT('Ctrl Pts',(2.05544558753515,3.11505618933762,1.02780964366498));
#17940=CARTESIAN_POINT('Ctrl Pts',(2.14715669181916,3.18574528928516,1.03367136161167));
#17941=CARTESIAN_POINT('Ctrl Pts',(2.24208959325428,3.25245589098474,1.03953307955836));
#17942=CARTESIAN_POINT('Ctrl Pts',(2.33986235636494,3.31488534741028,1.04539479750505));
#17943=CARTESIAN_POINT('Ctrl Pts',(2.44112446476054,3.3795428060165,1.05146571029525));
#17944=CARTESIAN_POINT('Ctrl Pts',(2.54543259012771,3.43960753068541,1.05753662308546));
#17945=CARTESIAN_POINT('Ctrl Pts',(2.65232685961407,3.49479037340125,1.06360753587566));
#17946=CARTESIAN_POINT('Ctrl Pts',(2.75541910430907,3.54801046790737,1.06946251790507));
#17947=CARTESIAN_POINT('Ctrl Pts',(2.86091625959808,3.59668983951194,1.07531749993449));
#17948=CARTESIAN_POINT('Ctrl Pts',(2.96837914617397,3.64061495778054,1.0811724819639));
#17949=CARTESIAN_POINT('Ctrl Pts',(3.07582584722618,3.68453346026704,1.08702658214514));
#17950=CARTESIAN_POINT('Ctrl Pts',(3.18523730877148,3.7236989770682,1.09288068232638));
#17951=CARTESIAN_POINT('Ctrl Pts',(3.29615394353355,3.75794594469425,1.09873478250762));
#17952=CARTESIAN_POINT('Ctrl Pts',(3.40708065488555,3.79219602359978,1.10458941452402));
#17953=CARTESIAN_POINT('Ctrl Pts',(3.51951241675792,3.82152654323087,1.11044404654043));
#17954=CARTESIAN_POINT('Ctrl Pts',(3.63297472209708,3.84582188866319,1.11629867855683));
#17955=CARTESIAN_POINT('Ctrl Pts',(3.74647473218941,3.87012530770198,1.12215525613088));
#17956=CARTESIAN_POINT('Ctrl Pts',(3.86100556320786,3.88939013893042,1.12801183370492));
#17957=CARTESIAN_POINT('Ctrl Pts',(3.97608346737002,3.90355205396167,1.13386841127897));
#17958=CARTESIAN_POINT('Ctrl Pts',(4.09129141055242,3.91772997207856,1.13973160683598));
#17959=CARTESIAN_POINT('Ctrl Pts',(4.20704725074402,3.92679341422568,1.14559480239299));
#17960=CARTESIAN_POINT('Ctrl Pts',(4.32286298031701,3.93073000893239,1.15145799795));
#17961=CARTESIAN_POINT('Ctrl Pts',(4.43875661605547,3.93466925168182,1.15732513752295));
#17962=CARTESIAN_POINT('Ctrl Pts',(4.55470980954187,3.93347478398154,1.1631922770959));
#17963=CARTESIAN_POINT('Ctrl Pts',(4.67023715244117,3.92718629840934,1.16905941666885));
#17964=CARTESIAN_POINT('Ctrl Pts',(4.78593289379385,3.92088864642494,1.17493510847892));
#17965=CARTESIAN_POINT('Ctrl Pts',(4.90120113639546,3.90948219795967,1.18081080028899));
#17966=CARTESIAN_POINT('Ctrl Pts',(5.01556409209311,3.89305815481475,1.18668649209905));
#17967=CARTESIAN_POINT('Ctrl Pts',(5.04417717223732,3.88894893553188,1.18815656288936));
#17968=CARTESIAN_POINT('Ctrl Pts',(5.0727336478532,3.88452587313218,1.18962663367966));
#17969=CARTESIAN_POINT('Ctrl Pts',(5.10122617683407,3.87979088610339,1.19109670446997));
#17970=CARTESIAN_POINT('Ctrl Pts',(5.21506675973802,3.86087246423347,1.19697030438069));
#17971=CARTESIAN_POINT('Ctrl Pts',(5.32826262852322,3.83690799495832,1.20284390429142));
#17972=CARTESIAN_POINT('Ctrl Pts',(5.44033177785518,3.80795263144901,1.20871750420215));
#17973=CARTESIAN_POINT('Ctrl Pts',(5.55227467966402,3.77902988657691,1.21458448741733));
#17974=CARTESIAN_POINT('Ctrl Pts',(5.6630929884551,3.74512752236364,1.22045147063252));
#17975=CARTESIAN_POINT('Ctrl Pts',(5.77231213114212,3.70635213299535,1.22631845384771));
#17976=CARTESIAN_POINT('Ctrl Pts',(5.88141493970294,3.66761804500455,1.2321791878803));
#17977=CARTESIAN_POINT('Ctrl Pts',(5.98892158433081,3.62402139587162,1.23803992191289));
#17978=CARTESIAN_POINT('Ctrl Pts',(6.09437090185581,3.57571904766681,1.24390065594547));
#17979=CARTESIAN_POINT('Ctrl Pts',(6.19115331118495,3.53138668264788,1.2492796946479));
#17980=CARTESIAN_POINT('Ctrl Pts',(6.28620258476723,3.48309099504578,1.25465873335032));
#17981=CARTESIAN_POINT('Ctrl Pts',(6.37917532067788,3.4309896258774,1.26003777205275));
#17982=CARTESIAN_POINT('Ctrl Pts',(2.17296269996979,-3.20554048108048,-0.411765747138983));
#17983=CARTESIAN_POINT('Ctrl Pts',(1.10598262521586,-2.44554835076675,-0.345549597099719));
#17984=CARTESIAN_POINT('Ctrl Pts',(-0.190085171851759,0.209786400507346,
-0.213161407923235));
#17985=CARTESIAN_POINT('Ctrl Pts',(2.11904905146237,4.02596493684606,-0.0146011796095345));
#17986=CARTESIAN_POINT('Ctrl Pts',(6.57036830017086,4.14281137096193,0.183914937802122));
#17987=CARTESIAN_POINT('Ctrl Pts',(9.08469850437939,0.471525498888313,0.382431055213778));
#17988=CARTESIAN_POINT('Ctrl Pts',(7.36116941620609,-3.63455711911314,0.580947172625436));
#17989=CARTESIAN_POINT('Ctrl Pts',(2.97726580402431,-4.41062931823268,0.77946329003709));
#17990=CARTESIAN_POINT('Ctrl Pts',(-0.0518523842630756,-1.14834011450979,
0.977979407448747));
#17991=CARTESIAN_POINT('Ctrl Pts',(1.04758148582589,3.16599895701937,1.1764955248604));
#17992=CARTESIAN_POINT('Ctrl Pts',(5.26885307852876,4.58075644304919,1.37501164227206));
#17993=CARTESIAN_POINT('Ctrl Pts',(8.74613631193873,1.80065901519612,1.57352775968371));
#17994=CARTESIAN_POINT('Ctrl Pts',(8.2950356860829,-2.62850749839492,1.77204387709537));
#17995=CARTESIAN_POINT('Ctrl Pts',(4.32864266632258,-4.6505056552148,1.97055999450703));
#17996=CARTESIAN_POINT('Ctrl Pts',(0.479313869061077,-2.41367545883394,
2.16907611191868));
#17997=CARTESIAN_POINT('Ctrl Pts',(0.272186515624751,2.03356129066451,2.36759222933034));
#17998=CARTESIAN_POINT('Ctrl Pts',(3.89694643539194,4.61849687019083,2.56610834674199));
#17999=CARTESIAN_POINT('Ctrl Pts',(8.03410612006349,2.97390317522259,2.76462446415365));
#18000=CARTESIAN_POINT('Ctrl Pts',(8.89493411795877,-1.39413568050936,2.9631405815653));
#18001=CARTESIAN_POINT('Ctrl Pts',(5.69110016326603,-4.48545097223521,3.16165669897696));
#18002=CARTESIAN_POINT('Ctrl Pts',(1.35661463604595,-3.46907591290164,3.36017281638862));
#18003=CARTESIAN_POINT('Ctrl Pts',(-0.139083166427389,0.724213049156903,
3.55868893380027));
#18004=CARTESIAN_POINT('Ctrl Pts',(2.57373840321099,4.25428138787658,3.75720505121192));
#18005=CARTESIAN_POINT('Ctrl Pts',(7.01072892820446,3.88835980295648,3.95572116862359));
#18006=CARTESIAN_POINT('Ctrl Pts',(9.10857690015422,-0.0384477492421469,
4.15423728603523));
#18007=CARTESIAN_POINT('Ctrl Pts',(6.94611304441007,-3.93004557143118,4.3527534034469));
#18008=CARTESIAN_POINT('Ctrl Pts',(2.50368062941278,-4.22258242327136,4.55126952085854));
#18009=CARTESIAN_POINT('Ctrl Pts',(-0.15042524517621,-0.648158610486061,
4.74978563827021));
#18010=CARTESIAN_POINT('Ctrl Pts',(1.41437509517098,3.51983652671062,4.94830175568186));
#18011=CARTESIAN_POINT('Ctrl Pts',(5.76506726388787,4.46443232806813,5.14681787309352));
#18012=CARTESIAN_POINT('Ctrl Pts',(8.91737013208296,1.32058592540232,5.34533399050517));
#18013=CARTESIAN_POINT('Ctrl Pts',(7.98446469607637,-3.03262794728552,5.54385010791683));
#18014=CARTESIAN_POINT('Ctrl Pts',(3.82068800849579,-4.60861883268182,5.74236622532849));
#18015=CARTESIAN_POINT('Ctrl Pts',(0.239147556357015,-1.9641242562649,5.94088234274014));
#18016=CARTESIAN_POINT('Ctrl Pts',(0.519749957626067,2.47907795239849,6.13939846015179));
#18017=CARTESIAN_POINT('Ctrl Pts',(4.40552487083362,4.65198772933701,6.33791457756345));
#18018=CARTESIAN_POINT('Ctrl Pts',(8.33795354574623,2.56469563392857,6.53643069497511));
#18019=CARTESIAN_POINT('Ctrl Pts',(8.71579260460107,-1.87129593734266,6.73494681238676));
#18020=CARTESIAN_POINT('Ctrl Pts',(5.19302422456139,-4.59359028502123,6.93346292979842));
#18021=CARTESIAN_POINT('Ctrl Pts',(0.995732677906764,-3.10916202902842,
7.13197904721008));
#18022=CARTESIAN_POINT('Ctrl Pts',(-0.0322822778871914,1.22257767061497,
7.33049516462173));
#18023=CARTESIAN_POINT('Ctrl Pts',(3.05041589877745,4.43470399540276,7.52901128203338));
#18024=CARTESIAN_POINT('Ctrl Pts',(7.42075085684839,3.58561275821527,7.72752739944505));
#18025=CARTESIAN_POINT('Ctrl Pts',(9.07645297431008,-0.547114437358846,
7.9260435168567));
#18026=CARTESIAN_POINT('Ctrl Pts',(6.5012617467849,-4.17880463841992,8.12455963426836));
#18027=CARTESIAN_POINT('Ctrl Pts',(2.05348831510913,-3.98362504090881,8.32307575168001));
#18028=CARTESIAN_POINT('Ctrl Pts',(-0.193681017610346,-0.140317407516647,
8.52159186909167));
#18029=CARTESIAN_POINT('Ctrl Pts',(1.81766867783776,3.83149023855917,8.72010798650331));
#18030=CARTESIAN_POINT('Ctrl Pts',(6.24558161029013,4.2944920068349,8.91862410391498));
#18031=CARTESIAN_POINT('Ctrl Pts',(9.03505934404192,0.824679685151172,9.11714022132663));
#18032=CARTESIAN_POINT('Ctrl Pts',(7.6315512320161,-3.40035860512303,9.31565633873829));
#18033=CARTESIAN_POINT('Ctrl Pts',(3.32036330565075,-4.51141316650472,9.51417245614994));
#18034=CARTESIAN_POINT('Ctrl Pts',(0.0495994604212725,-1.49100136617927,
9.71268857356161));
#18035=CARTESIAN_POINT('Ctrl Pts',(0.814563009263402,2.89484112343983,9.91120469097325));
#18036=CARTESIAN_POINT('Ctrl Pts',(4.91471488529713,4.62964317792977,10.1097208083849));
#18037=CARTESIAN_POINT('Ctrl Pts',(8.59521399360942,2.1247060752228,10.3082369257966));
#18038=CARTESIAN_POINT('Ctrl Pts',(8.48552926132444,-2.32599643497811,10.5067530432082));
#18039=CARTESIAN_POINT('Ctrl Pts',(4.68610787984395,-4.64659565516981,10.7052691606199));
#18040=CARTESIAN_POINT('Ctrl Pts',(0.676387677669684,-2.71193096197848,
10.9037852780315));
#18041=CARTESIAN_POINT('Ctrl Pts',(0.128394142987057,1.70626851979591,11.1023013954432));
#18042=CARTESIAN_POINT('Ctrl Pts',(3.54396933091606,4.56189974780998,11.3008175128549));
#18043=CARTESIAN_POINT('Ctrl Pts',(7.79519445548059,3.23982996331418,11.4993336302665));
#18044=CARTESIAN_POINT('Ctrl Pts',(8.98887841448097,-1.04921447348414,11.6978497476782));
#18045=CARTESIAN_POINT('Ctrl Pts',(6.03186814454124,-4.3774082536412,11.8963658650898));
#18046=CARTESIAN_POINT('Ctrl Pts',(1.63213740257258,-3.69685482224785,12.0948819825015));
#18047=CARTESIAN_POINT('Ctrl Pts',(-0.181124089683036,0.369207933724872,
12.2933980999131));
#18048=CARTESIAN_POINT('Ctrl Pts',(2.2526340504912,4.09715708707193,12.4919142173248));
#18049=CARTESIAN_POINT('Ctrl Pts',(6.70462241331237,4.07300771627025,12.6904303347364));
#18050=CARTESIAN_POINT('Ctrl Pts',(9.09779474190718,0.318875355730261,12.8889464521481));
#18051=CARTESIAN_POINT('Ctrl Pts',(7.24052934071316,-3.72727698993507,13.0874625695597));
#18052=CARTESIAN_POINT('Ctrl Pts',(2.83367453520978,-4.36005996854408,13.2859786869714));
#18053=CARTESIAN_POINT('Ctrl Pts',(-0.0870558709899348,-0.999982965095223,
13.4844948043831));
#18054=CARTESIAN_POINT('Ctrl Pts',(1.1530874699283,3.2758594160949,13.6830109217947));
#18055=CARTESIAN_POINT('Ctrl Pts',(5.41840487637927,4.55173205747878,13.8815270392064));
#18056=CARTESIAN_POINT('Ctrl Pts',(8.80279980247531,1.65921506374814,14.080043156618));
#18057=CARTESIAN_POINT('Ctrl Pts',(8.20690775291552,-2.75277952374592,14.2785592740297));
#18058=CARTESIAN_POINT('Ctrl Pts',(4.17643533161801,-4.64383098681233,14.4770753914414));
#18059=CARTESIAN_POINT('Ctrl Pts',(0.402412514292184,-2.28215036718792,
14.675591508853));
#18060=CARTESIAN_POINT('Ctrl Pts',(0.341017607518878,2.16948014760412,14.8741076262646));
#18061=CARTESIAN_POINT('Ctrl Pts',(4.04847489906614,4.63434201110855,15.0726237436763));
#18062=CARTESIAN_POINT('Ctrl Pts',(8.12956552465056,2.85516161537223,15.271139861088));
#18063=CARTESIAN_POINT('Ctrl Pts',(8.84690431993714,-1.53872147678918,15.4696559784996));
#18064=CARTESIAN_POINT('Ctrl Pts',(5.54356606143321,-4.52347271009317,15.6681720959113));
#18065=CARTESIAN_POINT('Ctrl Pts',(1.24468509012015,-3.36571368106855,15.8666882133229));
#18066=CARTESIAN_POINT('Ctrl Pts',(-0.112905173860372,0.874301914415817,
16.0652043307346));
#18067=CARTESIAN_POINT('Ctrl Pts',(2.71405060913991,4.31364844766405,16.2637204481462));
#18068=CARTESIAN_POINT('Ctrl Pts',(7.1366801074503,3.80263778683562,16.4622365655579));
#18069=CARTESIAN_POINT('Ctrl Pts',(9.10482335385156,-0.190756225336315,
16.6607526829696));
#18070=CARTESIAN_POINT('Ctrl Pts',(6.81609220134375,-4.00945931491334,16.8592688003812));
#18071=CARTESIAN_POINT('Ctrl Pts',(2.36646310311057,-4.15637583189606,17.0577849177929));
#18072=CARTESIAN_POINT('Ctrl Pts',(-0.16917825360623,-0.496962424679848,
17.2563010352045));
#18073=CARTESIAN_POINT('Ctrl Pts',(1.53126025266144,3.61755971783011,17.4548171526162));
#18074=CARTESIAN_POINT('Ctrl Pts',(5.91054938364417,4.41918948403437,17.6533332700278));
#18075=CARTESIAN_POINT('Ctrl Pts',(8.95821945609951,1.17380958265607,17.8518493874395));
#18076=CARTESIAN_POINT('Ctrl Pts',(7.88327219050615,-3.14652280629029,18.0503655048511));
#18077=CARTESIAN_POINT('Ctrl Pts',(3.67012384502666,-4.58532946245115,18.2488816222628));
#18078=CARTESIAN_POINT('Ctrl Pts',(0.177095531876928,-1.82497861910485,
18.4473977396744));
#18079=CARTESIAN_POINT('Ctrl Pts',(0.603036135785551,2.60665292882547,18.6459138570862));
#18080=CARTESIAN_POINT('Ctrl Pts',(4.55787735396168,4.65116130836808,18.8444299744978));
#18081=CARTESIAN_POINT('Ctrl Pts',(8.41985082781949,2.43622463611074,19.0429460919094));
#18082=CARTESIAN_POINT('Ctrl Pts',(8.65223471259592,-2.00976021586402,19.2414622093211));
#18083=CARTESIAN_POINT('Ctrl Pts',(5.04221626688697,-4.61524489208584,19.4399783267328));
#18084=CARTESIAN_POINT('Ctrl Pts',(0.895781713701428,-2.99417608693739,
19.6384944441444));
#18085=CARTESIAN_POINT('Ctrl Pts',(0.0101569427980723,1.36890222246852,
19.8370105615561));
#18086=CARTESIAN_POINT('Ctrl Pts',(3.1963802739596,4.47836591752857,20.0355266789677));
#18087=CARTESIAN_POINT('Ctrl Pts',(7.53656898706393,3.48662728959027,20.2340427963793));
#18088=CARTESIAN_POINT('Ctrl Pts',(9.05606082131957,-0.698098281184544,
20.432558913791));
#18089=CARTESIAN_POINT('Ctrl Pts',(6.36333405195284,-4.24351873734398,20.6310750312027));
#18090=CARTESIAN_POINT('Ctrl Pts',(1.9243366462227,-3.90280543100934,20.8295911486144));
#18091=CARTESIAN_POINT('Ctrl Pts',(-0.195782035254683,0.0120228054752082,
21.028107266026));
#18092=CARTESIAN_POINT('Ctrl Pts',(1.94454241477252,3.91584087042925,21.2266233834376));
#18093=CARTESIAN_POINT('Ctrl Pts',(6.38524148680512,4.23360619038166,21.4251395008493));
#18094=CARTESIAN_POINT('Ctrl Pts',(9.05960761710739,0.674315805600993,21.623655618261));
#18095=CARTESIAN_POINT('Ctrl Pts',(7.5185068390623,-3.50250076674849,21.8221717356726));
#18096=CARTESIAN_POINT('Ctrl Pts',(3.17325057532877,-4.47179261159471,22.0206878530843));
#18097=CARTESIAN_POINT('Ctrl Pts',(0.0031406198327811,-1.34590405051051,
22.2192039704959));
#18098=CARTESIAN_POINT('Ctrl Pts',(0.911305739869395,3.01254206724522,22.4177200879076));
#18099=CARTESIAN_POINT('Ctrl Pts',(5.06606104496655,4.6121513544261,22.6162362053192));
#18100=CARTESIAN_POINT('Ctrl Pts',(8.66256938155685,1.98805571626367,22.8147523227309));
#18101=CARTESIAN_POINT('Ctrl Pts',(8.4072000996685,-2.45669335535235,23.0132684401425));
#18102=CARTESIAN_POINT('Ctrl Pts',(4.53384760969594,-4.65159218721967,23.2117845575542));
#18103=CARTESIAN_POINT('Ctrl Pts',(0.589592923617338,-2.58676106216746,
23.4103006749659));
#18104=CARTESIAN_POINT('Ctrl Pts',(0.186627431348294,1.84718698340797,23.6088167923775));
#18105=CARTESIAN_POINT('Ctrl Pts',(3.69375302108596,4.58911293885384,23.8073329097892));
#18106=CARTESIAN_POINT('Ctrl Pts',(7.89964467060016,3.12919021086655,24.0058490272008));
#18107=CARTESIAN_POINT('Ctrl Pts',(8.95179466357075,-1.19786968887199,24.2043651446125));
#18108=CARTESIAN_POINT('Ctrl Pts',(5.88826072308503,-4.42509080397621,24.4028812620241));
#18109=CARTESIAN_POINT('Ctrl Pts',(1.51149918181804,-3.60542346049212,24.6013973794358));
#18110=CARTESIAN_POINT('Ctrl Pts',(-0.164376056275096,0.527120914407128,
24.7999134968474));
#18111=CARTESIAN_POINT('Ctrl Pts',(1.53399129555416,2.94325066577138,24.9322575751219));
#18112=CARTESIAN_POINT('Ctrl Pts',(2.70656526709436,3.52529833870864,24.9984296142591));
#18113=CARTESIAN_POINT('Ctrl Pts',(2.31196529717974,-3.01041142380583,-0.273445981108207));
#18114=CARTESIAN_POINT('Ctrl Pts',(1.30993489857133,-2.29668186568531,-0.207229831068943));
#18115=CARTESIAN_POINT('Ctrl Pts',(0.0927619053280601,0.197016191301887,
-0.0748416418924601));
#18116=CARTESIAN_POINT('Ctrl Pts',(2.26133350378215,3.78089464452436,0.123718586421241));
#18117=CARTESIAN_POINT('Ctrl Pts',(6.44169010710979,3.89062835157607,0.322234703832897));
#18118=CARTESIAN_POINT('Ctrl Pts',(8.80296690727615,0.442822593209179,0.520750821244553));
#18119=CARTESIAN_POINT('Ctrl Pts',(7.18435323294509,-3.41331277406459,0.719266938656211));
#18120=CARTESIAN_POINT('Ctrl Pts',(3.06730851213489,-4.14214356803415,0.917783056067867));
#18121=CARTESIAN_POINT('Ctrl Pts',(0.222580126422941,-1.07843785456408,
1.11629917347952));
#18122=CARTESIAN_POINT('Ctrl Pts',(1.25508877879203,2.97327688863128,1.31481529089117));
#18123=CARTESIAN_POINT('Ctrl Pts',(5.21940128729496,4.30191464036023,1.51333140830283));
#18124=CARTESIAN_POINT('Ctrl Pts',(8.48501382017349,1.69104851481962,1.71184752571448));
#18125=CARTESIAN_POINT('Ctrl Pts',(8.06137278822348,-2.46850384433775,1.91036364312614));
#18126=CARTESIAN_POINT('Ctrl Pts',(4.33642377308406,-4.36741804808325,2.1088797605378));
#18127=CARTESIAN_POINT('Ctrl Pts',(0.721412996069988,-2.26674915432179,
2.30739587794946));
#18128=CARTESIAN_POINT('Ctrl Pts',(0.526893989166935,1.90977346146706,2.50591199536111));
#18129=CARTESIAN_POINT('Ctrl Pts',(3.93100594327419,4.33735771577206,2.70442811277276));
#18130=CARTESIAN_POINT('Ctrl Pts',(7.81632664047099,2.79287444498747,2.90294423018442));
#18131=CARTESIAN_POINT('Ctrl Pts',(8.62475394129306,-1.30927124574203,3.10146034759608));
#18132=CARTESIAN_POINT('Ctrl Pts',(5.61594516345689,-4.21241064570382,3.29997646500774));
#18133=CARTESIAN_POINT('Ctrl Pts',(1.54531032840212,-3.25790481196126,3.49849258241939));
#18134=CARTESIAN_POINT('Ctrl Pts',(0.140659294449413,0.680128436785933,
3.69700869983105));
#18135=CARTESIAN_POINT('Ctrl Pts',(2.68834480713824,3.99531291703776,3.8955248172427));
#18136=CARTESIAN_POINT('Ctrl Pts',(6.85524491106594,3.65166587031902,4.09404093465435));
#18137=CARTESIAN_POINT('Ctrl Pts',(8.82539176693615,-0.0361073410931478,
4.29255705206602));
#18138=CARTESIAN_POINT('Ctrl Pts',(6.79456235351217,-3.69081412452673,4.49107316947766));
#18139=CARTESIAN_POINT('Ctrl Pts',(2.62255162068078,-3.96554354562172,4.68958928688933));
#18140=CARTESIAN_POINT('Ctrl Pts',(0.130007635661538,-0.608703617053558,
4.88810540430098));
#18141=CARTESIAN_POINT('Ctrl Pts',(1.59955476768487,3.30557550356288,5.08662152171263));
#18142=CARTESIAN_POINT('Ctrl Pts',(5.68540970649173,4.19267145760527,5.28513763912429));
#18143=CARTESIAN_POINT('Ctrl Pts',(8.64582422058695,1.24019864338394,5.48365375653594));
#18144=CARTESIAN_POINT('Ctrl Pts',(7.76970701088062,-2.84802449713069,5.68216987394761));
#18145=CARTESIAN_POINT('Ctrl Pts',(3.85938955257665,-4.32808097846753,5.88068599135924));
#18146=CARTESIAN_POINT('Ctrl Pts',(0.495866191827503,-1.844563228489,6.07920210877092));
#18147=CARTESIAN_POINT('Ctrl Pts',(0.759387641428115,2.32817043879295,6.27771822618256));
#18148=CARTESIAN_POINT('Ctrl Pts',(4.40862597053364,4.36880990474354,6.47623434359423));
#18149=CARTESIAN_POINT('Ctrl Pts',(8.10167813322798,2.40857636349708,6.67475046100588));
#18150=CARTESIAN_POINT('Ctrl Pts',(8.45651720821394,-1.75738559545474,6.87326657841754));
#18151=CARTESIAN_POINT('Ctrl Pts',(5.14818832037566,-4.31396725511023,7.0717826958292));
#18152=CARTESIAN_POINT('Ctrl Pts',(1.20639613410644,-2.9198997628929,7.27029881324085));
#18153=CARTESIAN_POINT('Ctrl Pts',(0.240958952754043,1.14815638979818,7.4688149306525));
#18154=CARTESIAN_POINT('Ctrl Pts',(3.13600578243834,4.16475276096279,7.66733104806417));
#18155=CARTESIAN_POINT('Ctrl Pts',(7.24030780616454,3.36734777563528,7.86584716547581));
#18156=CARTESIAN_POINT('Ctrl Pts',(8.79522330270695,-0.513810248872322,
8.06436328288747));
#18157=CARTESIAN_POINT('Ctrl Pts',(6.37679023796107,-3.92443062116999,8.26287940029913));
#18158=CARTESIAN_POINT('Ctrl Pts',(2.1997636091463,-3.74113208118609,8.46139551771078));
#18159=CARTESIAN_POINT('Ctrl Pts',(0.089384947459713,-0.131775945129999,
8.65991163512245));
#18160=CARTESIAN_POINT('Ctrl Pts',(1.97829888761515,3.5982580948319,8.8584277525341));
#18161=CARTESIAN_POINT('Ctrl Pts',(6.13667397417128,4.03307581767334,9.05694386994575));
#18162=CARTESIAN_POINT('Ctrl Pts',(8.75634940354159,0.774479423926291,9.2554599873574));
#18163=CARTESIAN_POINT('Ctrl Pts',(7.43827624901926,-3.19337049409171,9.45397610476906));
#18164=CARTESIAN_POINT('Ctrl Pts',(3.38952083310589,-4.23679245796831,9.65249222218073));
#18165=CARTESIAN_POINT('Ctrl Pts',(0.317856350200649,-1.40024048117564,
9.85100833959237));
#18166=CARTESIAN_POINT('Ctrl Pts',(1.03625470449417,2.71862509287945,10.049524457004));
#18167=CARTESIAN_POINT('Ctrl Pts',(4.88682034851015,4.34782552060827,10.2480405744157));
#18168=CARTESIAN_POINT('Ctrl Pts',(8.34327851098385,1.99537004097493,10.4465566918273));
#18169=CARTESIAN_POINT('Ctrl Pts',(8.24027055552775,-2.18440736622039,10.645072809239));
#18170=CARTESIAN_POINT('Ctrl Pts',(4.67212920832948,-4.36374605926514,10.8435889266506));
#18171=CARTESIAN_POINT('Ctrl Pts',(0.906490441907856,-2.54684911848653,
11.0421050440623));
#18172=CARTESIAN_POINT('Ctrl Pts',(0.391854608507251,1.60240379879482,11.2406211614739));
#18173=CARTESIAN_POINT('Ctrl Pts',(3.59951541494433,4.28420579809219,11.4391372788856));
#18174=CARTESIAN_POINT('Ctrl Pts',(7.59195811086242,3.04261362173219,11.6376533962972));
#18175=CARTESIAN_POINT('Ctrl Pts',(8.71297961965247,-0.98534623276214,11.8361695137089));
#18176=CARTESIAN_POINT('Ctrl Pts',(5.93596976765481,-4.11094475056566,12.0346856311206));
#18177=CARTESIAN_POINT('Ctrl Pts',(1.80406135300024,-3.47181826426207,12.2332017485322));
#18178=CARTESIAN_POINT('Ctrl Pts',(0.101177504597399,0.346733347466743,
12.4317178659439));
#18179=CARTESIAN_POINT('Ctrl Pts',(2.38678685852808,3.84775315515312,12.6302339833555));
#18180=CARTESIAN_POINT('Ctrl Pts',(6.56777184536255,3.82507381537617,12.8287501007672));
#18181=CARTESIAN_POINT('Ctrl Pts',(8.81526594492522,0.29946463609684,13.0272662181788));
#18182=CARTESIAN_POINT('Ctrl Pts',(7.07105681270762,-3.5003885604986,13.2257823355905));
#18183=CARTESIAN_POINT('Ctrl Pts',(2.93245799361878,-4.09465249784007,13.4242984530022));
#18184=CARTESIAN_POINT('Ctrl Pts',(0.189519561683291,-0.939111566208993,
13.6228145704138));
#18185=CARTESIAN_POINT('Ctrl Pts',(1.35417235664619,3.07644987396012,13.8213306878255));
#18186=CARTESIAN_POINT('Ctrl Pts',(5.3598495029257,4.27465703983832,14.0198468052371));
#18187=CARTESIAN_POINT('Ctrl Pts',(8.53822806601778,1.55821460123144,14.2183629226488));
#18188=CARTESIAN_POINT('Ctrl Pts',(7.97860941701375,-2.58521112879858,14.4168790400604));
#18189=CARTESIAN_POINT('Ctrl Pts',(4.19348166959603,-4.36114968300486,14.6153951574721));
#18190=CARTESIAN_POINT('Ctrl Pts',(0.649192814085452,-2.14323031537866,
14.8139112748837));
#18191=CARTESIAN_POINT('Ctrl Pts',(0.59153516483578,2.03741860650786,15.0124273922954));
#18192=CARTESIAN_POINT('Ctrl Pts',(4.07331050026509,4.35223832436584,15.2109435097071));
#18193=CARTESIAN_POINT('Ctrl Pts',(7.9059751985768,2.68136097312093,15.4094596271187));
#18194=CARTESIAN_POINT('Ctrl Pts',(8.57964783407003,-1.44505575241412,15.6079757445304));
#18195=CARTESIAN_POINT('Ctrl Pts',(5.47739182177246,-4.24811790776339,15.806491861942));
#18196=CARTESIAN_POINT('Ctrl Pts',(1.44019420657955,-3.16083449095397,16.0050079793537));
#18197=CARTESIAN_POINT('Ctrl Pts',(0.165243768843413,0.821081027223728,
16.2035240967653));
#18198=CARTESIAN_POINT('Ctrl Pts',(2.82011586731386,4.05106615928717,16.402040214177));
#18199=CARTESIAN_POINT('Ctrl Pts',(6.97352913523386,3.57116196212476,16.6005563315886));
#18200=CARTESIAN_POINT('Ctrl Pts',(8.82186670813997,-0.17914442924803,16.7990724490003));
#18201=CARTESIAN_POINT('Ctrl Pts',(6.67245619587356,-3.76539376000376,16.997588566412));
#18202=CARTESIAN_POINT('Ctrl Pts',(2.49368685944485,-3.90336711073225,17.1961046838236));
#18203=CARTESIAN_POINT('Ctrl Pts',(0.112396168534027,-0.466711111367439,
17.3946208012353));
#18204=CARTESIAN_POINT('Ctrl Pts',(1.70932484092508,3.39735004600064,17.5931369186469));
#18205=CARTESIAN_POINT('Ctrl Pts',(5.82203597524696,4.15018265569229,17.7916530360586));
#18206=CARTESIAN_POINT('Ctrl Pts',(8.68418694674809,1.10235693414467,17.9901691534703));
#18207=CARTESIAN_POINT('Ctrl Pts',(7.67467433961344,-2.9549862986379,18.1886852708819));
#18208=CARTESIAN_POINT('Ctrl Pts',(3.71799059648846,-4.30620928893205,18.3872013882936));
#18209=CARTESIAN_POINT('Ctrl Pts',(0.437591425226463,-1.7138877251997,18.5857175057052));
#18210=CARTESIAN_POINT('Ctrl Pts',(0.837603987051035,2.44797961565228,18.7842336231169));
#18211=CARTESIAN_POINT('Ctrl Pts',(4.55170438690705,4.36803379003202,18.9827497405285));
#18212=CARTESIAN_POINT('Ctrl Pts',(8.17859012825258,2.28792570825151,19.1812658579402));
#18213=CARTESIAN_POINT('Ctrl Pts',(8.39682823991214,-1.88742121606535,19.3797819753518));
#18214=CARTESIAN_POINT('Ctrl Pts',(5.0065604104293,-4.33430369349561,19.5782980927635));
#18215=CARTESIAN_POINT('Ctrl Pts',(1.11252942855707,-2.81191329518458,19.7768142101752));
#18216=CARTESIAN_POINT('Ctrl Pts',(0.280814794700937,1.28557380975688,19.9753303275868));
#18217=CARTESIAN_POINT('Ctrl Pts',(3.27308495055695,4.20575687553525,20.1738464449984));
#18218=CARTESIAN_POINT('Ctrl Pts',(7.34907580467911,3.27438779359847,20.3723625624101));
#18219=CARTESIAN_POINT('Ctrl Pts',(8.77607246974106,-0.65560333835151,20.5708786798217));
#18220=CARTESIAN_POINT('Ctrl Pts',(6.24725853788356,-3.98520541525919,20.7693947972334));
#18221=CARTESIAN_POINT('Ctrl Pts',(2.07847371693811,-3.66523215780504,20.9679109146451));
#18222=CARTESIAN_POINT('Ctrl Pts',(0.0874118238771355,0.0112909480203034,
21.1664270320568));
#18223=CARTESIAN_POINT('Ctrl Pts',(2.09744951113826,3.6774740982752,21.3649431494684));
#18224=CARTESIAN_POINT('Ctrl Pts',(6.26783241381338,3.97589626917586,21.56345926688));
#18225=CARTESIAN_POINT('Ctrl Pts',(8.77940336342984,0.633268559987037,21.7619753842917));
#18226=CARTESIAN_POINT('Ctrl Pts',(7.33211314362288,-3.28929501353682,21.9604915017033));
#18227=CARTESIAN_POINT('Ctrl Pts',(3.25136321302202,-4.1995837027451,22.159007619115));
#18228=CARTESIAN_POINT('Ctrl Pts',(0.274225572405194,-1.26397559254583,
22.3575237365266));
#18229=CARTESIAN_POINT('Ctrl Pts',(1.12710846943813,2.82916129353447,22.5560398539383));
#18230=CARTESIAN_POINT('Ctrl Pts',(5.0289536987851,4.33139846700858,22.75455597135));
#18231=CARTESIAN_POINT('Ctrl Pts',(8.40653381239982,1.86703792222437,22.9530720887616));
#18232=CARTESIAN_POINT('Ctrl Pts',(8.1667094807393,-2.30714844669435,23.1515882061733));
#18233=CARTESIAN_POINT('Ctrl Pts',(4.52913739170739,-4.36843844023836,23.3501043235849));
#18234=CARTESIAN_POINT('Ctrl Pts',(0.824979095953012,-2.42929861537115,
23.5486204409966));
#18235=CARTESIAN_POINT('Ctrl Pts',(0.44654309475883,1.73474421227166,23.7471365584082));
#18236=CARTESIAN_POINT('Ctrl Pts',(3.74018140704413,4.30976245591016,23.9456526758199));
#18237=CARTESIAN_POINT('Ctrl Pts',(7.69005018696339,2.93870878051704,24.1441687932315));
#18238=CARTESIAN_POINT('Ctrl Pts',(8.67815324699032,-1.12495244308866,24.3426849106432));
#18239=CARTESIAN_POINT('Ctrl Pts',(5.80110407974766,-4.15572474791461,24.5412010280549));
#18240=CARTESIAN_POINT('Ctrl Pts',(1.69076667459873,-3.38595255220879,24.7397171454665));
#18241=CARTESIAN_POINT('Ctrl Pts',(0.116906044416222,0.495033780363739,
24.9382332628782));
#18242=CARTESIAN_POINT('Ctrl Pts',(1.71188963858453,2.76408782845127,25.0705773411526));
#18243=CARTESIAN_POINT('Ctrl Pts',(2.81308617627174,3.31070484176046,25.1367493802898));
#18244=CARTESIAN_POINT('Ctrl Pts',(2.45096789438968,-2.81528236653118,-0.135126215077433));
#18245=CARTESIAN_POINT('Ctrl Pts',(1.5138871719268,-2.14781538060387,-0.0689100650381678));
#18246=CARTESIAN_POINT('Ctrl Pts',(0.375608982507884,0.184245982096433,
0.0634781241383155));
#18247=CARTESIAN_POINT('Ctrl Pts',(2.40361795610193,3.53582435220265,0.262038352452016));
#18248=CARTESIAN_POINT('Ctrl Pts',(6.31301191404873,3.63844533219021,0.460554469863673));
#18249=CARTESIAN_POINT('Ctrl Pts',(8.52123531017291,0.41411968753004,0.659070587275328));
#18250=CARTESIAN_POINT('Ctrl Pts',(7.00753704968407,-3.19206842901602,0.857586704686986));
#18251=CARTESIAN_POINT('Ctrl Pts',(3.15735122024546,-3.87365781783563,1.05610282209864));
#18252=CARTESIAN_POINT('Ctrl Pts',(0.497012637108953,-1.00853559461836,
1.25461893951029));
#18253=CARTESIAN_POINT('Ctrl Pts',(1.46259607175817,2.78055482024318,1.45313505692195));
#18254=CARTESIAN_POINT('Ctrl Pts',(5.16994949606116,4.02307283767128,1.6516511743336));
#18255=CARTESIAN_POINT('Ctrl Pts',(8.22389132840824,1.58143801444312,1.85016729174526));
#18256=CARTESIAN_POINT('Ctrl Pts',(7.82770989036406,-2.30850019028058,2.04868340915692));
#18257=CARTESIAN_POINT('Ctrl Pts',(4.34420487984554,-4.08433044095169,2.24719952656857));
#18258=CARTESIAN_POINT('Ctrl Pts',(0.963512123078899,-2.11982284980964,
2.44571564398023));
#18259=CARTESIAN_POINT('Ctrl Pts',(0.781601462709117,1.78598563226962,2.64423176139188));
#18260=CARTESIAN_POINT('Ctrl Pts',(3.96506545115642,4.05621856135326,2.84274787880354));
#18261=CARTESIAN_POINT('Ctrl Pts',(7.59854716087849,2.61184571475234,3.0412639962152));
#18262=CARTESIAN_POINT('Ctrl Pts',(8.35457376462735,-1.22440681097471,3.23978011362686));
#18263=CARTESIAN_POINT('Ctrl Pts',(5.54079016364776,-3.93937031917242,3.43829623103851));
#18264=CARTESIAN_POINT('Ctrl Pts',(1.7340060207583,-3.04673371102089,3.63681234845017));
#18265=CARTESIAN_POINT('Ctrl Pts',(0.420401755326215,0.636043824414959,
3.83532846586182));
#18266=CARTESIAN_POINT('Ctrl Pts',(2.8029512110655,3.73634444619894,4.03384458327349));
#18267=CARTESIAN_POINT('Ctrl Pts',(6.6997608939274,3.41497193768155,4.23236070068513));
#18268=CARTESIAN_POINT('Ctrl Pts',(8.54220663371807,-0.0337669329441494,
4.4308768180968));
#18269=CARTESIAN_POINT('Ctrl Pts',(6.64301166261426,-3.45158267762228,4.62939293550844));
#18270=CARTESIAN_POINT('Ctrl Pts',(2.74142261194879,-3.70850466797209,4.82790905292011));
#18271=CARTESIAN_POINT('Ctrl Pts',(0.410440516499291,-0.569248623621048,
5.02642517033176));
#18272=CARTESIAN_POINT('Ctrl Pts',(1.78473444019877,3.09131448041513,5.22494128774342));
#18273=CARTESIAN_POINT('Ctrl Pts',(5.60575214909559,3.92091058714242,5.42345740515506));
#18274=CARTESIAN_POINT('Ctrl Pts',(8.37427830909092,1.15981136136555,5.62197352256674));
#18275=CARTESIAN_POINT('Ctrl Pts',(7.55494932568486,-2.66342104697584,5.82048963997839));
#18276=CARTESIAN_POINT('Ctrl Pts',(3.89809109665752,-4.04754312425325,6.01900575739004));
#18277=CARTESIAN_POINT('Ctrl Pts',(0.752584827297987,-1.72500220071308,
6.21752187480171));
#18278=CARTESIAN_POINT('Ctrl Pts',(0.999025325230166,2.17726292518741,6.41603799221334));
#18279=CARTESIAN_POINT('Ctrl Pts',(4.41172707023364,4.08563208015006,6.61455410962502));
#18280=CARTESIAN_POINT('Ctrl Pts',(7.86540272070975,2.25245709306557,6.81307022703666));
#18281=CARTESIAN_POINT('Ctrl Pts',(8.1972418118268,-1.64347525356681,7.01158634444832));
#18282=CARTESIAN_POINT('Ctrl Pts',(5.10335241618994,-4.03434422519923,7.21010246185998));
#18283=CARTESIAN_POINT('Ctrl Pts',(1.4170595903061,-2.73063749675737,7.40861857927163));
#18284=CARTESIAN_POINT('Ctrl Pts',(0.514200183395272,1.07373510898141,7.60713469668328));
#18285=CARTESIAN_POINT('Ctrl Pts',(3.22159566609925,3.89480152652282,7.80565081409495));
#18286=CARTESIAN_POINT('Ctrl Pts',(7.05986475548066,3.14908279305528,8.0041669315066));
#18287=CARTESIAN_POINT('Ctrl Pts',(8.51399363110384,-0.480506060385796,
8.20268304891826));
#18288=CARTESIAN_POINT('Ctrl Pts',(6.25231872913724,-3.67005660392007,8.40119916632992));
#18289=CARTESIAN_POINT('Ctrl Pts',(2.34603890318347,-3.49863912146337,8.59971528374156));
#18290=CARTESIAN_POINT('Ctrl Pts',(0.372450912529775,-0.123234482743352,
8.79823140115322));
#18291=CARTESIAN_POINT('Ctrl Pts',(2.13892909739252,3.36502595110463,8.99674751856487));
#18292=CARTESIAN_POINT('Ctrl Pts',(6.02776633805246,3.77165962851178,9.19526363597655));
#18293=CARTESIAN_POINT('Ctrl Pts',(8.47763946304124,0.72427916270141,9.39377975338818));
#18294=CARTESIAN_POINT('Ctrl Pts',(7.24500126602242,-2.98638238306039,9.59229587079984));
#18295=CARTESIAN_POINT('Ctrl Pts',(3.45867836056103,-3.9621717494319,9.79081198821151));
#18296=CARTESIAN_POINT('Ctrl Pts',(0.586113239980029,-1.30947959617202,
9.98932810562315));
#18297=CARTESIAN_POINT('Ctrl Pts',(1.25794639972494,2.54240906231909,10.1878442230349));
#18298=CARTESIAN_POINT('Ctrl Pts',(4.85892581172318,4.06600786328675,10.3863603404465));
#18299=CARTESIAN_POINT('Ctrl Pts',(8.09134302835829,1.86603400672705,10.5848764578582));
#18300=CARTESIAN_POINT('Ctrl Pts',(7.99501184973105,-2.04281829746266,10.7833925752698));
#18301=CARTESIAN_POINT('Ctrl Pts',(4.658150536815,-4.08089646336047,10.9819086926815));
#18302=CARTESIAN_POINT('Ctrl Pts',(1.13659320614603,-2.38176727499459,11.1804248100931));
#18303=CARTESIAN_POINT('Ctrl Pts',(0.655315074027438,1.49853907779376,11.3789409275048));
#18304=CARTESIAN_POINT('Ctrl Pts',(3.6550614989726,4.00651184837438,11.5774570449165));
#18305=CARTESIAN_POINT('Ctrl Pts',(7.38872176624422,2.84539728015019,11.7759731623281));
#18306=CARTESIAN_POINT('Ctrl Pts',(8.43708082482397,-0.921477992040132,
11.9744892797398));
#18307=CARTESIAN_POINT('Ctrl Pts',(5.84007139076835,-3.84448124749012,12.1730053971514));
#18308=CARTESIAN_POINT('Ctrl Pts',(1.97598530342792,-3.24678170627628,12.3715215145631));
#18309=CARTESIAN_POINT('Ctrl Pts',(0.383479098877827,0.324258761208613,
12.5700376319747));
#18310=CARTESIAN_POINT('Ctrl Pts',(2.52093966656498,3.59834922323431,12.7685537493864));
#18311=CARTESIAN_POINT('Ctrl Pts',(6.43092127741269,3.5771399144821,12.967069866798));
#18312=CARTESIAN_POINT('Ctrl Pts',(8.53273714794332,0.280053916463419,13.1655859842097));
#18313=CARTESIAN_POINT('Ctrl Pts',(6.90158428470204,-3.27350013106212,13.3641021016213));
#18314=CARTESIAN_POINT('Ctrl Pts',(3.0312414520278,-3.82924502713605,13.562618219033));
#18315=CARTESIAN_POINT('Ctrl Pts',(0.466094994356506,-0.878240167322765,
13.7611343364446));
#18316=CARTESIAN_POINT('Ctrl Pts',(1.55525724336407,2.87704033182534,13.9596504538563));
#18317=CARTESIAN_POINT('Ctrl Pts',(5.30129412947213,3.99758202219787,14.1581665712679));
#18318=CARTESIAN_POINT('Ctrl Pts',(8.27365632956023,1.45721413871475,14.3566826886797));
#18319=CARTESIAN_POINT('Ctrl Pts',(7.75031108111198,-2.41764273385123,14.5551988060912));
#18320=CARTESIAN_POINT('Ctrl Pts',(4.21052800757405,-4.07846837919741,14.753714923503));
#18321=CARTESIAN_POINT('Ctrl Pts',(0.895973113878727,-2.00431026356939,
14.9522310409146));
#18322=CARTESIAN_POINT('Ctrl Pts',(0.842052722152676,1.9053570654116,15.1507471583263));
#18323=CARTESIAN_POINT('Ctrl Pts',(4.09814610146403,4.07013463762311,15.3492632757379));
#18324=CARTESIAN_POINT('Ctrl Pts',(7.682384872503,2.50756033086961,15.5477793931496));
#18325=CARTESIAN_POINT('Ctrl Pts',(8.31239134820293,-1.35139002803904,15.7462955105612));
#18326=CARTESIAN_POINT('Ctrl Pts',(5.41121758211169,-3.97276310543362,15.9448116279729));
#18327=CARTESIAN_POINT('Ctrl Pts',(1.63570332303896,-2.95595530083938,16.1433277453845));
#18328=CARTESIAN_POINT('Ctrl Pts',(0.443392711547191,0.767860140031627,
16.3418438627962));
#18329=CARTESIAN_POINT('Ctrl Pts',(2.92618112548781,3.7884838709103,16.5403599802078));
#18330=CARTESIAN_POINT('Ctrl Pts',(6.8103781630174,3.33968613741389,16.7388760976195));
#18331=CARTESIAN_POINT('Ctrl Pts',(8.5389100624284,-0.167532633159739,16.9373922150311));
#18332=CARTESIAN_POINT('Ctrl Pts',(6.52882019040339,-3.5213282050942,17.1359083324428));
#18333=CARTESIAN_POINT('Ctrl Pts',(2.62091061577914,-3.65035838956845,17.3344244498544));
#18334=CARTESIAN_POINT('Ctrl Pts',(0.393970590674286,-0.43645979805503,
17.5329405672661));
#18335=CARTESIAN_POINT('Ctrl Pts',(1.88738942918871,3.17714037417117,17.7314566846778));
#18336=CARTESIAN_POINT('Ctrl Pts',(5.73352256684974,3.8811758273502,17.9299728020894));
#18337=CARTESIAN_POINT('Ctrl Pts',(8.41015443739666,1.03090428563328,18.1284889195011));
#18338=CARTESIAN_POINT('Ctrl Pts',(7.46607648872073,-2.76344979098553,18.3270050369127));
#18339=CARTESIAN_POINT('Ctrl Pts',(3.76585734795025,-4.02708911541293,18.5255211543244));
#18340=CARTESIAN_POINT('Ctrl Pts',(0.698087318576006,-1.60279683129456,
18.724037271736));
#18341=CARTESIAN_POINT('Ctrl Pts',(1.07217183831651,2.28930630247911,18.9225533891477));
#18342=CARTESIAN_POINT('Ctrl Pts',(4.54553141985243,4.08490627169594,19.1210695065593));
#18343=CARTESIAN_POINT('Ctrl Pts',(7.93732942868568,2.13962678039228,19.319585623971));
#18344=CARTESIAN_POINT('Ctrl Pts',(8.14142176722837,-1.76508221626667,19.5181017413827));
#18345=CARTESIAN_POINT('Ctrl Pts',(4.97090455397163,-4.05336249490537,19.7166178587943));
#18346=CARTESIAN_POINT('Ctrl Pts',(1.3292771434127,-2.62965050343175,19.915133976206));
#18347=CARTESIAN_POINT('Ctrl Pts',(0.551472646603815,1.20224539704524,20.1136500936177));
#18348=CARTESIAN_POINT('Ctrl Pts',(3.3497896271543,3.93314783354192,20.3121662110293));
#18349=CARTESIAN_POINT('Ctrl Pts',(7.16158262229433,3.06214829760668,20.510682328441));
#18350=CARTESIAN_POINT('Ctrl Pts',(8.49608411816253,-0.613108395518473,
20.7091984458526));
#18351=CARTESIAN_POINT('Ctrl Pts',(6.13118302381429,-3.72689209317441,20.9077145632643));
#18352=CARTESIAN_POINT('Ctrl Pts',(2.23261078765349,-3.42765888460072,21.1062306806759));
#18353=CARTESIAN_POINT('Ctrl Pts',(0.370605683008962,0.0105590905653954,
21.3047467980876));
#18354=CARTESIAN_POINT('Ctrl Pts',(2.250356607504,3.43910732612115,21.5032629154992));
#18355=CARTESIAN_POINT('Ctrl Pts',(6.15042334082164,3.71818634797007,21.7017790329109));
#18356=CARTESIAN_POINT('Ctrl Pts',(8.49919910975228,0.592221314373082,21.9002951503225));
#18357=CARTESIAN_POINT('Ctrl Pts',(7.14571944818345,-3.07608926032515,22.0988112677342));
#18358=CARTESIAN_POINT('Ctrl Pts',(3.32947585071529,-3.92737479389549,22.2973273851459));
#18359=CARTESIAN_POINT('Ctrl Pts',(0.545310524977601,-1.18204713458114,
22.4958435025575));
#18360=CARTESIAN_POINT('Ctrl Pts',(1.34291119900688,2.64578051982372,22.6943596199692));
#18361=CARTESIAN_POINT('Ctrl Pts',(4.99184635260365,4.05064557959106,22.8928757373808));
#18362=CARTESIAN_POINT('Ctrl Pts',(8.15049824324278,1.74602012818506,23.0913918547925));
#18363=CARTESIAN_POINT('Ctrl Pts',(7.92621886181009,-2.15760353803636,23.2899079722041));
#18364=CARTESIAN_POINT('Ctrl Pts',(4.52442717371885,-4.08528469325705,23.4884240896158));
#18365=CARTESIAN_POINT('Ctrl Pts',(1.06036526828869,-2.27183616857484,23.6869402070274));
#18366=CARTESIAN_POINT('Ctrl Pts',(0.706458758169362,1.62230144113535,23.8854563244391));
#18367=CARTESIAN_POINT('Ctrl Pts',(3.78660979300229,4.03041197296648,24.0839724418507));
#18368=CARTESIAN_POINT('Ctrl Pts',(7.48045570332662,2.74822735016753,24.2824885592624));
#18369=CARTESIAN_POINT('Ctrl Pts',(8.40451183040988,-1.05203519730533,24.481004676674));
#18370=CARTESIAN_POINT('Ctrl Pts',(5.71394743641032,-3.88635869185298,24.6795207940858));
#18371=CARTESIAN_POINT('Ctrl Pts',(1.87003416737941,-3.16648164392546,24.8780369114974));
#18372=CARTESIAN_POINT('Ctrl Pts',(0.398188145107553,0.462946646320358,
25.076553028909));
#18373=CARTESIAN_POINT('Ctrl Pts',(1.88978798161488,2.58492499113116,25.2088971071835));
#18374=CARTESIAN_POINT('Ctrl Pts',(2.91960708544911,3.09611134481228,25.2750691463207));
#18375=CARTESIAN_POINT('Ctrl Pts',(2.58997049159961,-2.62015330925654,0.00319355095334283));
#18376=CARTESIAN_POINT('Ctrl Pts',(1.71783944528228,-1.99894889552244,0.0694097009926075));
#18377=CARTESIAN_POINT('Ctrl Pts',(0.65845605968771,0.171475772890977,0.20179789016909));
#18378=CARTESIAN_POINT('Ctrl Pts',(2.5459024084217,3.29075405988094,0.400358118482792));
#18379=CARTESIAN_POINT('Ctrl Pts',(6.18433372098768,3.38626231280436,0.598874235894448));
#18380=CARTESIAN_POINT('Ctrl Pts',(8.23950371306965,0.385416781850904,0.797390353306103));
#18381=CARTESIAN_POINT('Ctrl Pts',(6.83072086642306,-2.97082408396747,0.995906470717762));
#18382=CARTESIAN_POINT('Ctrl Pts',(3.24739392835603,-3.60517206763711,1.19442258812942));
#18383=CARTESIAN_POINT('Ctrl Pts',(0.771445147794971,-0.938633334672633,
1.39293870554108));
#18384=CARTESIAN_POINT('Ctrl Pts',(1.6701033647243,2.58783275185508,1.59145482295273));
#18385=CARTESIAN_POINT('Ctrl Pts',(5.12049770482736,3.74423103498232,1.78997094036439));
#18386=CARTESIAN_POINT('Ctrl Pts',(7.96276883664299,1.47182751406662,1.98848705777604));
#18387=CARTESIAN_POINT('Ctrl Pts',(7.59404699250464,-2.14849653622342,2.1870031751877));
#18388=CARTESIAN_POINT('Ctrl Pts',(4.35198598660702,-3.80124283382013,2.38551929259936));
#18389=CARTESIAN_POINT('Ctrl Pts',(1.20561125008781,-1.97289654529749,2.58403541001101));
#18390=CARTESIAN_POINT('Ctrl Pts',(1.0363089362513,1.66219780307218,2.78255152742267));
#18391=CARTESIAN_POINT('Ctrl Pts',(3.99912495903867,3.77507940693446,2.98106764483432));
#18392=CARTESIAN_POINT('Ctrl Pts',(7.38076768128599,2.43081698451723,3.17958376224598));
#18393=CARTESIAN_POINT('Ctrl Pts',(8.08439358796167,-1.13954237620741,3.37809987965763));
#18394=CARTESIAN_POINT('Ctrl Pts',(5.4656351638386,-3.66632999264102,3.5766159970693));
#18395=CARTESIAN_POINT('Ctrl Pts',(1.92270171311447,-2.83556261008053,3.77513211448094));
#18396=CARTESIAN_POINT('Ctrl Pts',(0.700144216203009,0.591959212043988,
3.97364823189261));
#18397=CARTESIAN_POINT('Ctrl Pts',(2.91755761499276,3.47737597536012,4.17216434930425));
#18398=CARTESIAN_POINT('Ctrl Pts',(6.54427687678886,3.1782780050441,4.37068046671592));
#18399=CARTESIAN_POINT('Ctrl Pts',(8.2590215005,-0.0314265247951463,4.56919658412757));
#18400=CARTESIAN_POINT('Ctrl Pts',(6.49146097171637,-3.21235123071783,4.76771270153922));
#18401=CARTESIAN_POINT('Ctrl Pts',(2.86029360321679,-3.45146579032245,4.96622881895089));
#18402=CARTESIAN_POINT('Ctrl Pts',(0.690873397337037,-0.529793630188544,
5.16474493636253));
#18403=CARTESIAN_POINT('Ctrl Pts',(1.96991411271267,2.8770534572674,5.36326105377419));
#18404=CARTESIAN_POINT('Ctrl Pts',(5.52609459169944,3.64914971667956,5.56177717118585));
#18405=CARTESIAN_POINT('Ctrl Pts',(8.1027323975949,1.07942407934716,5.7602932885975));
#18406=CARTESIAN_POINT('Ctrl Pts',(7.34019164048911,-2.47881759682101,5.95880940600916));
#18407=CARTESIAN_POINT('Ctrl Pts',(3.93679264073839,-3.76700527003896,6.15732552342081));
#18408=CARTESIAN_POINT('Ctrl Pts',(1.00930346276847,-1.60544117293717,6.35584164083248));
#18409=CARTESIAN_POINT('Ctrl Pts',(1.23866300903221,2.02635541158186,6.55435775824412));
#18410=CARTESIAN_POINT('Ctrl Pts',(4.41482816993367,3.80245425555658,6.75287387565579));
#18411=CARTESIAN_POINT('Ctrl Pts',(7.6291273081915,2.09633782263408,6.95138999306744));
#18412=CARTESIAN_POINT('Ctrl Pts',(7.93796641543966,-1.5295649116789,7.14990611047909));
#18413=CARTESIAN_POINT('Ctrl Pts',(5.05851651200422,-3.75472119528823,7.34842222789076));
#18414=CARTESIAN_POINT('Ctrl Pts',(1.62772304650576,-2.54137523062185,7.5469383453024));
#18415=CARTESIAN_POINT('Ctrl Pts',(0.787441414036509,0.999313828164636,
7.74545446271406));
#18416=CARTESIAN_POINT('Ctrl Pts',(3.30718554976015,3.62485029208286,7.94397058012572));
#18417=CARTESIAN_POINT('Ctrl Pts',(6.8794217047968,2.93081781047529,8.14248669753737));
#18418=CARTESIAN_POINT('Ctrl Pts',(8.23276395950072,-0.447201871899268,
8.34100281494903));
#18419=CARTESIAN_POINT('Ctrl Pts',(6.12784722031342,-3.41568258667014,8.53951893236069));
#18420=CARTESIAN_POINT('Ctrl Pts',(2.49231419722064,-3.25614616174064,8.73803504977233));
#18421=CARTESIAN_POINT('Ctrl Pts',(0.655516877599837,-0.114693020356707,
8.93655116718401));
#18422=CARTESIAN_POINT('Ctrl Pts',(2.29955930716991,3.13179380737736,9.13506728459565));
#18423=CARTESIAN_POINT('Ctrl Pts',(5.9188587019336,3.51024343935022,9.33358340200731));
#18424=CARTESIAN_POINT('Ctrl Pts',(8.19892952254092,0.674078901476532,9.53209951941897));
#18425=CARTESIAN_POINT('Ctrl Pts',(7.05172628302556,-2.77939427202906,9.73061563683061));
#18426=CARTESIAN_POINT('Ctrl Pts',(3.52783588801619,-3.68755104089551,9.92913175424228));
#18427=CARTESIAN_POINT('Ctrl Pts',(0.854370129759403,-1.21871871116838,
10.1276478716539));
#18428=CARTESIAN_POINT('Ctrl Pts',(1.47963809495571,2.36619303175871,10.3261639890656));
#18429=CARTESIAN_POINT('Ctrl Pts',(4.83103127493619,3.78419020596524,10.5246801064772));
#18430=CARTESIAN_POINT('Ctrl Pts',(7.83940754573271,1.73669797247918,10.7231962238889));
#18431=CARTESIAN_POINT('Ctrl Pts',(7.74975314393437,-1.90122922870495,10.9217123413006));
#18432=CARTESIAN_POINT('Ctrl Pts',(4.64417186530054,-3.79804686745578,11.1202284587122));
#18433=CARTESIAN_POINT('Ctrl Pts',(1.36669597038421,-2.21668543150265,11.3187445761239));
#18434=CARTESIAN_POINT('Ctrl Pts',(0.91877553954763,1.39467435679268,11.5172606935355));
#18435=CARTESIAN_POINT('Ctrl Pts',(3.71060758300086,3.72881789865659,11.7157768109472));
#18436=CARTESIAN_POINT('Ctrl Pts',(7.18548542162604,2.64818093856821,11.9142929283589));
#18437=CARTESIAN_POINT('Ctrl Pts',(8.16118202999545,-0.857609751318129,
12.1128090457705));
#18438=CARTESIAN_POINT('Ctrl Pts',(5.74417301388192,-3.57801774441457,12.3113251631822));
#18439=CARTESIAN_POINT('Ctrl Pts',(2.14790925385559,-3.02174514829049,12.5098412805938));
#18440=CARTESIAN_POINT('Ctrl Pts',(0.665780693158256,0.301784174950485,
12.7083573980055));
#18441=CARTESIAN_POINT('Ctrl Pts',(2.65509247460188,3.34894529131551,12.9068735154171));
#18442=CARTESIAN_POINT('Ctrl Pts',(6.29407070946287,3.32920601358802,13.1053896328288));
#18443=CARTESIAN_POINT('Ctrl Pts',(8.25020835096136,0.260643196829997,13.3039057502404));
#18444=CARTESIAN_POINT('Ctrl Pts',(6.7321117566965,-3.04661170162563,13.5024218676521));
#18445=CARTESIAN_POINT('Ctrl Pts',(3.1300249104368,-3.56383755643203,13.7009379850637));
#18446=CARTESIAN_POINT('Ctrl Pts',(0.742670427029733,-0.817368768436538,
13.8994541024754));
#18447=CARTESIAN_POINT('Ctrl Pts',(1.75634213008195,2.67763078969056,14.0979702198871));
#18448=CARTESIAN_POINT('Ctrl Pts',(5.24273875601857,3.7205070045574,14.2964863372987));
#18449=CARTESIAN_POINT('Ctrl Pts',(8.0090845931027,1.35621367619806,14.4950024547104));
#18450=CARTESIAN_POINT('Ctrl Pts',(7.52201274521021,-2.25007433890389,14.693518572122));
#18451=CARTESIAN_POINT('Ctrl Pts',(4.22757434555207,-3.79578707538995,14.8920346895337));
#18452=CARTESIAN_POINT('Ctrl Pts',(1.14275341367199,-1.86539021176013,15.0905508069453));
#18453=CARTESIAN_POINT('Ctrl Pts',(1.09257027946957,1.77329552431533,15.289066924357));
#18454=CARTESIAN_POINT('Ctrl Pts',(4.12298170266298,3.78803095088039,15.4875830417686));
#18455=CARTESIAN_POINT('Ctrl Pts',(7.45879454642923,2.3337596886183,15.6860991591803));
#18456=CARTESIAN_POINT('Ctrl Pts',(8.04513486233581,-1.25772430366396,15.8846152765919));
#18457=CARTESIAN_POINT('Ctrl Pts',(5.34504334245093,-3.69740830310385,16.0831313940036));
#18458=CARTESIAN_POINT('Ctrl Pts',(1.83121243949837,-2.75107611072479,16.2816475114153));
#18459=CARTESIAN_POINT('Ctrl Pts',(0.721541654250978,0.714639252839528,
16.4801636288269));
#18460=CARTESIAN_POINT('Ctrl Pts',(3.03224638366176,3.52590158253341,16.6786797462386));
#18461=CARTESIAN_POINT('Ctrl Pts',(6.64722719080097,3.10821031270302,16.8771958636502));
#18462=CARTESIAN_POINT('Ctrl Pts',(8.25595341671681,-0.155920837071448,
17.0757119810619));
#18463=CARTESIAN_POINT('Ctrl Pts',(6.38518418493321,-3.27726265018464,17.2742280984735));
#18464=CARTESIAN_POINT('Ctrl Pts',(2.74813437211341,-3.39734966840464,17.4727442158852));
#18465=CARTESIAN_POINT('Ctrl Pts',(0.675545012814546,-0.406208484742623,
17.6712603332969));
#18466=CARTESIAN_POINT('Ctrl Pts',(2.06545401745235,2.9569307023417,17.8697764507085));
#18467=CARTESIAN_POINT('Ctrl Pts',(5.64500915845253,3.61216899900811,18.0682925681202));
#18468=CARTESIAN_POINT('Ctrl Pts',(8.13612192804524,0.959451637121888,18.2668086855318));
#18469=CARTESIAN_POINT('Ctrl Pts',(7.25747863782803,-2.57191328333314,18.4653248029435));
#18470=CARTESIAN_POINT('Ctrl Pts',(3.81372409941205,-3.74796894189382,18.6638409203551));
#18471=CARTESIAN_POINT('Ctrl Pts',(0.958583211925542,-1.49170593738941,
18.8623570377668));
#18472=CARTESIAN_POINT('Ctrl Pts',(1.306739689582,2.13063298930591,19.0608731551785));
#18473=CARTESIAN_POINT('Ctrl Pts',(4.53935845279781,3.80177875335989,19.2593892725901));
#18474=CARTESIAN_POINT('Ctrl Pts',(7.69606872911877,1.99132785253305,19.4579053900018));
#18475=CARTESIAN_POINT('Ctrl Pts',(7.88601529454458,-1.64274321646801,19.6564215074134));
#18476=CARTESIAN_POINT('Ctrl Pts',(4.93524869751396,-3.77242129631514,19.8549376248251));
#18477=CARTESIAN_POINT('Ctrl Pts',(1.54602485826833,-2.44738771167893,20.0534537422367));
#18478=CARTESIAN_POINT('Ctrl Pts',(0.822130498506685,1.11891698433359,20.2519698596484));
#18479=CARTESIAN_POINT('Ctrl Pts',(3.42649430375165,3.66053879154859,20.45048597706));
#18480=CARTESIAN_POINT('Ctrl Pts',(6.97408943990954,2.84990880161489,20.6490020944717));
#18481=CARTESIAN_POINT('Ctrl Pts',(8.21609576658401,-0.570613452685432,
20.8475182118833));
#18482=CARTESIAN_POINT('Ctrl Pts',(6.015107509745,-3.46857877108964,21.046034329295));
#18483=CARTESIAN_POINT('Ctrl Pts',(2.38674785836889,-3.19008561139642,21.2445504467067));
#18484=CARTESIAN_POINT('Ctrl Pts',(0.653799542140776,0.00982723311048271,
21.4430665641183));
#18485=CARTESIAN_POINT('Ctrl Pts',(2.40326370386975,3.2007405539671,21.64158268153));
#18486=CARTESIAN_POINT('Ctrl Pts',(6.03301426782987,3.46047642676426,21.8400987989417));
#18487=CARTESIAN_POINT('Ctrl Pts',(8.21899485607472,0.551174068759129,22.0386149163533));
#18488=CARTESIAN_POINT('Ctrl Pts',(6.95932575274402,-2.86288350711349,22.2371310337649));
#18489=CARTESIAN_POINT('Ctrl Pts',(3.40758848840856,-3.65516588504588,22.4356471511766));
#18490=CARTESIAN_POINT('Ctrl Pts',(0.816395477550012,-1.10011867661645,
22.6341632685882));
#18491=CARTESIAN_POINT('Ctrl Pts',(1.55871392857562,2.46239974611297,22.8326793859999));
#18492=CARTESIAN_POINT('Ctrl Pts',(4.95473900642221,3.76989269217354,23.0311955034116));
#18493=CARTESIAN_POINT('Ctrl Pts',(7.89446267408575,1.62500233414576,23.2297116208232));
#18494=CARTESIAN_POINT('Ctrl Pts',(7.68572824288089,-2.00805862937836,23.4282277382349));
#18495=CARTESIAN_POINT('Ctrl Pts',(4.5197169557303,-3.80213094627573,23.6267438556465));
#18496=CARTESIAN_POINT('Ctrl Pts',(1.29575144062437,-2.11437372177854,23.8252599730582));
#18497=CARTESIAN_POINT('Ctrl Pts',(0.966374421579891,1.50985866999905,24.0237760904698));
#18498=CARTESIAN_POINT('Ctrl Pts',(3.83303817896047,3.7510614900228,24.2222922078815));
#18499=CARTESIAN_POINT('Ctrl Pts',(7.27086121968984,2.55774591981802,24.4208083252931));
#18500=CARTESIAN_POINT('Ctrl Pts',(8.13087041382945,-0.979117951521988,
24.6193244427048));
#18501=CARTESIAN_POINT('Ctrl Pts',(5.62679079307294,-3.61699263579137,24.8178405601165));
#18502=CARTESIAN_POINT('Ctrl Pts',(2.04930166016011,-2.94701073564213,25.0163566775281));
#18503=CARTESIAN_POINT('Ctrl Pts',(0.679470245798868,0.430859512276974,
25.2148727949398));
#18504=CARTESIAN_POINT('Ctrl Pts',(2.06768632464525,2.40576215381105,25.3472168732142));
#18505=CARTESIAN_POINT('Ctrl Pts',(3.02612799462649,2.8815178478641,25.4133889123514));
#18506=CARTESIAN_POINT('Ctrl Pts',(7.67921910621823,-4.71466720739905E-12,
7.06143953130409));
#18507=CARTESIAN_POINT('Ctrl Pts',(7.67921910621831,0.0545498630660913,
7.05794747266055));
#18508=CARTESIAN_POINT('Ctrl Pts',(7.67783410610462,0.109093485856064,7.05449675160843));
#18509=CARTESIAN_POINT('Ctrl Pts',(7.67397229027254,0.185079155343071,7.04974406424712));
#18510=CARTESIAN_POINT('Ctrl Pts',(7.67266413224706,0.206568690253113,7.04840602391199));
#18511=CARTESIAN_POINT('Ctrl Pts',(7.67020844577946,0.241185816649767,7.04626001003213));
#18512=CARTESIAN_POINT('Ctrl Pts',(7.66919559031489,0.254322015162662,7.04544784665494));
#18513=CARTESIAN_POINT('Ctrl Pts',(7.66692191112318,0.281624966894758,7.04376421665415));
#18514=CARTESIAN_POINT('Ctrl Pts',(7.66564780386039,0.295790350290824,7.04289318545173));
#18515=CARTESIAN_POINT('Ctrl Pts',(7.66241913326567,0.329205624482212,7.04084409294529));
#18516=CARTESIAN_POINT('Ctrl Pts',(7.66038489069605,0.348447399679791,7.03966855651076));
#18517=CARTESIAN_POINT('Ctrl Pts',(7.6530305271936,0.412489953607678,7.03576978018177));
#18518=CARTESIAN_POINT('Ctrl Pts',(7.64694286227679,0.457198418187983,7.0330706032779));
#18519=CARTESIAN_POINT('Ctrl Pts',(7.63014773790944,0.563754898121742,7.02668095458917));
#18520=CARTESIAN_POINT('Ctrl Pts',(7.61856835416684,0.625447582698257,7.02301702342752));
#18521=CARTESIAN_POINT('Ctrl Pts',(7.53208656273389,1.02195459713622,6.99959512792977));
#18522=CARTESIAN_POINT('Ctrl Pts',(7.4059461969243,1.34325170704917,6.98144958759926));
#18523=CARTESIAN_POINT('Ctrl Pts',(7.21453106278311,1.66743364901107,6.95901953622476));
#18524=CARTESIAN_POINT('Ctrl Pts',(7.19704299798727,1.69602337056475,6.95700035940156));
#18525=CARTESIAN_POINT('Ctrl Pts',(7.1724331160615,1.73488124331287,6.95419170118274));
#18526=CARTESIAN_POINT('Ctrl Pts',(7.16569204497459,1.74538949448345,6.9534255965834));
#18527=CARTESIAN_POINT('Ctrl Pts',(7.15484438255907,1.76208500746242,6.9521974547987));
#18528=CARTESIAN_POINT('Ctrl Pts',(7.15077708781622,1.76829782648793,6.95173799300674));
#18529=CARTESIAN_POINT('Ctrl Pts',(7.14224598542037,1.78123137515562,6.95077628348628));
#18530=CARTESIAN_POINT('Ctrl Pts',(7.13777838645317,1.78794943866016,6.95027376979013));
#18531=CARTESIAN_POINT('Ctrl Pts',(7.12681494783224,1.80430198963618,6.94904344895844));
#18532=CARTESIAN_POINT('Ctrl Pts',(7.12029216956595,1.81391820683403,6.94831386601263));
#18533=CARTESIAN_POINT('Ctrl Pts',(7.09664511410958,1.84837729442617,6.94567809970447));
#18534=CARTESIAN_POINT('Ctrl Pts',(7.0792247380929,1.87301380605635,6.94375348487185));
#18535=CARTESIAN_POINT('Ctrl Pts',(7.03482017917462,1.93397801363059,6.93889682132624));
#18536=CARTESIAN_POINT('Ctrl Pts',(7.00741244238302,1.96998804594177,6.93594259379422));
#18537=CARTESIAN_POINT('Ctrl Pts',(6.88300525647569,2.12649139742149,6.92276058556181));
#18538=CARTESIAN_POINT('Ctrl Pts',(6.77816524591359,2.24048354031629,6.91224862792232));
#18539=CARTESIAN_POINT('Ctrl Pts',(6.50860736048722,2.49425508036803,6.88722768406429));
#18540=CARTESIAN_POINT('Ctrl Pts',(6.33721225166477,2.6259120767463,6.87286630142336));
#18541=CARTESIAN_POINT('Ctrl Pts',(6.12199490454193,2.75926665925321,6.85679631632119));
#18542=CARTESIAN_POINT('Ctrl Pts',(6.08971857443983,2.77849330529497,6.85443207935948));
#18543=CARTESIAN_POINT('Ctrl Pts',(6.03940100920803,2.80728704713101,6.85081504063938));
#18544=CARTESIAN_POINT('Ctrl Pts',(6.02159350464018,2.81725391519632,6.84954795653557));
#18545=CARTESIAN_POINT('Ctrl Pts',(5.99117344482579,2.83390257713619,6.84740504987146));
#18546=CARTESIAN_POINT('Ctrl Pts',(5.97860916200309,2.84067085116231,6.84652616077616));
#18547=CARTESIAN_POINT('Ctrl Pts',(5.95307214613288,2.8542093497338,6.84475212417148));
#18548=CARTESIAN_POINT('Ctrl Pts',(5.94009742753306,2.86097512860345,6.84385714923083));
#18549=CARTESIAN_POINT('Ctrl Pts',(5.9079452940464,2.87746359089304,6.84165475441424));
#18550=CARTESIAN_POINT('Ctrl Pts',(5.88871563032272,2.88708326332889,6.84035096422927));
#18551=CARTESIAN_POINT('Ctrl Pts',(5.81610436206522,2.92250314298512,6.83547655693551));
#18552=CARTESIAN_POINT('Ctrl Pts',(5.76210853617939,2.94702205490176,6.83195016001737));
#18553=CARTESIAN_POINT('Ctrl Pts',(5.62381835365986,3.00527057658443,6.82313671059623));
#18554=CARTESIAN_POINT('Ctrl Pts',(5.53871763960454,3.03695495190129,6.81791355744433));
#18555=CARTESIAN_POINT('Ctrl Pts',(5.32004022474157,3.10801025218747,6.80484974487328));
#18556=CARTESIAN_POINT('Ctrl Pts',(5.18504351812508,3.14239769296895,6.79711620624979));
#18557=CARTESIAN_POINT('Ctrl Pts',(4.88632415695871,3.19819886884139,6.78009289464508));
#18558=CARTESIAN_POINT('Ctrl Pts',(4.72233958322252,3.21598370194662,6.77080282897045));
#18559=CARTESIAN_POINT('Ctrl Pts',(4.53071098778791,3.22200820053171,6.75931067882571));
#18560=CARTESIAN_POINT('Ctrl Pts',(4.50367614109252,3.22251766300787,6.75767450568788));
#18561=CARTESIAN_POINT('Ctrl Pts',(4.4663052108205,3.22275155838395,6.75538832135935));
#18562=CARTESIAN_POINT('Ctrl Pts',(4.4559712302031,3.22276652914662,6.7547535498709));
#18563=CARTESIAN_POINT('Ctrl Pts',(4.4382326663515,3.22270690991921,6.75365923699334));
#18564=CARTESIAN_POINT('Ctrl Pts',(4.43082800828194,3.22265650147056,6.7532010259754));
#18565=CARTESIAN_POINT('Ctrl Pts',(4.41533765113833,3.22249765812268,6.75223939045816));
#18566=CARTESIAN_POINT('Ctrl Pts',(4.40725213376453,3.22238430944009,6.75173568443449));
#18567=CARTESIAN_POINT('Ctrl Pts',(4.38745473400983,3.22203224781219,6.75049818339108));
#18568=CARTESIAN_POINT('Ctrl Pts',(4.37574362641558,3.2217601053569,6.74976256505833));
#18569=CARTESIAN_POINT('Ctrl Pts',(4.33324338548577,3.22054061551258,6.74708061424375));
#18570=CARTESIAN_POINT('Ctrl Pts',(4.30246783862567,3.2192157246286,6.74511501416291));
#18571=CARTESIAN_POINT('Ctrl Pts',(4.22526128858735,3.21478238617426,6.74013260070047));
#18572=CARTESIAN_POINT('Ctrl Pts',(4.1788707185064,3.21110908295534,6.73709220825989));
#18573=CARTESIAN_POINT('Ctrl Pts',(3.80599027407461,3.17344339261597,6.71235907738362));
#18574=CARTESIAN_POINT('Ctrl Pts',(3.486332456222,3.0907556932948,6.68959230843498));
#18575=CARTESIAN_POINT('Ctrl Pts',(3.11979746471539,2.93332655536681,6.66383483414238));
#18576=CARTESIAN_POINT('Ctrl Pts',(3.05589615559065,2.90335881580813,6.65934585249315));
#18577=CARTESIAN_POINT('Ctrl Pts',(2.97190778834495,2.86055188500096,6.65344450995049));
#18578=CARTESIAN_POINT('Ctrl Pts',(2.95090853225848,2.8495555442316,6.65196884671701));
#18579=CARTESIAN_POINT('Ctrl Pts',(2.91673344162846,2.83117637183442,6.64956651451181));
#18580=CARTESIAN_POINT('Ctrl Pts',(2.90348508964356,2.82393098745104,6.64863502870482));
#18581=CARTESIAN_POINT('Ctrl Pts',(2.87791383845791,2.80971195893903,6.64683655592072));
#18582=CARTESIAN_POINT('Ctrl Pts',(2.86558503518017,2.80274970487728,6.64596918919227));
#18583=CARTESIAN_POINT('Ctrl Pts',(2.83685329473996,2.78627380744042,6.64394699982994));
#18584=CARTESIAN_POINT('Ctrl Pts',(2.82048753523173,2.77669613569922,6.64279451309375));
#18585=CARTESIAN_POINT('Ctrl Pts',(2.76740056055959,2.74499595198367,6.6390531587996));
#18586=CARTESIAN_POINT('Ctrl Pts',(2.73103512065816,2.72228454611836,6.63648571237267));
#18587=CARTESIAN_POINT('Ctrl Pts',(2.64597800151533,2.66677422141495,6.63046069388591));
#18588=CARTESIAN_POINT('Ctrl Pts',(2.59770739603153,2.63335684437312,6.62702565189595));
#18589=CARTESIAN_POINT('Ctrl Pts',(2.32466469171216,2.4330806882104,6.60742857800775));
#18590=CARTESIAN_POINT('Ctrl Pts',(2.12150553136897,2.23883961320361,6.59229460778197));
#18591=CARTESIAN_POINT('Ctrl Pts',(1.88712318114709,1.94766412125108,6.57087024492528));
#18592=CARTESIAN_POINT('Ctrl Pts',(1.83147651957991,1.87198945180368,6.56538487669216));
#18593=CARTESIAN_POINT('Ctrl Pts',(1.77035223314986,1.78077155976628,6.55873008886696));
#18594=CARTESIAN_POINT('Ctrl Pts',(1.76158506924278,1.76747594259092,6.5577590752292));
#18595=CARTESIAN_POINT('Ctrl Pts',(1.74750260969583,1.74577118725325,6.55617130538348));
#18596=CARTESIAN_POINT('Ctrl Pts',(1.74212695631936,1.73740127911217,6.5555583957658));
#18597=CARTESIAN_POINT('Ctrl Pts',(1.73259000765924,1.72239992766327,6.55445851383493));
#18598=CARTESIAN_POINT('Ctrl Pts',(1.72841402400765,1.71577805109736,6.55397252102732));
#18599=CARTESIAN_POINT('Ctrl Pts',(1.71933975850382,1.70127206672224,6.55290678858469));
#18600=CARTESIAN_POINT('Ctrl Pts',(1.71445146408054,1.69338210580463,6.55232643795355));
#18601=CARTESIAN_POINT('Ctrl Pts',(1.70059138453959,1.67079384729648,6.55066323723582));
#18602=CARTESIAN_POINT('Ctrl Pts',(1.69170338883237,1.6560448648964,6.54957519841967));
#18603=CARTESIAN_POINT('Ctrl Pts',(1.63028708352406,1.55225642267066,6.54190821677805));
#18604=CARTESIAN_POINT('Ctrl Pts',(1.581956513041,1.46081408225307,6.53510124996775));
#18605=CARTESIAN_POINT('Ctrl Pts',(1.44766852525336,1.17417306079102,6.51394136699242));
#18606=CARTESIAN_POINT('Ctrl Pts',(1.37659953460437,0.972612949668182,6.49934281088194));
#18607=CARTESIAN_POINT('Ctrl Pts',(1.29312558635291,0.631252147921198,6.47602193979214));
#18608=CARTESIAN_POINT('Ctrl Pts',(1.26896214407291,0.495004713421878,6.46705093425879));
#18609=CARTESIAN_POINT('Ctrl Pts',(1.25070726795639,0.33150916594133,6.45670309542836));
#18610=CARTESIAN_POINT('Ctrl Pts',(1.24811213979421,0.305373430999844,6.45506114259031));
#18611=CARTESIAN_POINT('Ctrl Pts',(1.24434977985552,0.262109829862578,6.45236273293054));
#18612=CARTESIAN_POINT('Ctrl Pts',(1.24299942787276,0.244999539383633,6.45130059021131));
#18613=CARTESIAN_POINT('Ctrl Pts',(1.24079978475586,0.213969230666835,6.44938325016281));
#18614=CARTESIAN_POINT('Ctrl Pts',(1.23990404209925,0.200053029587059,6.44852661909977));
#18615=CARTESIAN_POINT('Ctrl Pts',(1.23817025693055,0.170083702153091,6.44668860698538));
#18616=CARTESIAN_POINT('Ctrl Pts',(1.23736193587382,0.154029184025547,6.4457081776259));
#18617=CARTESIAN_POINT('Ctrl Pts',(1.23546770296442,0.109823313951739,6.44301969980809));
#18618=CARTESIAN_POINT('Ctrl Pts',(1.23463072691646,0.0816623168428676,
6.44131944048409));
#18619=CARTESIAN_POINT('Ctrl Pts',(1.23185162351298,-0.0857441899358567,
6.43128008385597));
#18620=CARTESIAN_POINT('Ctrl Pts',(1.23856693518712,-0.224994120066761,
6.42321786095159));
#18621=CARTESIAN_POINT('Ctrl Pts',(1.27574499601554,-0.552610559315221,
6.40449739916481));
#18622=CARTESIAN_POINT('Ctrl Pts',(1.31394717235191,-0.739552479198644,
6.39402076261361));
#18623=CARTESIAN_POINT('Ctrl Pts',(1.40408609072948,-1.04144522622785,6.37617311039338));
#18624=CARTESIAN_POINT('Ctrl Pts',(1.44663602769604,-1.15868369210127,6.36898760959665));
#18625=CARTESIAN_POINT('Ctrl Pts',(1.50246463102475,-1.28850868785228,6.36043218465812));
#18626=CARTESIAN_POINT('Ctrl Pts',(1.50918863123946,-1.30381549804905,6.3594137090073));
#18627=CARTESIAN_POINT('Ctrl Pts',(1.52015522525942,-1.32826197499614,6.35777033058758));
#18628=CARTESIAN_POINT('Ctrl Pts',(1.52432221555184,-1.33743548888224,6.35714983988396));
#18629=CARTESIAN_POINT('Ctrl Pts',(1.53181375854405,-1.35372461890982,6.35604098927605));
#18630=CARTESIAN_POINT('Ctrl Pts',(1.53512139198103,-1.3608478156862,6.3555536647527));
#18631=CARTESIAN_POINT('Ctrl Pts',(1.54230522728327,-1.37617176337293,6.35449998020553));
#18632=CARTESIAN_POINT('Ctrl Pts',(1.54618995698475,-1.38436812459012,6.35393312129449));
#18633=CARTESIAN_POINT('Ctrl Pts',(1.55712532754275,-1.40719112675114,6.35234576693081));
#18634=CARTESIAN_POINT('Ctrl Pts',(1.56425187325645,-1.42178080794705,6.3513207800823));
#18635=CARTESIAN_POINT('Ctrl Pts',(1.60765590912273,-1.5089620726903,6.34513690373842));
#18636=CARTESIAN_POINT('Ctrl Pts',(1.64655157937313,-1.58021020495437,6.33983699319324));
#18637=CARTESIAN_POINT('Ctrl Pts',(1.77114349345315,-1.78926284956254,6.32369506924111));
#18638=CARTESIAN_POINT('Ctrl Pts',(1.86459801223715,-1.92214392848086,6.31264122068349));
#18639=CARTESIAN_POINT('Ctrl Pts',(2.10164730026644,-2.21029724533973,6.28748151720168));
#18640=CARTESIAN_POINT('Ctrl Pts',(2.25132255145439,-2.35965197640766,6.27353937786568));
#18641=CARTESIAN_POINT('Ctrl Pts',(2.43575032279125,-2.51068998829175,6.25852989158309));
#18642=CARTESIAN_POINT('Ctrl Pts',(2.45717403514613,-2.52778320121041,6.25681518979986));
#18643=CARTESIAN_POINT('Ctrl Pts',(2.49263972149303,-2.55534700863238,6.25402276402041));
#18644=CARTESIAN_POINT('Ctrl Pts',(2.50655328009757,-2.56597982791365,6.25293864562728));
#18645=CARTESIAN_POINT('Ctrl Pts',(2.53172271028672,-2.58489150091124,6.25099757115393));
#18646=CARTESIAN_POINT('Ctrl Pts',(2.54294698154918,-2.59321149316611,6.25013901723904));
#18647=CARTESIAN_POINT('Ctrl Pts',(2.56700222314939,-2.61080121868161,6.24831382898448));
#18648=CARTESIAN_POINT('Ctrl Pts',(2.57984813343294,-2.62004996978445,6.24734802131185));
#18649=CARTESIAN_POINT('Ctrl Pts',(2.61482102242391,-2.64484045058727,6.24474213980746));
#18650=CARTESIAN_POINT('Ctrl Pts',(2.63707660440195,-2.66019917779934,6.24310906360733));
#18651=CARTESIAN_POINT('Ctrl Pts',(2.75799428501011,-2.74141789366567,6.23436648895444));
#18652=CARTESIAN_POINT('Ctrl Pts',(2.86004805611365,-2.80207657323799,6.2274535142884));
#18653=CARTESIAN_POINT('Ctrl Pts',(3.10274555887014,-2.92875656313907,6.21180223373956));
#18654=CARTESIAN_POINT('Ctrl Pts',(3.24527478284619,-2.99051716569644,6.20318165744625));
#18655=CARTESIAN_POINT('Ctrl Pts',(3.55137655637161,-3.09766789410364,6.18502229334651));
#18656=CARTESIAN_POINT('Ctrl Pts',(3.71518931338,-3.14089623823361,6.17549649820751));
#18657=CARTESIAN_POINT('Ctrl Pts',(3.90811462294718,-3.17587000544165,6.16374261435684));
#18658=CARTESIAN_POINT('Ctrl Pts',(3.93467356102573,-3.18034152761911,6.16211279383551));
#18659=CARTESIAN_POINT('Ctrl Pts',(3.9714816246255,-3.18606515979188,6.15983395863119));
#18660=CARTESIAN_POINT('Ctrl Pts',(3.98168622306138,-3.18760180494331,6.15920005256082));
#18661=CARTESIAN_POINT('Ctrl Pts',(3.99922168109147,-3.19015628634111,6.15810683660689));
#18662=CARTESIAN_POINT('Ctrl Pts',(4.00654906450147,-3.19119794004161,6.15764885108599));
#18663=CARTESIAN_POINT('Ctrl Pts',(4.02189312839014,-3.19332534020925,6.1566872203085));
#18664=CARTESIAN_POINT('Ctrl Pts',(4.02991036223953,-3.19440614853321,6.15618329067231));
#18665=CARTESIAN_POINT('Ctrl Pts',(4.04956404157137,-3.19698036744667,6.15494445306365));
#18666=CARTESIAN_POINT('Ctrl Pts',(4.06120467115549,-3.19844043525146,6.15420771293067));
#18667=CARTESIAN_POINT('Ctrl Pts',(4.10355507725739,-3.20351766479161,6.15151710531463));
#18668=CARTESIAN_POINT('Ctrl Pts',(4.13430744436685,-3.20675621774022,6.14954381136009));
#18669=CARTESIAN_POINT('Ctrl Pts',(4.21168338884739,-3.21378054377743,6.14453768907915));
#18670=CARTESIAN_POINT('Ctrl Pts',(4.25835073874192,-3.21699457562839,6.14148101275596));
#18671=CARTESIAN_POINT('Ctrl Pts',(4.63899007278846,-3.23489622157584,6.11632907114974));
#18672=CARTESIAN_POINT('Ctrl Pts',(4.97335016979985,-3.19855892402255,6.09313818176793));
#18673=CARTESIAN_POINT('Ctrl Pts',(5.35944158697716,-3.09435751119089,6.06738422899522));
#18674=CARTESIAN_POINT('Ctrl Pts',(5.42214657120999,-3.07536595252416,6.06322431739818));
#18675=CARTESIAN_POINT('Ctrl Pts',(5.50607932307142,-3.04712442341133,6.05768399963668));
#18676=CARTESIAN_POINT('Ctrl Pts',(5.5278466031188,-3.03953930103551,6.05624968716785));
#18677=CARTESIAN_POINT('Ctrl Pts',(5.56360313648351,-3.02664757856896,6.05389730155039));
#18678=CARTESIAN_POINT('Ctrl Pts',(5.57763986775712,-3.02147604017148,6.05297479163161));
#18679=CARTESIAN_POINT('Ctrl Pts',(5.6049523350546,-3.01119679654915,6.05118146066393));
#18680=CARTESIAN_POINT('Ctrl Pts',(5.61823124665056,-3.00609857019894,6.05031034840215));
#18681=CARTESIAN_POINT('Ctrl Pts',(5.64850016095526,-2.99424677950658,6.04832623648522));
#18682=CARTESIAN_POINT('Ctrl Pts',(5.66546741554319,-2.98743617863443,6.04721517666254));
#18683=CARTESIAN_POINT('Ctrl Pts',(5.72111869065572,-2.96454615671034,6.04357396356449));
#18684=CARTESIAN_POINT('Ctrl Pts',(5.75954817542988,-2.94785645329155,6.04106438575535));
#18685=CARTESIAN_POINT('Ctrl Pts',(5.84987264037354,-2.90651742284235,6.03516910679155));
#18686=CARTESIAN_POINT('Ctrl Pts',(5.90145610767507,-2.88122023594089,6.03180506668112));
#18687=CARTESIAN_POINT('Ctrl Pts',(6.09515758979043,-2.77971514464306,6.0191377611272));
#18688=CARTESIAN_POINT('Ctrl Pts',(6.23216579202492,-2.69425727127677,6.01011764512194));
#18689=CARTESIAN_POINT('Ctrl Pts',(6.5241172185557,-2.48017341526836,5.98987538747658));
#18690=CARTESIAN_POINT('Ctrl Pts',(6.67455803008167,-2.34659092720768,5.97870083864261));
#18691=CARTESIAN_POINT('Ctrl Pts',(6.82946475245728,-2.18075583845231,5.96508718217023));
#18692=CARTESIAN_POINT('Ctrl Pts',(6.84711913849459,-2.16138767641669,5.96350047187086));
#18693=CARTESIAN_POINT('Ctrl Pts',(6.87132121489615,-2.13417692134579,5.96127214354097));
#18694=CARTESIAN_POINT('Ctrl Pts',(6.87807130262276,-2.12651466823914,5.96064476501514));
#18695=CARTESIAN_POINT('Ctrl Pts',(6.88963211702837,-2.11326517144869,5.95955980615747));
#18696=CARTESIAN_POINT('Ctrl Pts',(6.89446034277903,-2.107693205832,5.95910350506069));
#18697=CARTESIAN_POINT('Ctrl Pts',(6.90456386884837,-2.0959521660517,5.95814181889217));
#18698=CARTESIAN_POINT('Ctrl Pts',(6.90983502322842,-2.08977968254442,5.95763612757738));
#18699=CARTESIAN_POINT('Ctrl Pts',(6.92275618613006,-2.07453283187,5.95638686010046));
#18700=CARTESIAN_POINT('Ctrl Pts',(6.93037944362659,-2.0654360467395,5.95564138266314));
#18701=CARTESIAN_POINT('Ctrl Pts',(6.95827833931186,-2.03176843041808,5.95288255568935));
#18702=CARTESIAN_POINT('Ctrl Pts',(6.97823884415019,-2.00694035881856,5.95084850390347));
#18703=CARTESIAN_POINT('Ctrl Pts',(7.12604202740783,-1.81740725256396,5.93534996911446));
#18704=CARTESIAN_POINT('Ctrl Pts',(7.23798981984625,-1.64095086079407,5.92111854117941));
#18705=CARTESIAN_POINT('Ctrl Pts',(7.3803369854828,-1.35960586758362,5.89982885787792));
#18706=CARTESIAN_POINT('Ctrl Pts',(7.42380131093422,-1.26193249485502,5.89266166909107));
#18707=CARTESIAN_POINT('Ctrl Pts',(7.5054964708819,-1.05065314499286,5.87772243499036));
#18708=CARTESIAN_POINT('Ctrl Pts',(7.54241008394384,-0.936703797256036,
5.86999377157115));
#18709=CARTESIAN_POINT('Ctrl Pts',(7.57999296240963,-0.794034710956098,
5.86072126571752));
#18710=CARTESIAN_POINT('Ctrl Pts',(7.58673492621508,-0.767025668870155,
5.85898303790319));
#18711=CARTESIAN_POINT('Ctrl Pts',(7.59683758733288,-0.724199320161467,
5.85625322076193));
#18712=CARTESIAN_POINT('Ctrl Pts',(7.60043052570603,-0.708438748581375,
5.85525422157419));
#18713=CARTESIAN_POINT('Ctrl Pts',(7.60690043584985,-0.679039225560604,
5.85340090817654));
#18714=CARTESIAN_POINT('Ctrl Pts',(7.60980778331766,-0.665407416356418,
5.85254564053503));
#18715=CARTESIAN_POINT('Ctrl Pts',(7.61532821032295,-0.638674543218368,
5.85087618797657));
#18716=CARTESIAN_POINT('Ctrl Pts',(7.61794844533969,-0.625575262008021,
5.85006179090648));
#18717=CARTESIAN_POINT('Ctrl Pts',(7.62365658001599,-0.596086570610306,
5.84823643786342));
#18718=CARTESIAN_POINT('Ctrl Pts',(7.62669887465297,-0.57968864502427,5.84722693839758));
#18719=CARTESIAN_POINT('Ctrl Pts',(7.63404904468938,-0.538281766951424,
5.84469127655215));
#18720=CARTESIAN_POINT('Ctrl Pts',(7.63818912353459,-0.513243910511666,
5.84317035789014));
#18721=CARTESIAN_POINT('Ctrl Pts',(7.66678699860404,-0.326623731942253,
5.8319200181707));
#18722=CARTESIAN_POINT('Ctrl Pts',(7.67921910621361,-0.163436536696629,
5.82257685402867));
#18723=CARTESIAN_POINT('Ctrl Pts',(7.67921910621823,-9.10799213826863E-11,
5.81337971654115));
#18724=CARTESIAN_POINT('',(2.58258872576669,-2.62522787511044,25.0015778214036));
#18725=CARTESIAN_POINT('Ctrl Pts',(2.62314711761431,-2.65048072028474,25.));
#18726=CARTESIAN_POINT('Ctrl Pts',(2.61007479697457,-2.64143867267145,25.0005259404679));
#18727=CARTESIAN_POINT('Ctrl Pts',(2.59706937140007,-2.63229991316527,25.0010518809357));
#18728=CARTESIAN_POINT('Ctrl Pts',(2.58413226446108,-2.62306544209225,25.0015778214036));
#18729=CARTESIAN_POINT('Ctrl Pts',(2.58086696126463,-2.62738283509833,25.));
#18730=CARTESIAN_POINT('Ctrl Pts',(2.51895112061205,-2.59291341350604,25.));
#18731=CARTESIAN_POINT('Ctrl Pts',(2.45838415266209,-2.55633419485211,25.));
#18732=CARTESIAN_POINT('Ctrl Pts',(2.39928606905601,-2.51767449708445,25.));
#18733=CARTESIAN_POINT('Ctrl Pts',(2.31388248279346,-2.46180674923679,25.));
#18734=CARTESIAN_POINT('Ctrl Pts',(2.23154518283394,-2.40159687600469,25.));
#18735=CARTESIAN_POINT('Ctrl Pts',(2.15235473238406,-2.3374492656266,25.));
#18736=CARTESIAN_POINT('Ctrl Pts',(2.0706327165835,-2.27125098036485,24.9999999999999));
#18737=CARTESIAN_POINT('Ctrl Pts',(1.99226142380909,-2.20085884507454,24.9999999999999));
#18738=CARTESIAN_POINT('Ctrl Pts',(1.91734952117858,-2.12666429431228,24.9999999999999));
#18739=CARTESIAN_POINT('Ctrl Pts',(1.84247962307714,-2.05251134584625,24.9999999999999));
#18740=CARTESIAN_POINT('Ctrl Pts',(1.77106477073175,-1.97455960018966,24.9999999999999));
#18741=CARTESIAN_POINT('Ctrl Pts',(1.70324071360077,-1.8931555210592,24.9999999999999));
#18742=CARTESIAN_POINT('Ctrl Pts',(1.68150575299838,-1.86706869394182,24.9999999999999));
#18743=CARTESIAN_POINT('Ctrl Pts',(1.66013978843617,-1.84062702848735,24.9999999999999));
#18744=CARTESIAN_POINT('Ctrl Pts',(1.63914800286785,-1.81384113209172,24.9999999999999));
#18745=CARTESIAN_POINT('Ctrl Pts',(1.62919321696348,-1.80113864601651,24.9999999999999));
#18746=CARTESIAN_POINT('Ctrl Pts',(1.6193222495985,-1.78835819280448,24.9999999999999));
#18747=CARTESIAN_POINT('Ctrl Pts',(1.60954519814125,-1.77551370299918,24.9999999999999));
#18748=CARTESIAN_POINT('Ctrl Pts',(1.54334451395581,-1.6885433094361,24.9999999999999));
#18749=CARTESIAN_POINT('Ctrl Pts',(1.48133988628096,-1.59850518093636,24.9999999999999));
#18750=CARTESIAN_POINT('Ctrl Pts',(1.42362862152261,-1.50583407628298,24.9999999999999));
#18751=CARTESIAN_POINT('Ctrl Pts',(1.36499217356469,-1.41167733880783,24.9999999999999));
#18752=CARTESIAN_POINT('Ctrl Pts',(1.31078728724555,-1.31480192020701,24.9999999999999));
#18753=CARTESIAN_POINT('Ctrl Pts',(1.26114495505595,-1.21561705804934,24.9999999999999));
#18754=CARTESIAN_POINT('Ctrl Pts',(1.2111258651229,-1.11567943784823,24.9999999999999));
#18755=CARTESIAN_POINT('Ctrl Pts',(1.16573827734856,-1.01339645096499,25.));
#18756=CARTESIAN_POINT('Ctrl Pts',(1.12515384086073,-0.909149914337555,
25.));
#18757=CARTESIAN_POINT('Ctrl Pts',(1.08984118530872,-0.818444649980424,
25.));
#18758=CARTESIAN_POINT('Ctrl Pts',(1.05816525700407,-0.726251929697037,
24.9999999999999));
#18759=CARTESIAN_POINT('Ctrl Pts',(1.03026717068748,-0.632807598513387,
24.9999999999999));
#18760=CARTESIAN_POINT('Ctrl Pts',(1.0257979958373,-0.617838146842787,25.));
#18761=CARTESIAN_POINT('Ctrl Pts',(1.02142649755212,-0.602838610619727,
24.9999999999999));
#18762=CARTESIAN_POINT('Ctrl Pts',(1.01715621625056,-0.587820957022462,
24.9999999999999));
#18763=CARTESIAN_POINT('Ctrl Pts',(0.985703770959921,-0.477209525408138,
24.9999999999999));
#18764=CARTESIAN_POINT('Ctrl Pts',(0.959689578443777,-0.365453494535015,
24.9999999999999));
#18765=CARTESIAN_POINT('Ctrl Pts',(0.93924671117129,-0.252983170698471,
25.));
#18766=CARTESIAN_POINT('Ctrl Pts',(0.918870509582298,-0.140879620803699,
25.));
#18767=CARTESIAN_POINT('Ctrl Pts',(0.904028866916014,-0.0280655825087988,
25.));
#18768=CARTESIAN_POINT('Ctrl Pts',(0.894895231890315,0.0850624586136153,
25.));
#18769=CARTESIAN_POINT('Ctrl Pts',(0.886340822666338,0.191016282665257,
25.));
#18770=CARTESIAN_POINT('Ctrl Pts',(0.882793434187598,0.297246370144321,
25.));
#18771=CARTESIAN_POINT('Ctrl Pts',(0.884434707218777,0.403440761847383,
25.));
#18772=CARTESIAN_POINT('Ctrl Pts',(0.885637860676345,0.481287742286474,
25.));
#18773=CARTESIAN_POINT('Ctrl Pts',(0.889630094231931,0.559115847805151,
25.));
#18774=CARTESIAN_POINT('Ctrl Pts',(0.896336380065494,0.636828108152072,
25.));
#18775=CARTESIAN_POINT('Ctrl Pts',(0.898266237245346,0.659191241384986,
25.));
#18776=CARTESIAN_POINT('Ctrl Pts',(0.900420926006865,0.681544782497862,
25.));
#18777=CARTESIAN_POINT('Ctrl Pts',(0.902798848013211,0.703886417160758,
25.));
#18778=CARTESIAN_POINT('Ctrl Pts',(0.90514245462499,0.725905643432187,25.));
#18779=CARTESIAN_POINT('Ctrl Pts',(0.907703616726005,0.747918192377519,
25.));
#18780=CARTESIAN_POINT('Ctrl Pts',(0.910476780326299,0.769891749104374,
25.));
#18781=CARTESIAN_POINT('Ctrl Pts',(0.924563913848233,0.881513157783874,
25.));
#18782=CARTESIAN_POINT('Ctrl Pts',(0.944128901058905,0.992259489847555,
25.));
#18783=CARTESIAN_POINT('Ctrl Pts',(0.968856780713456,1.10183615184693,25.));
#18784=CARTESIAN_POINT('Ctrl Pts',(0.994044372209712,1.21344993509565,25.));
#18785=CARTESIAN_POINT('Ctrl Pts',(1.0245887260487,1.32385079384828,25.));
#18786=CARTESIAN_POINT('Ctrl Pts',(1.06021172903275,1.43273620380258,25.));
#18787=CARTESIAN_POINT('Ctrl Pts',(1.09656535472959,1.54385483799233,25.));
#18788=CARTESIAN_POINT('Ctrl Pts',(1.13820822442275,1.65339597590095,25.));
#18789=CARTESIAN_POINT('Ctrl Pts',(1.18489932594814,1.76103650943336,25.));
#18790=CARTESIAN_POINT('Ctrl Pts',(1.22344065551518,1.84988875626652,25.));
#18791=CARTESIAN_POINT('Ctrl Pts',(1.26542279926213,1.93744616388805,25.));
#18792=CARTESIAN_POINT('Ctrl Pts',(1.31073612832854,2.02352051946335,25.));
#18793=CARTESIAN_POINT('Ctrl Pts',(1.32070254197158,2.04245209322752,25.));
#18794=CARTESIAN_POINT('Ctrl Pts',(1.33083018884825,2.0613118898127,25.));
#18795=CARTESIAN_POINT('Ctrl Pts',(1.34111804451498,2.08009784379795,25.));
#18796=CARTESIAN_POINT('Ctrl Pts',(1.35034361641663,2.09694403360137,25.));
#18797=CARTESIAN_POINT('Ctrl Pts',(1.35969385765356,2.11372318424346,25.));
#18798=CARTESIAN_POINT('Ctrl Pts',(1.36916492541488,2.13042919793156,25.));
#18799=CARTESIAN_POINT('Ctrl Pts',(1.42850674181193,2.2351022107311,25.));
#18800=CARTESIAN_POINT('Ctrl Pts',(1.49262023288704,2.33696417549315,25.));
#18801=CARTESIAN_POINT('Ctrl Pts',(1.56123071821778,2.43568204796968,25.));
#18802=CARTESIAN_POINT('Ctrl Pts',(1.63034991151195,2.53513185766571,25.));
#18803=CARTESIAN_POINT('Ctrl Pts',(1.70403334168491,2.63139161134848,25.));
#18804=CARTESIAN_POINT('Ctrl Pts',(1.78205063137054,2.72410643348489,25.));
#18805=CARTESIAN_POINT('Ctrl Pts',(1.81727298375025,2.76596425947796,25.));
#18806=CARTESIAN_POINT('Ctrl Pts',(1.85337933069364,2.80709927385776,25.));
#18807=CARTESIAN_POINT('Ctrl Pts',(1.89035154083729,2.84747716338277,25.));
#18808=CARTESIAN_POINT('Ctrl Pts',(1.90419446776442,2.8625952256245,25.));
#18809=CARTESIAN_POINT('Ctrl Pts',(1.91816074658184,2.87760919409566,25.));
#18810=CARTESIAN_POINT('Ctrl Pts',(1.93224291148647,2.89251028361586,25.));
#18811=CARTESIAN_POINT('Ctrl Pts',(2.01699807592679,2.98219424209656,25.));
#18812=CARTESIAN_POINT('Ctrl Pts',(2.10584503538453,3.06768542877611,25.));
#18813=CARTESIAN_POINT('Ctrl Pts',(2.19852420314815,3.14863093007319,25.));
#18814=CARTESIAN_POINT('Ctrl Pts',(2.29008964672514,3.22860371047983,25.));
#18815=CARTESIAN_POINT('Ctrl Pts',(2.38539622530628,3.30414016034279,25.));
#18816=CARTESIAN_POINT('Ctrl Pts',(2.48423691550681,3.37487470703325,25.));
#18817=CARTESIAN_POINT('Ctrl Pts',(2.55686352024641,3.42684935384624,25.));
#18818=CARTESIAN_POINT('Ctrl Pts',(2.63139913748095,3.47623095136753,25.));
#18819=CARTESIAN_POINT('Ctrl Pts',(2.70777463088727,3.52286199445091,25.));
#18820=CARTESIAN_POINT('Ctrl Pts',(2.17296269996979,-3.20554048108048,-0.411765747138983));
#18821=CARTESIAN_POINT('Ctrl Pts',(1.10598262521586,-2.44554835076675,-0.345549597099719));
#18822=CARTESIAN_POINT('Ctrl Pts',(-0.190085171851759,0.209786400507346,
-0.213161407923235));
#18823=CARTESIAN_POINT('Ctrl Pts',(2.11904905146237,4.02596493684606,-0.0146011796095345));
#18824=CARTESIAN_POINT('Ctrl Pts',(6.57036830017086,4.14281137096193,0.183914937802122));
#18825=CARTESIAN_POINT('Ctrl Pts',(9.08469850437939,0.471525498888313,0.382431055213778));
#18826=CARTESIAN_POINT('Ctrl Pts',(7.36116941620609,-3.63455711911314,0.580947172625436));
#18827=CARTESIAN_POINT('Ctrl Pts',(2.97726580402431,-4.41062931823268,0.77946329003709));
#18828=CARTESIAN_POINT('Ctrl Pts',(-0.0518523842630756,-1.14834011450979,
0.977979407448747));
#18829=CARTESIAN_POINT('Ctrl Pts',(1.04758148582589,3.16599895701937,1.1764955248604));
#18830=CARTESIAN_POINT('Ctrl Pts',(5.26885307852876,4.58075644304919,1.37501164227206));
#18831=CARTESIAN_POINT('Ctrl Pts',(8.74613631193873,1.80065901519612,1.57352775968371));
#18832=CARTESIAN_POINT('Ctrl Pts',(8.2950356860829,-2.62850749839492,1.77204387709537));
#18833=CARTESIAN_POINT('Ctrl Pts',(4.32864266632258,-4.6505056552148,1.97055999450703));
#18834=CARTESIAN_POINT('Ctrl Pts',(0.479313869061077,-2.41367545883394,
2.16907611191868));
#18835=CARTESIAN_POINT('Ctrl Pts',(0.272186515624751,2.03356129066451,2.36759222933034));
#18836=CARTESIAN_POINT('Ctrl Pts',(3.89694643539194,4.61849687019083,2.56610834674199));
#18837=CARTESIAN_POINT('Ctrl Pts',(8.03410612006349,2.97390317522259,2.76462446415365));
#18838=CARTESIAN_POINT('Ctrl Pts',(8.89493411795877,-1.39413568050936,2.9631405815653));
#18839=CARTESIAN_POINT('Ctrl Pts',(5.69110016326603,-4.48545097223521,3.16165669897696));
#18840=CARTESIAN_POINT('Ctrl Pts',(1.35661463604595,-3.46907591290164,3.36017281638862));
#18841=CARTESIAN_POINT('Ctrl Pts',(-0.139083166427389,0.724213049156903,
3.55868893380027));
#18842=CARTESIAN_POINT('Ctrl Pts',(2.57373840321099,4.25428138787658,3.75720505121192));
#18843=CARTESIAN_POINT('Ctrl Pts',(7.01072892820446,3.88835980295648,3.95572116862359));
#18844=CARTESIAN_POINT('Ctrl Pts',(9.10857690015422,-0.0384477492421469,
4.15423728603523));
#18845=CARTESIAN_POINT('Ctrl Pts',(6.94611304441007,-3.93004557143118,4.3527534034469));
#18846=CARTESIAN_POINT('Ctrl Pts',(2.50368062941278,-4.22258242327136,4.55126952085854));
#18847=CARTESIAN_POINT('Ctrl Pts',(-0.15042524517621,-0.648158610486061,
4.74978563827021));
#18848=CARTESIAN_POINT('Ctrl Pts',(1.41437509517098,3.51983652671062,4.94830175568186));
#18849=CARTESIAN_POINT('Ctrl Pts',(5.76506726388787,4.46443232806813,5.14681787309352));
#18850=CARTESIAN_POINT('Ctrl Pts',(8.91737013208296,1.32058592540232,5.34533399050517));
#18851=CARTESIAN_POINT('Ctrl Pts',(7.98446469607637,-3.03262794728552,5.54385010791683));
#18852=CARTESIAN_POINT('Ctrl Pts',(3.82068800849579,-4.60861883268182,5.74236622532849));
#18853=CARTESIAN_POINT('Ctrl Pts',(0.239147556357015,-1.9641242562649,5.94088234274014));
#18854=CARTESIAN_POINT('Ctrl Pts',(0.519749957626067,2.47907795239849,6.13939846015179));
#18855=CARTESIAN_POINT('Ctrl Pts',(4.40552487083362,4.65198772933701,6.33791457756345));
#18856=CARTESIAN_POINT('Ctrl Pts',(8.33795354574623,2.56469563392857,6.53643069497511));
#18857=CARTESIAN_POINT('Ctrl Pts',(8.71579260460107,-1.87129593734266,6.73494681238676));
#18858=CARTESIAN_POINT('Ctrl Pts',(5.19302422456139,-4.59359028502123,6.93346292979842));
#18859=CARTESIAN_POINT('Ctrl Pts',(0.995732677906764,-3.10916202902842,
7.13197904721008));
#18860=CARTESIAN_POINT('Ctrl Pts',(-0.0322822778871914,1.22257767061497,
7.33049516462173));
#18861=CARTESIAN_POINT('Ctrl Pts',(3.05041589877745,4.43470399540276,7.52901128203338));
#18862=CARTESIAN_POINT('Ctrl Pts',(7.42075085684839,3.58561275821527,7.72752739944505));
#18863=CARTESIAN_POINT('Ctrl Pts',(9.07645297431008,-0.547114437358846,
7.9260435168567));
#18864=CARTESIAN_POINT('Ctrl Pts',(6.5012617467849,-4.17880463841992,8.12455963426836));
#18865=CARTESIAN_POINT('Ctrl Pts',(2.05348831510913,-3.98362504090881,8.32307575168001));
#18866=CARTESIAN_POINT('Ctrl Pts',(-0.193681017610346,-0.140317407516647,
8.52159186909167));
#18867=CARTESIAN_POINT('Ctrl Pts',(1.81766867783776,3.83149023855917,8.72010798650331));
#18868=CARTESIAN_POINT('Ctrl Pts',(6.24558161029013,4.2944920068349,8.91862410391498));
#18869=CARTESIAN_POINT('Ctrl Pts',(9.03505934404192,0.824679685151172,9.11714022132663));
#18870=CARTESIAN_POINT('Ctrl Pts',(7.6315512320161,-3.40035860512303,9.31565633873829));
#18871=CARTESIAN_POINT('Ctrl Pts',(3.32036330565075,-4.51141316650472,9.51417245614994));
#18872=CARTESIAN_POINT('Ctrl Pts',(0.0495994604212725,-1.49100136617927,
9.71268857356161));
#18873=CARTESIAN_POINT('Ctrl Pts',(0.814563009263402,2.89484112343983,9.91120469097325));
#18874=CARTESIAN_POINT('Ctrl Pts',(4.91471488529713,4.62964317792977,10.1097208083849));
#18875=CARTESIAN_POINT('Ctrl Pts',(8.59521399360942,2.1247060752228,10.3082369257966));
#18876=CARTESIAN_POINT('Ctrl Pts',(8.48552926132444,-2.32599643497811,10.5067530432082));
#18877=CARTESIAN_POINT('Ctrl Pts',(4.68610787984395,-4.64659565516981,10.7052691606199));
#18878=CARTESIAN_POINT('Ctrl Pts',(0.676387677669684,-2.71193096197848,
10.9037852780315));
#18879=CARTESIAN_POINT('Ctrl Pts',(0.128394142987057,1.70626851979591,11.1023013954432));
#18880=CARTESIAN_POINT('Ctrl Pts',(3.54396933091606,4.56189974780998,11.3008175128549));
#18881=CARTESIAN_POINT('Ctrl Pts',(7.79519445548059,3.23982996331418,11.4993336302665));
#18882=CARTESIAN_POINT('Ctrl Pts',(8.98887841448097,-1.04921447348414,11.6978497476782));
#18883=CARTESIAN_POINT('Ctrl Pts',(6.03186814454124,-4.3774082536412,11.8963658650898));
#18884=CARTESIAN_POINT('Ctrl Pts',(1.63213740257258,-3.69685482224785,12.0948819825015));
#18885=CARTESIAN_POINT('Ctrl Pts',(-0.181124089683036,0.369207933724872,
12.2933980999131));
#18886=CARTESIAN_POINT('Ctrl Pts',(2.2526340504912,4.09715708707193,12.4919142173248));
#18887=CARTESIAN_POINT('Ctrl Pts',(6.70462241331237,4.07300771627025,12.6904303347364));
#18888=CARTESIAN_POINT('Ctrl Pts',(9.09779474190718,0.318875355730261,12.8889464521481));
#18889=CARTESIAN_POINT('Ctrl Pts',(7.24052934071316,-3.72727698993507,13.0874625695597));
#18890=CARTESIAN_POINT('Ctrl Pts',(2.83367453520978,-4.36005996854408,13.2859786869714));
#18891=CARTESIAN_POINT('Ctrl Pts',(-0.0870558709899348,-0.999982965095223,
13.4844948043831));
#18892=CARTESIAN_POINT('Ctrl Pts',(1.1530874699283,3.2758594160949,13.6830109217947));
#18893=CARTESIAN_POINT('Ctrl Pts',(5.41840487637927,4.55173205747878,13.8815270392064));
#18894=CARTESIAN_POINT('Ctrl Pts',(8.80279980247531,1.65921506374814,14.080043156618));
#18895=CARTESIAN_POINT('Ctrl Pts',(8.20690775291552,-2.75277952374592,14.2785592740297));
#18896=CARTESIAN_POINT('Ctrl Pts',(4.17643533161801,-4.64383098681233,14.4770753914414));
#18897=CARTESIAN_POINT('Ctrl Pts',(0.402412514292184,-2.28215036718792,
14.675591508853));
#18898=CARTESIAN_POINT('Ctrl Pts',(0.341017607518878,2.16948014760412,14.8741076262646));
#18899=CARTESIAN_POINT('Ctrl Pts',(4.04847489906614,4.63434201110855,15.0726237436763));
#18900=CARTESIAN_POINT('Ctrl Pts',(8.12956552465056,2.85516161537223,15.271139861088));
#18901=CARTESIAN_POINT('Ctrl Pts',(8.84690431993714,-1.53872147678918,15.4696559784996));
#18902=CARTESIAN_POINT('Ctrl Pts',(5.54356606143321,-4.52347271009317,15.6681720959113));
#18903=CARTESIAN_POINT('Ctrl Pts',(1.24468509012015,-3.36571368106855,15.8666882133229));
#18904=CARTESIAN_POINT('Ctrl Pts',(-0.112905173860372,0.874301914415817,
16.0652043307346));
#18905=CARTESIAN_POINT('Ctrl Pts',(2.71405060913991,4.31364844766405,16.2637204481462));
#18906=CARTESIAN_POINT('Ctrl Pts',(7.1366801074503,3.80263778683562,16.4622365655579));
#18907=CARTESIAN_POINT('Ctrl Pts',(9.10482335385156,-0.190756225336315,
16.6607526829696));
#18908=CARTESIAN_POINT('Ctrl Pts',(6.81609220134375,-4.00945931491334,16.8592688003812));
#18909=CARTESIAN_POINT('Ctrl Pts',(2.36646310311057,-4.15637583189606,17.0577849177929));
#18910=CARTESIAN_POINT('Ctrl Pts',(-0.16917825360623,-0.496962424679848,
17.2563010352045));
#18911=CARTESIAN_POINT('Ctrl Pts',(1.53126025266144,3.61755971783011,17.4548171526162));
#18912=CARTESIAN_POINT('Ctrl Pts',(5.91054938364417,4.41918948403437,17.6533332700278));
#18913=CARTESIAN_POINT('Ctrl Pts',(8.95821945609951,1.17380958265607,17.8518493874395));
#18914=CARTESIAN_POINT('Ctrl Pts',(7.88327219050615,-3.14652280629029,18.0503655048511));
#18915=CARTESIAN_POINT('Ctrl Pts',(3.67012384502666,-4.58532946245115,18.2488816222628));
#18916=CARTESIAN_POINT('Ctrl Pts',(0.177095531876928,-1.82497861910485,
18.4473977396744));
#18917=CARTESIAN_POINT('Ctrl Pts',(0.603036135785551,2.60665292882547,18.6459138570862));
#18918=CARTESIAN_POINT('Ctrl Pts',(4.55787735396168,4.65116130836808,18.8444299744978));
#18919=CARTESIAN_POINT('Ctrl Pts',(8.41985082781949,2.43622463611074,19.0429460919094));
#18920=CARTESIAN_POINT('Ctrl Pts',(8.65223471259592,-2.00976021586402,19.2414622093211));
#18921=CARTESIAN_POINT('Ctrl Pts',(5.04221626688697,-4.61524489208584,19.4399783267328));
#18922=CARTESIAN_POINT('Ctrl Pts',(0.895781713701428,-2.99417608693739,
19.6384944441444));
#18923=CARTESIAN_POINT('Ctrl Pts',(0.0101569427980723,1.36890222246852,
19.8370105615561));
#18924=CARTESIAN_POINT('Ctrl Pts',(3.1963802739596,4.47836591752857,20.0355266789677));
#18925=CARTESIAN_POINT('Ctrl Pts',(7.53656898706393,3.48662728959027,20.2340427963793));
#18926=CARTESIAN_POINT('Ctrl Pts',(9.05606082131957,-0.698098281184544,
20.432558913791));
#18927=CARTESIAN_POINT('Ctrl Pts',(6.36333405195284,-4.24351873734398,20.6310750312027));
#18928=CARTESIAN_POINT('Ctrl Pts',(1.9243366462227,-3.90280543100934,20.8295911486144));
#18929=CARTESIAN_POINT('Ctrl Pts',(-0.195782035254683,0.0120228054752082,
21.028107266026));
#18930=CARTESIAN_POINT('Ctrl Pts',(1.94454241477252,3.91584087042925,21.2266233834376));
#18931=CARTESIAN_POINT('Ctrl Pts',(6.38524148680512,4.23360619038166,21.4251395008493));
#18932=CARTESIAN_POINT('Ctrl Pts',(9.05960761710739,0.674315805600993,21.623655618261));
#18933=CARTESIAN_POINT('Ctrl Pts',(7.5185068390623,-3.50250076674849,21.8221717356726));
#18934=CARTESIAN_POINT('Ctrl Pts',(3.17325057532877,-4.47179261159471,22.0206878530843));
#18935=CARTESIAN_POINT('Ctrl Pts',(0.0031406198327811,-1.34590405051051,
22.2192039704959));
#18936=CARTESIAN_POINT('Ctrl Pts',(0.911305739869395,3.01254206724522,22.4177200879076));
#18937=CARTESIAN_POINT('Ctrl Pts',(5.06606104496655,4.6121513544261,22.6162362053192));
#18938=CARTESIAN_POINT('Ctrl Pts',(8.66256938155685,1.98805571626367,22.8147523227309));
#18939=CARTESIAN_POINT('Ctrl Pts',(8.4072000996685,-2.45669335535235,23.0132684401425));
#18940=CARTESIAN_POINT('Ctrl Pts',(4.53384760969594,-4.65159218721967,23.2117845575542));
#18941=CARTESIAN_POINT('Ctrl Pts',(0.589592923617338,-2.58676106216746,
23.4103006749659));
#18942=CARTESIAN_POINT('Ctrl Pts',(0.186627431348294,1.84718698340797,23.6088167923775));
#18943=CARTESIAN_POINT('Ctrl Pts',(3.69375302108596,4.58911293885384,23.8073329097892));
#18944=CARTESIAN_POINT('Ctrl Pts',(7.89964467060016,3.12919021086655,24.0058490272008));
#18945=CARTESIAN_POINT('Ctrl Pts',(8.95179466357075,-1.19786968887199,24.2043651446125));
#18946=CARTESIAN_POINT('Ctrl Pts',(5.88826072308503,-4.42509080397621,24.4028812620241));
#18947=CARTESIAN_POINT('Ctrl Pts',(1.51149918181804,-3.60542346049212,24.6013973794358));
#18948=CARTESIAN_POINT('Ctrl Pts',(-0.164376056275096,0.527120914407128,
24.7999134968474));
#18949=CARTESIAN_POINT('Ctrl Pts',(1.53399129555416,2.94325066577138,24.9322575751219));
#18950=CARTESIAN_POINT('Ctrl Pts',(2.70656526709436,3.52529833870864,24.9984296142591));
#18951=CARTESIAN_POINT('Ctrl Pts',(2.31196529717974,-3.01041142380583,-0.273445981108207));
#18952=CARTESIAN_POINT('Ctrl Pts',(1.30993489857133,-2.29668186568531,-0.207229831068943));
#18953=CARTESIAN_POINT('Ctrl Pts',(0.0927619053280601,0.197016191301887,
-0.0748416418924601));
#18954=CARTESIAN_POINT('Ctrl Pts',(2.26133350378215,3.78089464452436,0.123718586421241));
#18955=CARTESIAN_POINT('Ctrl Pts',(6.44169010710979,3.89062835157607,0.322234703832897));
#18956=CARTESIAN_POINT('Ctrl Pts',(8.80296690727615,0.442822593209179,0.520750821244553));
#18957=CARTESIAN_POINT('Ctrl Pts',(7.18435323294509,-3.41331277406459,0.719266938656211));
#18958=CARTESIAN_POINT('Ctrl Pts',(3.06730851213489,-4.14214356803415,0.917783056067867));
#18959=CARTESIAN_POINT('Ctrl Pts',(0.222580126422941,-1.07843785456408,
1.11629917347952));
#18960=CARTESIAN_POINT('Ctrl Pts',(1.25508877879203,2.97327688863128,1.31481529089117));
#18961=CARTESIAN_POINT('Ctrl Pts',(5.21940128729496,4.30191464036023,1.51333140830283));
#18962=CARTESIAN_POINT('Ctrl Pts',(8.48501382017349,1.69104851481962,1.71184752571448));
#18963=CARTESIAN_POINT('Ctrl Pts',(8.06137278822348,-2.46850384433775,1.91036364312614));
#18964=CARTESIAN_POINT('Ctrl Pts',(4.33642377308406,-4.36741804808325,2.1088797605378));
#18965=CARTESIAN_POINT('Ctrl Pts',(0.721412996069988,-2.26674915432179,
2.30739587794946));
#18966=CARTESIAN_POINT('Ctrl Pts',(0.526893989166935,1.90977346146706,2.50591199536111));
#18967=CARTESIAN_POINT('Ctrl Pts',(3.93100594327419,4.33735771577206,2.70442811277276));
#18968=CARTESIAN_POINT('Ctrl Pts',(7.81632664047099,2.79287444498747,2.90294423018442));
#18969=CARTESIAN_POINT('Ctrl Pts',(8.62475394129306,-1.30927124574203,3.10146034759608));
#18970=CARTESIAN_POINT('Ctrl Pts',(5.61594516345689,-4.21241064570382,3.29997646500774));
#18971=CARTESIAN_POINT('Ctrl Pts',(1.54531032840212,-3.25790481196126,3.49849258241939));
#18972=CARTESIAN_POINT('Ctrl Pts',(0.140659294449413,0.680128436785933,
3.69700869983105));
#18973=CARTESIAN_POINT('Ctrl Pts',(2.68834480713824,3.99531291703776,3.8955248172427));
#18974=CARTESIAN_POINT('Ctrl Pts',(6.85524491106594,3.65166587031902,4.09404093465435));
#18975=CARTESIAN_POINT('Ctrl Pts',(8.82539176693615,-0.0361073410931478,
4.29255705206602));
#18976=CARTESIAN_POINT('Ctrl Pts',(6.79456235351217,-3.69081412452673,4.49107316947766));
#18977=CARTESIAN_POINT('Ctrl Pts',(2.62255162068078,-3.96554354562172,4.68958928688933));
#18978=CARTESIAN_POINT('Ctrl Pts',(0.130007635661538,-0.608703617053558,
4.88810540430098));
#18979=CARTESIAN_POINT('Ctrl Pts',(1.59955476768487,3.30557550356288,5.08662152171263));
#18980=CARTESIAN_POINT('Ctrl Pts',(5.68540970649173,4.19267145760527,5.28513763912429));
#18981=CARTESIAN_POINT('Ctrl Pts',(8.64582422058695,1.24019864338394,5.48365375653594));
#18982=CARTESIAN_POINT('Ctrl Pts',(7.76970701088062,-2.84802449713069,5.68216987394761));
#18983=CARTESIAN_POINT('Ctrl Pts',(3.85938955257665,-4.32808097846753,5.88068599135924));
#18984=CARTESIAN_POINT('Ctrl Pts',(0.495866191827503,-1.844563228489,6.07920210877092));
#18985=CARTESIAN_POINT('Ctrl Pts',(0.759387641428115,2.32817043879295,6.27771822618256));
#18986=CARTESIAN_POINT('Ctrl Pts',(4.40862597053364,4.36880990474354,6.47623434359423));
#18987=CARTESIAN_POINT('Ctrl Pts',(8.10167813322798,2.40857636349708,6.67475046100588));
#18988=CARTESIAN_POINT('Ctrl Pts',(8.45651720821394,-1.75738559545474,6.87326657841754));
#18989=CARTESIAN_POINT('Ctrl Pts',(5.14818832037566,-4.31396725511023,7.0717826958292));
#18990=CARTESIAN_POINT('Ctrl Pts',(1.20639613410644,-2.9198997628929,7.27029881324085));
#18991=CARTESIAN_POINT('Ctrl Pts',(0.240958952754043,1.14815638979818,7.4688149306525));
#18992=CARTESIAN_POINT('Ctrl Pts',(3.13600578243834,4.16475276096279,7.66733104806417));
#18993=CARTESIAN_POINT('Ctrl Pts',(7.24030780616454,3.36734777563528,7.86584716547581));
#18994=CARTESIAN_POINT('Ctrl Pts',(8.79522330270695,-0.513810248872322,
8.06436328288747));
#18995=CARTESIAN_POINT('Ctrl Pts',(6.37679023796107,-3.92443062116999,8.26287940029913));
#18996=CARTESIAN_POINT('Ctrl Pts',(2.1997636091463,-3.74113208118609,8.46139551771078));
#18997=CARTESIAN_POINT('Ctrl Pts',(0.089384947459713,-0.131775945129999,
8.65991163512245));
#18998=CARTESIAN_POINT('Ctrl Pts',(1.97829888761515,3.5982580948319,8.8584277525341));
#18999=CARTESIAN_POINT('Ctrl Pts',(6.13667397417128,4.03307581767334,9.05694386994575));
#19000=CARTESIAN_POINT('Ctrl Pts',(8.75634940354159,0.774479423926291,9.2554599873574));
#19001=CARTESIAN_POINT('Ctrl Pts',(7.43827624901926,-3.19337049409171,9.45397610476906));
#19002=CARTESIAN_POINT('Ctrl Pts',(3.38952083310589,-4.23679245796831,9.65249222218073));
#19003=CARTESIAN_POINT('Ctrl Pts',(0.317856350200649,-1.40024048117564,
9.85100833959237));
#19004=CARTESIAN_POINT('Ctrl Pts',(1.03625470449417,2.71862509287945,10.049524457004));
#19005=CARTESIAN_POINT('Ctrl Pts',(4.88682034851015,4.34782552060827,10.2480405744157));
#19006=CARTESIAN_POINT('Ctrl Pts',(8.34327851098385,1.99537004097493,10.4465566918273));
#19007=CARTESIAN_POINT('Ctrl Pts',(8.24027055552775,-2.18440736622039,10.645072809239));
#19008=CARTESIAN_POINT('Ctrl Pts',(4.67212920832948,-4.36374605926514,10.8435889266506));
#19009=CARTESIAN_POINT('Ctrl Pts',(0.906490441907856,-2.54684911848653,
11.0421050440623));
#19010=CARTESIAN_POINT('Ctrl Pts',(0.391854608507251,1.60240379879482,11.2406211614739));
#19011=CARTESIAN_POINT('Ctrl Pts',(3.59951541494433,4.28420579809219,11.4391372788856));
#19012=CARTESIAN_POINT('Ctrl Pts',(7.59195811086242,3.04261362173219,11.6376533962972));
#19013=CARTESIAN_POINT('Ctrl Pts',(8.71297961965247,-0.98534623276214,11.8361695137089));
#19014=CARTESIAN_POINT('Ctrl Pts',(5.93596976765481,-4.11094475056566,12.0346856311206));
#19015=CARTESIAN_POINT('Ctrl Pts',(1.80406135300024,-3.47181826426207,12.2332017485322));
#19016=CARTESIAN_POINT('Ctrl Pts',(0.101177504597399,0.346733347466743,
12.4317178659439));
#19017=CARTESIAN_POINT('Ctrl Pts',(2.38678685852808,3.84775315515312,12.6302339833555));
#19018=CARTESIAN_POINT('Ctrl Pts',(6.56777184536255,3.82507381537617,12.8287501007672));
#19019=CARTESIAN_POINT('Ctrl Pts',(8.81526594492522,0.29946463609684,13.0272662181788));
#19020=CARTESIAN_POINT('Ctrl Pts',(7.07105681270762,-3.5003885604986,13.2257823355905));
#19021=CARTESIAN_POINT('Ctrl Pts',(2.93245799361878,-4.09465249784007,13.4242984530022));
#19022=CARTESIAN_POINT('Ctrl Pts',(0.189519561683291,-0.939111566208993,
13.6228145704138));
#19023=CARTESIAN_POINT('Ctrl Pts',(1.35417235664619,3.07644987396012,13.8213306878255));
#19024=CARTESIAN_POINT('Ctrl Pts',(5.3598495029257,4.27465703983832,14.0198468052371));
#19025=CARTESIAN_POINT('Ctrl Pts',(8.53822806601778,1.55821460123144,14.2183629226488));
#19026=CARTESIAN_POINT('Ctrl Pts',(7.97860941701375,-2.58521112879858,14.4168790400604));
#19027=CARTESIAN_POINT('Ctrl Pts',(4.19348166959603,-4.36114968300486,14.6153951574721));
#19028=CARTESIAN_POINT('Ctrl Pts',(0.649192814085452,-2.14323031537866,
14.8139112748837));
#19029=CARTESIAN_POINT('Ctrl Pts',(0.59153516483578,2.03741860650786,15.0124273922954));
#19030=CARTESIAN_POINT('Ctrl Pts',(4.07331050026509,4.35223832436584,15.2109435097071));
#19031=CARTESIAN_POINT('Ctrl Pts',(7.9059751985768,2.68136097312093,15.4094596271187));
#19032=CARTESIAN_POINT('Ctrl Pts',(8.57964783407003,-1.44505575241412,15.6079757445304));
#19033=CARTESIAN_POINT('Ctrl Pts',(5.47739182177246,-4.24811790776339,15.806491861942));
#19034=CARTESIAN_POINT('Ctrl Pts',(1.44019420657955,-3.16083449095397,16.0050079793537));
#19035=CARTESIAN_POINT('Ctrl Pts',(0.165243768843413,0.821081027223728,
16.2035240967653));
#19036=CARTESIAN_POINT('Ctrl Pts',(2.82011586731386,4.05106615928717,16.402040214177));
#19037=CARTESIAN_POINT('Ctrl Pts',(6.97352913523386,3.57116196212476,16.6005563315886));
#19038=CARTESIAN_POINT('Ctrl Pts',(8.82186670813997,-0.17914442924803,16.7990724490003));
#19039=CARTESIAN_POINT('Ctrl Pts',(6.67245619587356,-3.76539376000376,16.997588566412));
#19040=CARTESIAN_POINT('Ctrl Pts',(2.49368685944485,-3.90336711073225,17.1961046838236));
#19041=CARTESIAN_POINT('Ctrl Pts',(0.112396168534027,-0.466711111367439,
17.3946208012353));
#19042=CARTESIAN_POINT('Ctrl Pts',(1.70932484092508,3.39735004600064,17.5931369186469));
#19043=CARTESIAN_POINT('Ctrl Pts',(5.82203597524696,4.15018265569229,17.7916530360586));
#19044=CARTESIAN_POINT('Ctrl Pts',(8.68418694674809,1.10235693414467,17.9901691534703));
#19045=CARTESIAN_POINT('Ctrl Pts',(7.67467433961344,-2.9549862986379,18.1886852708819));
#19046=CARTESIAN_POINT('Ctrl Pts',(3.71799059648846,-4.30620928893205,18.3872013882936));
#19047=CARTESIAN_POINT('Ctrl Pts',(0.437591425226463,-1.7138877251997,18.5857175057052));
#19048=CARTESIAN_POINT('Ctrl Pts',(0.837603987051035,2.44797961565228,18.7842336231169));
#19049=CARTESIAN_POINT('Ctrl Pts',(4.55170438690705,4.36803379003202,18.9827497405285));
#19050=CARTESIAN_POINT('Ctrl Pts',(8.17859012825258,2.28792570825151,19.1812658579402));
#19051=CARTESIAN_POINT('Ctrl Pts',(8.39682823991214,-1.88742121606535,19.3797819753518));
#19052=CARTESIAN_POINT('Ctrl Pts',(5.0065604104293,-4.33430369349561,19.5782980927635));
#19053=CARTESIAN_POINT('Ctrl Pts',(1.11252942855707,-2.81191329518458,19.7768142101752));
#19054=CARTESIAN_POINT('Ctrl Pts',(0.280814794700937,1.28557380975688,19.9753303275868));
#19055=CARTESIAN_POINT('Ctrl Pts',(3.27308495055695,4.20575687553525,20.1738464449984));
#19056=CARTESIAN_POINT('Ctrl Pts',(7.34907580467911,3.27438779359847,20.3723625624101));
#19057=CARTESIAN_POINT('Ctrl Pts',(8.77607246974106,-0.65560333835151,20.5708786798217));
#19058=CARTESIAN_POINT('Ctrl Pts',(6.24725853788356,-3.98520541525919,20.7693947972334));
#19059=CARTESIAN_POINT('Ctrl Pts',(2.07847371693811,-3.66523215780504,20.9679109146451));
#19060=CARTESIAN_POINT('Ctrl Pts',(0.0874118238771355,0.0112909480203034,
21.1664270320568));
#19061=CARTESIAN_POINT('Ctrl Pts',(2.09744951113826,3.6774740982752,21.3649431494684));
#19062=CARTESIAN_POINT('Ctrl Pts',(6.26783241381338,3.97589626917586,21.56345926688));
#19063=CARTESIAN_POINT('Ctrl Pts',(8.77940336342984,0.633268559987037,21.7619753842917));
#19064=CARTESIAN_POINT('Ctrl Pts',(7.33211314362288,-3.28929501353682,21.9604915017033));
#19065=CARTESIAN_POINT('Ctrl Pts',(3.25136321302202,-4.1995837027451,22.159007619115));
#19066=CARTESIAN_POINT('Ctrl Pts',(0.274225572405194,-1.26397559254583,
22.3575237365266));
#19067=CARTESIAN_POINT('Ctrl Pts',(1.12710846943813,2.82916129353447,22.5560398539383));
#19068=CARTESIAN_POINT('Ctrl Pts',(5.0289536987851,4.33139846700858,22.75455597135));
#19069=CARTESIAN_POINT('Ctrl Pts',(8.40653381239982,1.86703792222437,22.9530720887616));
#19070=CARTESIAN_POINT('Ctrl Pts',(8.1667094807393,-2.30714844669435,23.1515882061733));
#19071=CARTESIAN_POINT('Ctrl Pts',(4.52913739170739,-4.36843844023836,23.3501043235849));
#19072=CARTESIAN_POINT('Ctrl Pts',(0.824979095953012,-2.42929861537115,
23.5486204409966));
#19073=CARTESIAN_POINT('Ctrl Pts',(0.44654309475883,1.73474421227166,23.7471365584082));
#19074=CARTESIAN_POINT('Ctrl Pts',(3.74018140704413,4.30976245591016,23.9456526758199));
#19075=CARTESIAN_POINT('Ctrl Pts',(7.69005018696339,2.93870878051704,24.1441687932315));
#19076=CARTESIAN_POINT('Ctrl Pts',(8.67815324699032,-1.12495244308866,24.3426849106432));
#19077=CARTESIAN_POINT('Ctrl Pts',(5.80110407974766,-4.15572474791461,24.5412010280549));
#19078=CARTESIAN_POINT('Ctrl Pts',(1.69076667459873,-3.38595255220879,24.7397171454665));
#19079=CARTESIAN_POINT('Ctrl Pts',(0.116906044416222,0.495033780363739,
24.9382332628782));
#19080=CARTESIAN_POINT('Ctrl Pts',(1.71188963858453,2.76408782845127,25.0705773411526));
#19081=CARTESIAN_POINT('Ctrl Pts',(2.81308617627174,3.31070484176046,25.1367493802898));
#19082=CARTESIAN_POINT('Ctrl Pts',(2.45096789438968,-2.81528236653118,-0.135126215077433));
#19083=CARTESIAN_POINT('Ctrl Pts',(1.5138871719268,-2.14781538060387,-0.0689100650381678));
#19084=CARTESIAN_POINT('Ctrl Pts',(0.375608982507884,0.184245982096433,
0.0634781241383155));
#19085=CARTESIAN_POINT('Ctrl Pts',(2.40361795610193,3.53582435220265,0.262038352452016));
#19086=CARTESIAN_POINT('Ctrl Pts',(6.31301191404873,3.63844533219021,0.460554469863673));
#19087=CARTESIAN_POINT('Ctrl Pts',(8.52123531017291,0.41411968753004,0.659070587275328));
#19088=CARTESIAN_POINT('Ctrl Pts',(7.00753704968407,-3.19206842901602,0.857586704686986));
#19089=CARTESIAN_POINT('Ctrl Pts',(3.15735122024546,-3.87365781783563,1.05610282209864));
#19090=CARTESIAN_POINT('Ctrl Pts',(0.497012637108953,-1.00853559461836,
1.25461893951029));
#19091=CARTESIAN_POINT('Ctrl Pts',(1.46259607175817,2.78055482024318,1.45313505692195));
#19092=CARTESIAN_POINT('Ctrl Pts',(5.16994949606116,4.02307283767128,1.6516511743336));
#19093=CARTESIAN_POINT('Ctrl Pts',(8.22389132840824,1.58143801444312,1.85016729174526));
#19094=CARTESIAN_POINT('Ctrl Pts',(7.82770989036406,-2.30850019028058,2.04868340915692));
#19095=CARTESIAN_POINT('Ctrl Pts',(4.34420487984554,-4.08433044095169,2.24719952656857));
#19096=CARTESIAN_POINT('Ctrl Pts',(0.963512123078899,-2.11982284980964,
2.44571564398023));
#19097=CARTESIAN_POINT('Ctrl Pts',(0.781601462709117,1.78598563226962,2.64423176139188));
#19098=CARTESIAN_POINT('Ctrl Pts',(3.96506545115642,4.05621856135326,2.84274787880354));
#19099=CARTESIAN_POINT('Ctrl Pts',(7.59854716087849,2.61184571475234,3.0412639962152));
#19100=CARTESIAN_POINT('Ctrl Pts',(8.35457376462735,-1.22440681097471,3.23978011362686));
#19101=CARTESIAN_POINT('Ctrl Pts',(5.54079016364776,-3.93937031917242,3.43829623103851));
#19102=CARTESIAN_POINT('Ctrl Pts',(1.7340060207583,-3.04673371102089,3.63681234845017));
#19103=CARTESIAN_POINT('Ctrl Pts',(0.420401755326215,0.636043824414959,
3.83532846586182));
#19104=CARTESIAN_POINT('Ctrl Pts',(2.8029512110655,3.73634444619894,4.03384458327349));
#19105=CARTESIAN_POINT('Ctrl Pts',(6.6997608939274,3.41497193768155,4.23236070068513));
#19106=CARTESIAN_POINT('Ctrl Pts',(8.54220663371807,-0.0337669329441494,
4.4308768180968));
#19107=CARTESIAN_POINT('Ctrl Pts',(6.64301166261426,-3.45158267762228,4.62939293550844));
#19108=CARTESIAN_POINT('Ctrl Pts',(2.74142261194879,-3.70850466797209,4.82790905292011));
#19109=CARTESIAN_POINT('Ctrl Pts',(0.410440516499291,-0.569248623621048,
5.02642517033176));
#19110=CARTESIAN_POINT('Ctrl Pts',(1.78473444019877,3.09131448041513,5.22494128774342));
#19111=CARTESIAN_POINT('Ctrl Pts',(5.60575214909559,3.92091058714242,5.42345740515506));
#19112=CARTESIAN_POINT('Ctrl Pts',(8.37427830909092,1.15981136136555,5.62197352256674));
#19113=CARTESIAN_POINT('Ctrl Pts',(7.55494932568486,-2.66342104697584,5.82048963997839));
#19114=CARTESIAN_POINT('Ctrl Pts',(3.89809109665752,-4.04754312425325,6.01900575739004));
#19115=CARTESIAN_POINT('Ctrl Pts',(0.752584827297987,-1.72500220071308,
6.21752187480171));
#19116=CARTESIAN_POINT('Ctrl Pts',(0.999025325230166,2.17726292518741,6.41603799221334));
#19117=CARTESIAN_POINT('Ctrl Pts',(4.41172707023364,4.08563208015006,6.61455410962502));
#19118=CARTESIAN_POINT('Ctrl Pts',(7.86540272070975,2.25245709306557,6.81307022703666));
#19119=CARTESIAN_POINT('Ctrl Pts',(8.1972418118268,-1.64347525356681,7.01158634444832));
#19120=CARTESIAN_POINT('Ctrl Pts',(5.10335241618994,-4.03434422519923,7.21010246185998));
#19121=CARTESIAN_POINT('Ctrl Pts',(1.4170595903061,-2.73063749675737,7.40861857927163));
#19122=CARTESIAN_POINT('Ctrl Pts',(0.514200183395272,1.07373510898141,7.60713469668328));
#19123=CARTESIAN_POINT('Ctrl Pts',(3.22159566609925,3.89480152652282,7.80565081409495));
#19124=CARTESIAN_POINT('Ctrl Pts',(7.05986475548066,3.14908279305528,8.0041669315066));
#19125=CARTESIAN_POINT('Ctrl Pts',(8.51399363110384,-0.480506060385796,
8.20268304891826));
#19126=CARTESIAN_POINT('Ctrl Pts',(6.25231872913724,-3.67005660392007,8.40119916632992));
#19127=CARTESIAN_POINT('Ctrl Pts',(2.34603890318347,-3.49863912146337,8.59971528374156));
#19128=CARTESIAN_POINT('Ctrl Pts',(0.372450912529775,-0.123234482743352,
8.79823140115322));
#19129=CARTESIAN_POINT('Ctrl Pts',(2.13892909739252,3.36502595110463,8.99674751856487));
#19130=CARTESIAN_POINT('Ctrl Pts',(6.02776633805246,3.77165962851178,9.19526363597655));
#19131=CARTESIAN_POINT('Ctrl Pts',(8.47763946304124,0.72427916270141,9.39377975338818));
#19132=CARTESIAN_POINT('Ctrl Pts',(7.24500126602242,-2.98638238306039,9.59229587079984));
#19133=CARTESIAN_POINT('Ctrl Pts',(3.45867836056103,-3.9621717494319,9.79081198821151));
#19134=CARTESIAN_POINT('Ctrl Pts',(0.586113239980029,-1.30947959617202,
9.98932810562315));
#19135=CARTESIAN_POINT('Ctrl Pts',(1.25794639972494,2.54240906231909,10.1878442230349));
#19136=CARTESIAN_POINT('Ctrl Pts',(4.85892581172318,4.06600786328675,10.3863603404465));
#19137=CARTESIAN_POINT('Ctrl Pts',(8.09134302835829,1.86603400672705,10.5848764578582));
#19138=CARTESIAN_POINT('Ctrl Pts',(7.99501184973105,-2.04281829746266,10.7833925752698));
#19139=CARTESIAN_POINT('Ctrl Pts',(4.658150536815,-4.08089646336047,10.9819086926815));
#19140=CARTESIAN_POINT('Ctrl Pts',(1.13659320614603,-2.38176727499459,11.1804248100931));
#19141=CARTESIAN_POINT('Ctrl Pts',(0.655315074027438,1.49853907779376,11.3789409275048));
#19142=CARTESIAN_POINT('Ctrl Pts',(3.6550614989726,4.00651184837438,11.5774570449165));
#19143=CARTESIAN_POINT('Ctrl Pts',(7.38872176624422,2.84539728015019,11.7759731623281));
#19144=CARTESIAN_POINT('Ctrl Pts',(8.43708082482397,-0.921477992040132,
11.9744892797398));
#19145=CARTESIAN_POINT('Ctrl Pts',(5.84007139076835,-3.84448124749012,12.1730053971514));
#19146=CARTESIAN_POINT('Ctrl Pts',(1.97598530342792,-3.24678170627628,12.3715215145631));
#19147=CARTESIAN_POINT('Ctrl Pts',(0.383479098877827,0.324258761208613,
12.5700376319747));
#19148=CARTESIAN_POINT('Ctrl Pts',(2.52093966656498,3.59834922323431,12.7685537493864));
#19149=CARTESIAN_POINT('Ctrl Pts',(6.43092127741269,3.5771399144821,12.967069866798));
#19150=CARTESIAN_POINT('Ctrl Pts',(8.53273714794332,0.280053916463419,13.1655859842097));
#19151=CARTESIAN_POINT('Ctrl Pts',(6.90158428470204,-3.27350013106212,13.3641021016213));
#19152=CARTESIAN_POINT('Ctrl Pts',(3.0312414520278,-3.82924502713605,13.562618219033));
#19153=CARTESIAN_POINT('Ctrl Pts',(0.466094994356506,-0.878240167322765,
13.7611343364446));
#19154=CARTESIAN_POINT('Ctrl Pts',(1.55525724336407,2.87704033182534,13.9596504538563));
#19155=CARTESIAN_POINT('Ctrl Pts',(5.30129412947213,3.99758202219787,14.1581665712679));
#19156=CARTESIAN_POINT('Ctrl Pts',(8.27365632956023,1.45721413871475,14.3566826886797));
#19157=CARTESIAN_POINT('Ctrl Pts',(7.75031108111198,-2.41764273385123,14.5551988060912));
#19158=CARTESIAN_POINT('Ctrl Pts',(4.21052800757405,-4.07846837919741,14.753714923503));
#19159=CARTESIAN_POINT('Ctrl Pts',(0.895973113878727,-2.00431026356939,
14.9522310409146));
#19160=CARTESIAN_POINT('Ctrl Pts',(0.842052722152676,1.9053570654116,15.1507471583263));
#19161=CARTESIAN_POINT('Ctrl Pts',(4.09814610146403,4.07013463762311,15.3492632757379));
#19162=CARTESIAN_POINT('Ctrl Pts',(7.682384872503,2.50756033086961,15.5477793931496));
#19163=CARTESIAN_POINT('Ctrl Pts',(8.31239134820293,-1.35139002803904,15.7462955105612));
#19164=CARTESIAN_POINT('Ctrl Pts',(5.41121758211169,-3.97276310543362,15.9448116279729));
#19165=CARTESIAN_POINT('Ctrl Pts',(1.63570332303896,-2.95595530083938,16.1433277453845));
#19166=CARTESIAN_POINT('Ctrl Pts',(0.443392711547191,0.767860140031627,
16.3418438627962));
#19167=CARTESIAN_POINT('Ctrl Pts',(2.92618112548781,3.7884838709103,16.5403599802078));
#19168=CARTESIAN_POINT('Ctrl Pts',(6.8103781630174,3.33968613741389,16.7388760976195));
#19169=CARTESIAN_POINT('Ctrl Pts',(8.5389100624284,-0.167532633159739,16.9373922150311));
#19170=CARTESIAN_POINT('Ctrl Pts',(6.52882019040339,-3.5213282050942,17.1359083324428));
#19171=CARTESIAN_POINT('Ctrl Pts',(2.62091061577914,-3.65035838956845,17.3344244498544));
#19172=CARTESIAN_POINT('Ctrl Pts',(0.393970590674286,-0.43645979805503,
17.5329405672661));
#19173=CARTESIAN_POINT('Ctrl Pts',(1.88738942918871,3.17714037417117,17.7314566846778));
#19174=CARTESIAN_POINT('Ctrl Pts',(5.73352256684974,3.8811758273502,17.9299728020894));
#19175=CARTESIAN_POINT('Ctrl Pts',(8.41015443739666,1.03090428563328,18.1284889195011));
#19176=CARTESIAN_POINT('Ctrl Pts',(7.46607648872073,-2.76344979098553,18.3270050369127));
#19177=CARTESIAN_POINT('Ctrl Pts',(3.76585734795025,-4.02708911541293,18.5255211543244));
#19178=CARTESIAN_POINT('Ctrl Pts',(0.698087318576006,-1.60279683129456,
18.724037271736));
#19179=CARTESIAN_POINT('Ctrl Pts',(1.07217183831651,2.28930630247911,18.9225533891477));
#19180=CARTESIAN_POINT('Ctrl Pts',(4.54553141985243,4.08490627169594,19.1210695065593));
#19181=CARTESIAN_POINT('Ctrl Pts',(7.93732942868568,2.13962678039228,19.319585623971));
#19182=CARTESIAN_POINT('Ctrl Pts',(8.14142176722837,-1.76508221626667,19.5181017413827));
#19183=CARTESIAN_POINT('Ctrl Pts',(4.97090455397163,-4.05336249490537,19.7166178587943));
#19184=CARTESIAN_POINT('Ctrl Pts',(1.3292771434127,-2.62965050343175,19.915133976206));
#19185=CARTESIAN_POINT('Ctrl Pts',(0.551472646603815,1.20224539704524,20.1136500936177));
#19186=CARTESIAN_POINT('Ctrl Pts',(3.3497896271543,3.93314783354192,20.3121662110293));
#19187=CARTESIAN_POINT('Ctrl Pts',(7.16158262229433,3.06214829760668,20.510682328441));
#19188=CARTESIAN_POINT('Ctrl Pts',(8.49608411816253,-0.613108395518473,
20.7091984458526));
#19189=CARTESIAN_POINT('Ctrl Pts',(6.13118302381429,-3.72689209317441,20.9077145632643));
#19190=CARTESIAN_POINT('Ctrl Pts',(2.23261078765349,-3.42765888460072,21.1062306806759));
#19191=CARTESIAN_POINT('Ctrl Pts',(0.370605683008962,0.0105590905653954,
21.3047467980876));
#19192=CARTESIAN_POINT('Ctrl Pts',(2.250356607504,3.43910732612115,21.5032629154992));
#19193=CARTESIAN_POINT('Ctrl Pts',(6.15042334082164,3.71818634797007,21.7017790329109));
#19194=CARTESIAN_POINT('Ctrl Pts',(8.49919910975228,0.592221314373082,21.9002951503225));
#19195=CARTESIAN_POINT('Ctrl Pts',(7.14571944818345,-3.07608926032515,22.0988112677342));
#19196=CARTESIAN_POINT('Ctrl Pts',(3.32947585071529,-3.92737479389549,22.2973273851459));
#19197=CARTESIAN_POINT('Ctrl Pts',(0.545310524977601,-1.18204713458114,
22.4958435025575));
#19198=CARTESIAN_POINT('Ctrl Pts',(1.34291119900688,2.64578051982372,22.6943596199692));
#19199=CARTESIAN_POINT('Ctrl Pts',(4.99184635260365,4.05064557959106,22.8928757373808));
#19200=CARTESIAN_POINT('Ctrl Pts',(8.15049824324278,1.74602012818506,23.0913918547925));
#19201=CARTESIAN_POINT('Ctrl Pts',(7.92621886181009,-2.15760353803636,23.2899079722041));
#19202=CARTESIAN_POINT('Ctrl Pts',(4.52442717371885,-4.08528469325705,23.4884240896158));
#19203=CARTESIAN_POINT('Ctrl Pts',(1.06036526828869,-2.27183616857484,23.6869402070274));
#19204=CARTESIAN_POINT('Ctrl Pts',(0.706458758169362,1.62230144113535,23.8854563244391));
#19205=CARTESIAN_POINT('Ctrl Pts',(3.78660979300229,4.03041197296648,24.0839724418507));
#19206=CARTESIAN_POINT('Ctrl Pts',(7.48045570332662,2.74822735016753,24.2824885592624));
#19207=CARTESIAN_POINT('Ctrl Pts',(8.40451183040988,-1.05203519730533,24.481004676674));
#19208=CARTESIAN_POINT('Ctrl Pts',(5.71394743641032,-3.88635869185298,24.6795207940858));
#19209=CARTESIAN_POINT('Ctrl Pts',(1.87003416737941,-3.16648164392546,24.8780369114974));
#19210=CARTESIAN_POINT('Ctrl Pts',(0.398188145107553,0.462946646320358,
25.076553028909));
#19211=CARTESIAN_POINT('Ctrl Pts',(1.88978798161488,2.58492499113116,25.2088971071835));
#19212=CARTESIAN_POINT('Ctrl Pts',(2.91960708544911,3.09611134481228,25.2750691463207));
#19213=CARTESIAN_POINT('Ctrl Pts',(2.58997049159961,-2.62015330925654,0.00319355095334283));
#19214=CARTESIAN_POINT('Ctrl Pts',(1.71783944528228,-1.99894889552244,0.0694097009926075));
#19215=CARTESIAN_POINT('Ctrl Pts',(0.65845605968771,0.171475772890977,0.20179789016909));
#19216=CARTESIAN_POINT('Ctrl Pts',(2.5459024084217,3.29075405988094,0.400358118482792));
#19217=CARTESIAN_POINT('Ctrl Pts',(6.18433372098768,3.38626231280436,0.598874235894448));
#19218=CARTESIAN_POINT('Ctrl Pts',(8.23950371306965,0.385416781850904,0.797390353306103));
#19219=CARTESIAN_POINT('Ctrl Pts',(6.83072086642306,-2.97082408396747,0.995906470717762));
#19220=CARTESIAN_POINT('Ctrl Pts',(3.24739392835603,-3.60517206763711,1.19442258812942));
#19221=CARTESIAN_POINT('Ctrl Pts',(0.771445147794971,-0.938633334672633,
1.39293870554108));
#19222=CARTESIAN_POINT('Ctrl Pts',(1.6701033647243,2.58783275185508,1.59145482295273));
#19223=CARTESIAN_POINT('Ctrl Pts',(5.12049770482736,3.74423103498232,1.78997094036439));
#19224=CARTESIAN_POINT('Ctrl Pts',(7.96276883664299,1.47182751406662,1.98848705777604));
#19225=CARTESIAN_POINT('Ctrl Pts',(7.59404699250464,-2.14849653622342,2.1870031751877));
#19226=CARTESIAN_POINT('Ctrl Pts',(4.35198598660702,-3.80124283382013,2.38551929259936));
#19227=CARTESIAN_POINT('Ctrl Pts',(1.20561125008781,-1.97289654529749,2.58403541001101));
#19228=CARTESIAN_POINT('Ctrl Pts',(1.0363089362513,1.66219780307218,2.78255152742267));
#19229=CARTESIAN_POINT('Ctrl Pts',(3.99912495903867,3.77507940693446,2.98106764483432));
#19230=CARTESIAN_POINT('Ctrl Pts',(7.38076768128599,2.43081698451723,3.17958376224598));
#19231=CARTESIAN_POINT('Ctrl Pts',(8.08439358796167,-1.13954237620741,3.37809987965763));
#19232=CARTESIAN_POINT('Ctrl Pts',(5.4656351638386,-3.66632999264102,3.5766159970693));
#19233=CARTESIAN_POINT('Ctrl Pts',(1.92270171311447,-2.83556261008053,3.77513211448094));
#19234=CARTESIAN_POINT('Ctrl Pts',(0.700144216203009,0.591959212043988,
3.97364823189261));
#19235=CARTESIAN_POINT('Ctrl Pts',(2.91755761499276,3.47737597536012,4.17216434930425));
#19236=CARTESIAN_POINT('Ctrl Pts',(6.54427687678886,3.1782780050441,4.37068046671592));
#19237=CARTESIAN_POINT('Ctrl Pts',(8.2590215005,-0.0314265247951463,4.56919658412757));
#19238=CARTESIAN_POINT('Ctrl Pts',(6.49146097171637,-3.21235123071783,4.76771270153922));
#19239=CARTESIAN_POINT('Ctrl Pts',(2.86029360321679,-3.45146579032245,4.96622881895089));
#19240=CARTESIAN_POINT('Ctrl Pts',(0.690873397337037,-0.529793630188544,
5.16474493636253));
#19241=CARTESIAN_POINT('Ctrl Pts',(1.96991411271267,2.8770534572674,5.36326105377419));
#19242=CARTESIAN_POINT('Ctrl Pts',(5.52609459169944,3.64914971667956,5.56177717118585));
#19243=CARTESIAN_POINT('Ctrl Pts',(8.1027323975949,1.07942407934716,5.7602932885975));
#19244=CARTESIAN_POINT('Ctrl Pts',(7.34019164048911,-2.47881759682101,5.95880940600916));
#19245=CARTESIAN_POINT('Ctrl Pts',(3.93679264073839,-3.76700527003896,6.15732552342081));
#19246=CARTESIAN_POINT('Ctrl Pts',(1.00930346276847,-1.60544117293717,6.35584164083248));
#19247=CARTESIAN_POINT('Ctrl Pts',(1.23866300903221,2.02635541158186,6.55435775824412));
#19248=CARTESIAN_POINT('Ctrl Pts',(4.41482816993367,3.80245425555658,6.75287387565579));
#19249=CARTESIAN_POINT('Ctrl Pts',(7.6291273081915,2.09633782263408,6.95138999306744));
#19250=CARTESIAN_POINT('Ctrl Pts',(7.93796641543966,-1.5295649116789,7.14990611047909));
#19251=CARTESIAN_POINT('Ctrl Pts',(5.05851651200422,-3.75472119528823,7.34842222789076));
#19252=CARTESIAN_POINT('Ctrl Pts',(1.62772304650576,-2.54137523062185,7.5469383453024));
#19253=CARTESIAN_POINT('Ctrl Pts',(0.787441414036509,0.999313828164636,
7.74545446271406));
#19254=CARTESIAN_POINT('Ctrl Pts',(3.30718554976015,3.62485029208286,7.94397058012572));
#19255=CARTESIAN_POINT('Ctrl Pts',(6.8794217047968,2.93081781047529,8.14248669753737));
#19256=CARTESIAN_POINT('Ctrl Pts',(8.23276395950072,-0.447201871899268,
8.34100281494903));
#19257=CARTESIAN_POINT('Ctrl Pts',(6.12784722031342,-3.41568258667014,8.53951893236069));
#19258=CARTESIAN_POINT('Ctrl Pts',(2.49231419722064,-3.25614616174064,8.73803504977233));
#19259=CARTESIAN_POINT('Ctrl Pts',(0.655516877599837,-0.114693020356707,
8.93655116718401));
#19260=CARTESIAN_POINT('Ctrl Pts',(2.29955930716991,3.13179380737736,9.13506728459565));
#19261=CARTESIAN_POINT('Ctrl Pts',(5.9188587019336,3.51024343935022,9.33358340200731));
#19262=CARTESIAN_POINT('Ctrl Pts',(8.19892952254092,0.674078901476532,9.53209951941897));
#19263=CARTESIAN_POINT('Ctrl Pts',(7.05172628302556,-2.77939427202906,9.73061563683061));
#19264=CARTESIAN_POINT('Ctrl Pts',(3.52783588801619,-3.68755104089551,9.92913175424228));
#19265=CARTESIAN_POINT('Ctrl Pts',(0.854370129759403,-1.21871871116838,
10.1276478716539));
#19266=CARTESIAN_POINT('Ctrl Pts',(1.47963809495571,2.36619303175871,10.3261639890656));
#19267=CARTESIAN_POINT('Ctrl Pts',(4.83103127493619,3.78419020596524,10.5246801064772));
#19268=CARTESIAN_POINT('Ctrl Pts',(7.83940754573271,1.73669797247918,10.7231962238889));
#19269=CARTESIAN_POINT('Ctrl Pts',(7.74975314393437,-1.90122922870495,10.9217123413006));
#19270=CARTESIAN_POINT('Ctrl Pts',(4.64417186530054,-3.79804686745578,11.1202284587122));
#19271=CARTESIAN_POINT('Ctrl Pts',(1.36669597038421,-2.21668543150265,11.3187445761239));
#19272=CARTESIAN_POINT('Ctrl Pts',(0.91877553954763,1.39467435679268,11.5172606935355));
#19273=CARTESIAN_POINT('Ctrl Pts',(3.71060758300086,3.72881789865659,11.7157768109472));
#19274=CARTESIAN_POINT('Ctrl Pts',(7.18548542162604,2.64818093856821,11.9142929283589));
#19275=CARTESIAN_POINT('Ctrl Pts',(8.16118202999545,-0.857609751318129,
12.1128090457705));
#19276=CARTESIAN_POINT('Ctrl Pts',(5.74417301388192,-3.57801774441457,12.3113251631822));
#19277=CARTESIAN_POINT('Ctrl Pts',(2.14790925385559,-3.02174514829049,12.5098412805938));
#19278=CARTESIAN_POINT('Ctrl Pts',(0.665780693158256,0.301784174950485,
12.7083573980055));
#19279=CARTESIAN_POINT('Ctrl Pts',(2.65509247460188,3.34894529131551,12.9068735154171));
#19280=CARTESIAN_POINT('Ctrl Pts',(6.29407070946287,3.32920601358802,13.1053896328288));
#19281=CARTESIAN_POINT('Ctrl Pts',(8.25020835096136,0.260643196829997,13.3039057502404));
#19282=CARTESIAN_POINT('Ctrl Pts',(6.7321117566965,-3.04661170162563,13.5024218676521));
#19283=CARTESIAN_POINT('Ctrl Pts',(3.1300249104368,-3.56383755643203,13.7009379850637));
#19284=CARTESIAN_POINT('Ctrl Pts',(0.742670427029733,-0.817368768436538,
13.8994541024754));
#19285=CARTESIAN_POINT('Ctrl Pts',(1.75634213008195,2.67763078969056,14.0979702198871));
#19286=CARTESIAN_POINT('Ctrl Pts',(5.24273875601857,3.7205070045574,14.2964863372987));
#19287=CARTESIAN_POINT('Ctrl Pts',(8.0090845931027,1.35621367619806,14.4950024547104));
#19288=CARTESIAN_POINT('Ctrl Pts',(7.52201274521021,-2.25007433890389,14.693518572122));
#19289=CARTESIAN_POINT('Ctrl Pts',(4.22757434555207,-3.79578707538995,14.8920346895337));
#19290=CARTESIAN_POINT('Ctrl Pts',(1.14275341367199,-1.86539021176013,15.0905508069453));
#19291=CARTESIAN_POINT('Ctrl Pts',(1.09257027946957,1.77329552431533,15.289066924357));
#19292=CARTESIAN_POINT('Ctrl Pts',(4.12298170266298,3.78803095088039,15.4875830417686));
#19293=CARTESIAN_POINT('Ctrl Pts',(7.45879454642923,2.3337596886183,15.6860991591803));
#19294=CARTESIAN_POINT('Ctrl Pts',(8.04513486233581,-1.25772430366396,15.8846152765919));
#19295=CARTESIAN_POINT('Ctrl Pts',(5.34504334245093,-3.69740830310385,16.0831313940036));
#19296=CARTESIAN_POINT('Ctrl Pts',(1.83121243949837,-2.75107611072479,16.2816475114153));
#19297=CARTESIAN_POINT('Ctrl Pts',(0.721541654250978,0.714639252839528,
16.4801636288269));
#19298=CARTESIAN_POINT('Ctrl Pts',(3.03224638366176,3.52590158253341,16.6786797462386));
#19299=CARTESIAN_POINT('Ctrl Pts',(6.64722719080097,3.10821031270302,16.8771958636502));
#19300=CARTESIAN_POINT('Ctrl Pts',(8.25595341671681,-0.155920837071448,
17.0757119810619));
#19301=CARTESIAN_POINT('Ctrl Pts',(6.38518418493321,-3.27726265018464,17.2742280984735));
#19302=CARTESIAN_POINT('Ctrl Pts',(2.74813437211341,-3.39734966840464,17.4727442158852));
#19303=CARTESIAN_POINT('Ctrl Pts',(0.675545012814546,-0.406208484742623,
17.6712603332969));
#19304=CARTESIAN_POINT('Ctrl Pts',(2.06545401745235,2.9569307023417,17.8697764507085));
#19305=CARTESIAN_POINT('Ctrl Pts',(5.64500915845253,3.61216899900811,18.0682925681202));
#19306=CARTESIAN_POINT('Ctrl Pts',(8.13612192804524,0.959451637121888,18.2668086855318));
#19307=CARTESIAN_POINT('Ctrl Pts',(7.25747863782803,-2.57191328333314,18.4653248029435));
#19308=CARTESIAN_POINT('Ctrl Pts',(3.81372409941205,-3.74796894189382,18.6638409203551));
#19309=CARTESIAN_POINT('Ctrl Pts',(0.958583211925542,-1.49170593738941,
18.8623570377668));
#19310=CARTESIAN_POINT('Ctrl Pts',(1.306739689582,2.13063298930591,19.0608731551785));
#19311=CARTESIAN_POINT('Ctrl Pts',(4.53935845279781,3.80177875335989,19.2593892725901));
#19312=CARTESIAN_POINT('Ctrl Pts',(7.69606872911877,1.99132785253305,19.4579053900018));
#19313=CARTESIAN_POINT('Ctrl Pts',(7.88601529454458,-1.64274321646801,19.6564215074134));
#19314=CARTESIAN_POINT('Ctrl Pts',(4.93524869751396,-3.77242129631514,19.8549376248251));
#19315=CARTESIAN_POINT('Ctrl Pts',(1.54602485826833,-2.44738771167893,20.0534537422367));
#19316=CARTESIAN_POINT('Ctrl Pts',(0.822130498506685,1.11891698433359,20.2519698596484));
#19317=CARTESIAN_POINT('Ctrl Pts',(3.42649430375165,3.66053879154859,20.45048597706));
#19318=CARTESIAN_POINT('Ctrl Pts',(6.97408943990954,2.84990880161489,20.6490020944717));
#19319=CARTESIAN_POINT('Ctrl Pts',(8.21609576658401,-0.570613452685432,
20.8475182118833));
#19320=CARTESIAN_POINT('Ctrl Pts',(6.015107509745,-3.46857877108964,21.046034329295));
#19321=CARTESIAN_POINT('Ctrl Pts',(2.38674785836889,-3.19008561139642,21.2445504467067));
#19322=CARTESIAN_POINT('Ctrl Pts',(0.653799542140776,0.00982723311048271,
21.4430665641183));
#19323=CARTESIAN_POINT('Ctrl Pts',(2.40326370386975,3.2007405539671,21.64158268153));
#19324=CARTESIAN_POINT('Ctrl Pts',(6.03301426782987,3.46047642676426,21.8400987989417));
#19325=CARTESIAN_POINT('Ctrl Pts',(8.21899485607472,0.551174068759129,22.0386149163533));
#19326=CARTESIAN_POINT('Ctrl Pts',(6.95932575274402,-2.86288350711349,22.2371310337649));
#19327=CARTESIAN_POINT('Ctrl Pts',(3.40758848840856,-3.65516588504588,22.4356471511766));
#19328=CARTESIAN_POINT('Ctrl Pts',(0.816395477550012,-1.10011867661645,
22.6341632685882));
#19329=CARTESIAN_POINT('Ctrl Pts',(1.55871392857562,2.46239974611297,22.8326793859999));
#19330=CARTESIAN_POINT('Ctrl Pts',(4.95473900642221,3.76989269217354,23.0311955034116));
#19331=CARTESIAN_POINT('Ctrl Pts',(7.89446267408575,1.62500233414576,23.2297116208232));
#19332=CARTESIAN_POINT('Ctrl Pts',(7.68572824288089,-2.00805862937836,23.4282277382349));
#19333=CARTESIAN_POINT('Ctrl Pts',(4.5197169557303,-3.80213094627573,23.6267438556465));
#19334=CARTESIAN_POINT('Ctrl Pts',(1.29575144062437,-2.11437372177854,23.8252599730582));
#19335=CARTESIAN_POINT('Ctrl Pts',(0.966374421579891,1.50985866999905,24.0237760904698));
#19336=CARTESIAN_POINT('Ctrl Pts',(3.83303817896047,3.7510614900228,24.2222922078815));
#19337=CARTESIAN_POINT('Ctrl Pts',(7.27086121968984,2.55774591981802,24.4208083252931));
#19338=CARTESIAN_POINT('Ctrl Pts',(8.13087041382945,-0.979117951521988,
24.6193244427048));
#19339=CARTESIAN_POINT('Ctrl Pts',(5.62679079307294,-3.61699263579137,24.8178405601165));
#19340=CARTESIAN_POINT('Ctrl Pts',(2.04930166016011,-2.94701073564213,25.0163566775281));
#19341=CARTESIAN_POINT('Ctrl Pts',(0.679470245798868,0.430859512276974,
25.2148727949398));
#19342=CARTESIAN_POINT('Ctrl Pts',(2.06768632464525,2.40576215381105,25.3472168732142));
#19343=CARTESIAN_POINT('Ctrl Pts',(3.02612799462649,2.8815178478641,25.4133889123514));
#19344=CARTESIAN_POINT('Ctrl Pts',(6.63714354025255,2.37292574162131,4.40103865535666));
#19345=CARTESIAN_POINT('Ctrl Pts',(6.55488268407852,2.44852193194201,4.39474007739806));
#19346=CARTESIAN_POINT('Ctrl Pts',(6.46865122448045,2.51987705892792,4.38835546741982));
#19347=CARTESIAN_POINT('Ctrl Pts',(6.34696491642476,2.61030910125518,4.37937007910812));
#19348=CARTESIAN_POINT('Ctrl Pts',(6.31472595028534,2.63335701953105,4.3769914840871));
#19349=CARTESIAN_POINT('Ctrl Pts',(6.27107086748787,2.66336558124252,4.37376126446673));
#19350=CARTESIAN_POINT('Ctrl Pts',(6.26002316332987,2.67085913519949,4.37294301546732));
#19351=CARTESIAN_POINT('Ctrl Pts',(6.24261690245388,2.68250839866624,4.37165205802598));
#19352=CARTESIAN_POINT('Ctrl Pts',(6.23628951948158,2.6867107311069,4.37118241763664));
#19353=CARTESIAN_POINT('Ctrl Pts',(6.22330577753974,2.69526789232314,4.37021785074703));
#19354=CARTESIAN_POINT('Ctrl Pts',(6.21664813926369,2.69962045492134,4.36972277181799));
#19355=CARTESIAN_POINT('Ctrl Pts',(6.20075835437278,2.70992495110662,4.36854012389255));
#19356=CARTESIAN_POINT('Ctrl Pts',(6.19151180693461,2.71585438495665,4.36785109474993));
#19357=CARTESIAN_POINT('Ctrl Pts',(6.160121426178,2.73575802401162,4.36550966700096));
#19358=CARTESIAN_POINT('Ctrl Pts',(6.13783830938031,2.7495091732844,4.36384371533823));
#19359=CARTESIAN_POINT('Ctrl Pts',(6.08327588902524,2.78226893632639,4.35975985053256));
#19360=CARTESIAN_POINT('Ctrl Pts',(6.05082845238185,2.80098889165221,4.35732739463932));
#19361=CARTESIAN_POINT('Ctrl Pts',(5.92055058942352,2.87315321216537,4.34756715150589));
#19362=CARTESIAN_POINT('Ctrl Pts',(5.82030654684858,2.92206918328703,4.34007319236212));
#19363=CARTESIAN_POINT('Ctrl Pts',(5.46097046585614,3.0748899487689,4.31368798604764));
#19364=CARTESIAN_POINT('Ctrl Pts',(5.19105024728478,3.15030519228401,4.29483732674159));
#19365=CARTESIAN_POINT('Ctrl Pts',(4.87794294707159,3.19528722530131,4.2748209914205));
#19366=CARTESIAN_POINT('Ctrl Pts',(4.84104104073695,3.19993832188371,4.27248750713435));
#19367=CARTESIAN_POINT('Ctrl Pts',(4.78625005656266,3.20588259564447,4.26905934501755));
#19368=CARTESIAN_POINT('Ctrl Pts',(4.768418409425,3.20766680708476,4.26794935779944));
#19369=CARTESIAN_POINT('Ctrl Pts',(4.7366175001221,3.21058107167193,4.26597970089389));
#19370=CARTESIAN_POINT('Ctrl Pts',(4.722654121626,3.21176890323759,4.26511824015335));
#19371=CARTESIAN_POINT('Ctrl Pts',(4.6931501173022,3.21408500617995,4.26330498964153));
#19372=CARTESIAN_POINT('Ctrl Pts',(4.67760812520572,3.21519173232151,4.2623538961011));
#19373=CARTESIAN_POINT('Ctrl Pts',(4.63620557221076,3.2178383225922,4.25983077171111));
#19374=CARTESIAN_POINT('Ctrl Pts',(4.61033310461793,3.21917918065689,4.25826498224459));
#19375=CARTESIAN_POINT('Ctrl Pts',(4.48230818218853,3.22426715039714,4.25056729856685));
#19376=CARTESIAN_POINT('Ctrl Pts',(4.38002823204493,3.22346492852175,4.24457846371601));
#19377=CARTESIAN_POINT('Ctrl Pts',(4.05824805926166,3.2056131389574,4.22603670586311));
#19378=CARTESIAN_POINT('Ctrl Pts',(3.84037747209945,3.17095675489344,4.21395968460233));
#19379=CARTESIAN_POINT('Ctrl Pts',(3.49629258695045,3.07939594756862,4.19385642585561));
#19380=CARTESIAN_POINT('Ctrl Pts',(3.36721050871641,3.03613653969115,4.18605151726928));
#19381=CARTESIAN_POINT('Ctrl Pts',(3.22562740500828,2.9784948021723,4.17679911218933));
#19382=CARTESIAN_POINT('Ctrl Pts',(3.21004177644008,2.97200630279114,4.1757708375915));
#19383=CARTESIAN_POINT('Ctrl Pts',(3.18519325751506,2.96143170810658,4.1741146693485));
#19384=CARTESIAN_POINT('Ctrl Pts',(3.17589716340947,2.9574238008972,4.17349129744577));
#19385=CARTESIAN_POINT('Ctrl Pts',(3.15941805788424,2.95022675503432,4.17237925543451));
#19386=CARTESIAN_POINT('Ctrl Pts',(3.15222762705379,2.94705505388434,4.17189164343547));
#19387=CARTESIAN_POINT('Ctrl Pts',(3.1367918728316,2.9401787814991,4.17083965940718));
#19388=CARTESIAN_POINT('Ctrl Pts',(3.12855065247452,2.93646587635556,4.17027480545196));
#19389=CARTESIAN_POINT('Ctrl Pts',(3.10568063995503,2.92604631954392,4.16869861759416));
#19390=CARTESIAN_POINT('Ctrl Pts',(3.09108653173385,2.91926479528544,4.16768289114376));
#19391=CARTESIAN_POINT('Ctrl Pts',(3.00560381272456,2.87876185249217,4.16167762961063));
#19392=CARTESIAN_POINT('Ctrl Pts',(2.93592123784515,2.84257135568898,4.15655612283921));
#19393=CARTESIAN_POINT('Ctrl Pts',(2.68541284117065,2.70061929695741,4.13747898122937));
#19394=CARTESIAN_POINT('Ctrl Pts',(2.51369121042546,2.5798451953233,4.12312153948582));
#19395=CARTESIAN_POINT('Ctrl Pts',(2.22834397850403,2.33440408802079,4.09794487026822));
#19396=CARTESIAN_POINT('Ctrl Pts',(2.11042164841072,2.21586561164759,4.08702846526219));
#19397=CARTESIAN_POINT('Ctrl Pts',(1.98455041380825,2.06796451924443,4.07480193663515));
#19398=CARTESIAN_POINT('Ctrl Pts',(1.96716265469409,2.04700091311345,4.07309812618114));
#19399=CARTESIAN_POINT('Ctrl Pts',(1.93906762667253,2.01224058369367,4.07031975593556));
#19400=CARTESIAN_POINT('Ctrl Pts',(1.9282033194139,1.99857311759262,4.06923891004568));
#19401=CARTESIAN_POINT('Ctrl Pts',(1.90884863049959,1.97381421231537,4.06730140466714));
#19402=CARTESIAN_POINT('Ctrl Pts',(1.90031833680597,1.96275466801485,4.06644317176497));
#19403=CARTESIAN_POINT('Ctrl Pts',(1.88225380033723,1.93901643977188,4.06461624372245));
#19404=CARTESIAN_POINT('Ctrl Pts',(1.87274070080213,1.92632207479819,4.06364839295676));
#19405=CARTESIAN_POINT('Ctrl Pts',(1.8471730468032,1.89167420662591,4.06103099857694));
#19406=CARTESIAN_POINT('Ctrl Pts',(1.83130181161244,1.86958657831453,4.05938856069004));
#19407=CARTESIAN_POINT('Ctrl Pts',(1.7462413396612,1.74799070773689,4.05048324001675));
#19408=CARTESIAN_POINT('Ctrl Pts',(1.68242372657146,1.64483526708385,4.04342609480348));
#19409=CARTESIAN_POINT('Ctrl Pts',(1.54710730965076,1.39573022678048,4.02723439550252));
#19410=CARTESIAN_POINT('Ctrl Pts',(1.48053060468139,1.24749381197568,4.01823512076678));
#19411=CARTESIAN_POINT('Ctrl Pts',(1.39684237616308,1.01580908814963,4.00442603493253));
#19412=CARTESIAN_POINT('Ctrl Pts',(1.37138949904329,0.9356636824112,3.99969011159615));
#19413=CARTESIAN_POINT('Ctrl Pts',(1.32517093714158,0.767614272247132,3.98968340997938));
#19414=CARTESIAN_POINT('Ctrl Pts',(1.30490904509874,0.679651377057018,3.9844032805968));
#19415=CARTESIAN_POINT('Ctrl Pts',(1.28547292042375,0.575455991472863,3.97797809526813));
#19416=CARTESIAN_POINT('Ctrl Pts',(1.28269421267998,0.559927951396196,3.97701614546647));
#19417=CARTESIAN_POINT('Ctrl Pts',(1.27835703829167,0.534620704294659,3.97544028404424));
#19418=CARTESIAN_POINT('Ctrl Pts',(1.27672941411996,0.524853406381223,3.9748301245578));
#19419=CARTESIAN_POINT('Ctrl Pts',(1.27389602883365,0.507353346849962,3.97373314985021));
#19420=CARTESIAN_POINT('Ctrl Pts',(1.27267339156884,0.499623514805698,3.97324729181695));
#19421=CARTESIAN_POINT('Ctrl Pts',(1.27005674941131,0.482680715699323,3.97217941298946));
#19422=CARTESIAN_POINT('Ctrl Pts',(1.26867455853299,0.47346625807546,3.97159676239257));
#19423=CARTESIAN_POINT('Ctrl Pts',(1.26482731482698,0.447037631196479,3.96992049698131));
#19424=CARTESIAN_POINT('Ctrl Pts',(1.26246165270143,0.429809636743399,3.96882156870142));
#19425=CARTESIAN_POINT('Ctrl Pts',(1.24637826765028,0.305207683919472,3.96083271876518));
#19426=CARTESIAN_POINT('Ctrl Pts',(1.23794002750252,0.197232275798578,3.95369310244792));
#19427=CARTESIAN_POINT('Ctrl Pts',(1.22865345360236,-0.138725282627019,
3.93119484354953));
#19428=CARTESIAN_POINT('Ctrl Pts',(1.24653243089846,-0.366552032762402,
3.91558625067927));
#19429=CARTESIAN_POINT('Ctrl Pts',(1.31030989068635,-0.70868233097507,3.8926303279593));
#19430=CARTESIAN_POINT('Ctrl Pts',(1.3389117627164,-0.825463839051558,3.88487144671705));
#19431=CARTESIAN_POINT('Ctrl Pts',(1.38210312469079,-0.967040775300621,
3.87556839034563));
#19432=CARTESIAN_POINT('Ctrl Pts',(1.39057972650078,-0.993587660551746,
3.87382828416188));
#19433=CARTESIAN_POINT('Ctrl Pts',(1.4045180813754,-1.035361778117,3.87109618430907));
#19434=CARTESIAN_POINT('Ctrl Pts',(1.40975182770082,-1.05066308093795,3.87009676015599));
#19435=CARTESIAN_POINT('Ctrl Pts',(1.41971047807015,-1.07907777978,3.86824304451542));
#19436=CARTESIAN_POINT('Ctrl Pts',(1.42440568862094,-1.09220110866687,3.86738779626718));
#19437=CARTESIAN_POINT('Ctrl Pts',(1.4350298487967,-1.12129956485655,3.86549323885396));
#19438=CARTESIAN_POINT('Ctrl Pts',(1.44100068371131,-1.13725903411091,3.86445534932941));
#19439=CARTESIAN_POINT('Ctrl Pts',(1.45881585788157,-1.1837503947489,3.86143489130146));
#19440=CARTESIAN_POINT('Ctrl Pts',(1.47099954344172,-1.21415056836899,3.85946368227856));
#19441=CARTESIAN_POINT('Ctrl Pts',(1.49968350643886,-1.28267763377836,3.85502544082345));
#19442=CARTESIAN_POINT('Ctrl Pts',(1.51646197687699,-1.32068213309878,3.85256776540599));
#19443=CARTESIAN_POINT('Ctrl Pts',(1.5746066649179,-1.44578050557826,3.84447705397044));
#19444=CARTESIAN_POINT('Ctrl Pts',(1.61914674970129,-1.53134459804915,3.83894350740677));
#19445=CARTESIAN_POINT('Ctrl Pts',(1.778715517037,-1.80694666613101,3.82089462923562));
#19446=CARTESIAN_POINT('Ctrl Pts',(1.90952483699347,-1.98707954159423,3.80876126785247));
#19447=CARTESIAN_POINT('Ctrl Pts',(2.1168215912362,-2.21810207501499,3.79092449909815));
#19448=CARTESIAN_POINT('Ctrl Pts',(2.1785168759092,-2.2814157953018,3.78574902387989));
#19449=CARTESIAN_POINT('Ctrl Pts',(2.2541382939114,-2.35289247870969,3.77944059449199));
#19450=CARTESIAN_POINT('Ctrl Pts',(2.26562585417085,-2.3635925718365,3.77848318624358));
#19451=CARTESIAN_POINT('Ctrl Pts',(2.28446891407095,-2.38088855824728,3.77691329431993));
#19452=CARTESIAN_POINT('Ctrl Pts',(2.29177752751084,-2.3875354498998,3.77630451584164));
#19453=CARTESIAN_POINT('Ctrl Pts',(2.30492952173099,-2.39938663164652,3.77520899355371));
#19454=CARTESIAN_POINT('Ctrl Pts',(2.31076142675809,-2.40460336515258,3.77472319571049));
#19455=CARTESIAN_POINT('Ctrl Pts',(2.32359342226826,-2.41599793931169,3.77365420546329));
#19456=CARTESIAN_POINT('Ctrl Pts',(2.33060128390207,-2.42216653490683,3.7730703736257));
#19457=CARTESIAN_POINT('Ctrl Pts',(2.35080461701518,-2.43979508856389,3.77138738132441));
#19458=CARTESIAN_POINT('Ctrl Pts',(2.36406640284601,-2.45117806583521,3.77028284263082));
#19459=CARTESIAN_POINT('Ctrl Pts',(2.4621748538238,-2.53401106487337,3.76211735666286));
#19460=CARTESIAN_POINT('Ctrl Pts',(2.55055938668049,-2.60113908931772,3.75479440108431));
#19461=CARTESIAN_POINT('Ctrl Pts',(2.83233467554104,-2.79306617366292,3.7319551653276));
#19462=CARTESIAN_POINT('Ctrl Pts',(3.03579394575537,-2.90184944463289,3.71620264191942));
#19463=CARTESIAN_POINT('Ctrl Pts',(3.35635752644414,-3.03137811991607,3.6934343253737));
#19464=CARTESIAN_POINT('Ctrl Pts',(3.46587483272944,-3.06891300888237,3.68597227780328));
#19465=CARTESIAN_POINT('Ctrl Pts',(3.60371155635547,-3.10800295327964,3.67696974816441));
#19466=CARTESIAN_POINT('Ctrl Pts',(3.63033389859338,-3.11518514555741,3.67524826398053));
#19467=CARTESIAN_POINT('Ctrl Pts',(3.67264699455988,-3.12601980402549,3.67253880236369));
#19468=CARTESIAN_POINT('Ctrl Pts',(3.68827811827691,-3.12989768826049,3.67154359781388));
#19469=CARTESIAN_POINT('Ctrl Pts',(3.71613899817122,-3.13658832904476,3.6697796907865));
#19470=CARTESIAN_POINT('Ctrl Pts',(3.72835725498703,-3.13944710959247,3.66900952383088));
#19471=CARTESIAN_POINT('Ctrl Pts',(3.75669072457087,-3.14590215974455,3.66723123430979));
#19472=CARTESIAN_POINT('Ctrl Pts',(3.77281759004304,-3.14944611040867,3.66622480512684));
#19473=CARTESIAN_POINT('Ctrl Pts',(3.81852870812302,-3.15912367826299,3.66338786105483));
#19474=CARTESIAN_POINT('Ctrl Pts',(3.84817345768673,-3.16496553910517,3.66156665347908));
#19475=CARTESIAN_POINT('Ctrl Pts',(4.07958447297222,-3.20719631283937,3.64748521629961));
#19476=CARTESIAN_POINT('Ctrl Pts',(4.28433346042802,-3.22467592339774,3.63586481153996));
#19477=CARTESIAN_POINT('Ctrl Pts',(4.70776648503966,-3.22035175015661,3.61214653455955));
#19478=CARTESIAN_POINT('Ctrl Pts',(4.92533534426433,-3.19592825335681,3.6001191850577));
#19479=CARTESIAN_POINT('Ctrl Pts',(5.17531399632524,-3.14177983364646,3.58493232121331));
#19480=CARTESIAN_POINT('Ctrl Pts',(5.2117521295321,-3.13321971460517,3.58268278148958));
#19481=CARTESIAN_POINT('Ctrl Pts',(5.26068429100659,-3.12082134716424,3.57960328381719));
#19482=CARTESIAN_POINT('Ctrl Pts',(5.27331763260748,-3.11753851874338,3.57880290543457));
#19483=CARTESIAN_POINT('Ctrl Pts',(5.29321360210141,-3.112239229039,3.57753351194048));
#19484=CARTESIAN_POINT('Ctrl Pts',(5.30048985622825,-3.11027383697552,3.5770673923595));
#19485=CARTESIAN_POINT('Ctrl Pts',(5.31546292406649,-3.1061730448663,3.57610420237694));
#19486=CARTESIAN_POINT('Ctrl Pts',(5.32315871646269,-3.10403454841218,3.5756069425064));
#19487=CARTESIAN_POINT('Ctrl Pts',(5.34160834478264,-3.09883383139897,3.57440964479764));
#19488=CARTESIAN_POINT('Ctrl Pts',(5.35235429594077,-3.09574422464262,3.5737080495546));
#19489=CARTESIAN_POINT('Ctrl Pts',(5.38935421379915,-3.08489746764332,3.57127826306103));
#19490=CARTESIAN_POINT('Ctrl Pts',(5.41552446774038,-3.07686199033169,3.56953513563952));
#19491=CARTESIAN_POINT('Ctrl Pts',(5.47941747965404,-3.05634957809481,3.56522440861166));
#19492=CARTESIAN_POINT('Ctrl Pts',(5.51701730178626,-3.04350675278819,3.56264019759241));
#19493=CARTESIAN_POINT('Ctrl Pts',(5.66996691858379,-2.9880860358259,3.55195876841439));
#19494=CARTESIAN_POINT('Ctrl Pts',(5.78306712207926,-2.9396205982028,3.54366556446107));
#19495=CARTESIAN_POINT('Ctrl Pts',(6.06374047260983,-2.79984457493999,3.52245827590234));
#19496=CARTESIAN_POINT('Ctrl Pts',(6.22639116872241,-2.69995239561272,3.50958365281332));
#19497=CARTESIAN_POINT('Ctrl Pts',(6.37918776290017,-2.58636241268449,3.49716578845861));
#19498=CARTESIAN_POINT('Ctrl Pts',(2.17296269996979,-3.20554048108048,-0.411765747138983));
#19499=CARTESIAN_POINT('Ctrl Pts',(1.10598262521586,-2.44554835076675,-0.345549597099719));
#19500=CARTESIAN_POINT('Ctrl Pts',(-0.190085171851759,0.209786400507346,
-0.213161407923235));
#19501=CARTESIAN_POINT('Ctrl Pts',(2.11904905146237,4.02596493684606,-0.0146011796095345));
#19502=CARTESIAN_POINT('Ctrl Pts',(6.57036830017086,4.14281137096193,0.183914937802122));
#19503=CARTESIAN_POINT('Ctrl Pts',(9.08469850437939,0.471525498888313,0.382431055213778));
#19504=CARTESIAN_POINT('Ctrl Pts',(7.36116941620609,-3.63455711911314,0.580947172625436));
#19505=CARTESIAN_POINT('Ctrl Pts',(2.97726580402431,-4.41062931823268,0.77946329003709));
#19506=CARTESIAN_POINT('Ctrl Pts',(-0.0518523842630756,-1.14834011450979,
0.977979407448747));
#19507=CARTESIAN_POINT('Ctrl Pts',(1.04758148582589,3.16599895701937,1.1764955248604));
#19508=CARTESIAN_POINT('Ctrl Pts',(5.26885307852876,4.58075644304919,1.37501164227206));
#19509=CARTESIAN_POINT('Ctrl Pts',(8.74613631193873,1.80065901519612,1.57352775968371));
#19510=CARTESIAN_POINT('Ctrl Pts',(8.2950356860829,-2.62850749839492,1.77204387709537));
#19511=CARTESIAN_POINT('Ctrl Pts',(4.32864266632258,-4.6505056552148,1.97055999450703));
#19512=CARTESIAN_POINT('Ctrl Pts',(0.479313869061077,-2.41367545883394,
2.16907611191868));
#19513=CARTESIAN_POINT('Ctrl Pts',(0.272186515624751,2.03356129066451,2.36759222933034));
#19514=CARTESIAN_POINT('Ctrl Pts',(3.89694643539194,4.61849687019083,2.56610834674199));
#19515=CARTESIAN_POINT('Ctrl Pts',(8.03410612006349,2.97390317522259,2.76462446415365));
#19516=CARTESIAN_POINT('Ctrl Pts',(8.89493411795877,-1.39413568050936,2.9631405815653));
#19517=CARTESIAN_POINT('Ctrl Pts',(5.69110016326603,-4.48545097223521,3.16165669897696));
#19518=CARTESIAN_POINT('Ctrl Pts',(1.35661463604595,-3.46907591290164,3.36017281638862));
#19519=CARTESIAN_POINT('Ctrl Pts',(-0.139083166427389,0.724213049156903,
3.55868893380027));
#19520=CARTESIAN_POINT('Ctrl Pts',(2.57373840321099,4.25428138787658,3.75720505121192));
#19521=CARTESIAN_POINT('Ctrl Pts',(7.01072892820446,3.88835980295648,3.95572116862359));
#19522=CARTESIAN_POINT('Ctrl Pts',(9.10857690015422,-0.0384477492421469,
4.15423728603523));
#19523=CARTESIAN_POINT('Ctrl Pts',(6.94611304441007,-3.93004557143118,4.3527534034469));
#19524=CARTESIAN_POINT('Ctrl Pts',(2.50368062941278,-4.22258242327136,4.55126952085854));
#19525=CARTESIAN_POINT('Ctrl Pts',(-0.15042524517621,-0.648158610486061,
4.74978563827021));
#19526=CARTESIAN_POINT('Ctrl Pts',(1.41437509517098,3.51983652671062,4.94830175568186));
#19527=CARTESIAN_POINT('Ctrl Pts',(5.76506726388787,4.46443232806813,5.14681787309352));
#19528=CARTESIAN_POINT('Ctrl Pts',(8.91737013208296,1.32058592540232,5.34533399050517));
#19529=CARTESIAN_POINT('Ctrl Pts',(7.98446469607637,-3.03262794728552,5.54385010791683));
#19530=CARTESIAN_POINT('Ctrl Pts',(3.82068800849579,-4.60861883268182,5.74236622532849));
#19531=CARTESIAN_POINT('Ctrl Pts',(0.239147556357015,-1.9641242562649,5.94088234274014));
#19532=CARTESIAN_POINT('Ctrl Pts',(0.519749957626067,2.47907795239849,6.13939846015179));
#19533=CARTESIAN_POINT('Ctrl Pts',(4.40552487083362,4.65198772933701,6.33791457756345));
#19534=CARTESIAN_POINT('Ctrl Pts',(8.33795354574623,2.56469563392857,6.53643069497511));
#19535=CARTESIAN_POINT('Ctrl Pts',(8.71579260460107,-1.87129593734266,6.73494681238676));
#19536=CARTESIAN_POINT('Ctrl Pts',(5.19302422456139,-4.59359028502123,6.93346292979842));
#19537=CARTESIAN_POINT('Ctrl Pts',(0.995732677906764,-3.10916202902842,
7.13197904721008));
#19538=CARTESIAN_POINT('Ctrl Pts',(-0.0322822778871914,1.22257767061497,
7.33049516462173));
#19539=CARTESIAN_POINT('Ctrl Pts',(3.05041589877745,4.43470399540276,7.52901128203338));
#19540=CARTESIAN_POINT('Ctrl Pts',(7.42075085684839,3.58561275821527,7.72752739944505));
#19541=CARTESIAN_POINT('Ctrl Pts',(9.07645297431008,-0.547114437358846,
7.9260435168567));
#19542=CARTESIAN_POINT('Ctrl Pts',(6.5012617467849,-4.17880463841992,8.12455963426836));
#19543=CARTESIAN_POINT('Ctrl Pts',(2.05348831510913,-3.98362504090881,8.32307575168001));
#19544=CARTESIAN_POINT('Ctrl Pts',(-0.193681017610346,-0.140317407516647,
8.52159186909167));
#19545=CARTESIAN_POINT('Ctrl Pts',(1.81766867783776,3.83149023855917,8.72010798650331));
#19546=CARTESIAN_POINT('Ctrl Pts',(6.24558161029013,4.2944920068349,8.91862410391498));
#19547=CARTESIAN_POINT('Ctrl Pts',(9.03505934404192,0.824679685151172,9.11714022132663));
#19548=CARTESIAN_POINT('Ctrl Pts',(7.6315512320161,-3.40035860512303,9.31565633873829));
#19549=CARTESIAN_POINT('Ctrl Pts',(3.32036330565075,-4.51141316650472,9.51417245614994));
#19550=CARTESIAN_POINT('Ctrl Pts',(0.0495994604212725,-1.49100136617927,
9.71268857356161));
#19551=CARTESIAN_POINT('Ctrl Pts',(0.814563009263402,2.89484112343983,9.91120469097325));
#19552=CARTESIAN_POINT('Ctrl Pts',(4.91471488529713,4.62964317792977,10.1097208083849));
#19553=CARTESIAN_POINT('Ctrl Pts',(8.59521399360942,2.1247060752228,10.3082369257966));
#19554=CARTESIAN_POINT('Ctrl Pts',(8.48552926132444,-2.32599643497811,10.5067530432082));
#19555=CARTESIAN_POINT('Ctrl Pts',(4.68610787984395,-4.64659565516981,10.7052691606199));
#19556=CARTESIAN_POINT('Ctrl Pts',(0.676387677669684,-2.71193096197848,
10.9037852780315));
#19557=CARTESIAN_POINT('Ctrl Pts',(0.128394142987057,1.70626851979591,11.1023013954432));
#19558=CARTESIAN_POINT('Ctrl Pts',(3.54396933091606,4.56189974780998,11.3008175128549));
#19559=CARTESIAN_POINT('Ctrl Pts',(7.79519445548059,3.23982996331418,11.4993336302665));
#19560=CARTESIAN_POINT('Ctrl Pts',(8.98887841448097,-1.04921447348414,11.6978497476782));
#19561=CARTESIAN_POINT('Ctrl Pts',(6.03186814454124,-4.3774082536412,11.8963658650898));
#19562=CARTESIAN_POINT('Ctrl Pts',(1.63213740257258,-3.69685482224785,12.0948819825015));
#19563=CARTESIAN_POINT('Ctrl Pts',(-0.181124089683036,0.369207933724872,
12.2933980999131));
#19564=CARTESIAN_POINT('Ctrl Pts',(2.2526340504912,4.09715708707193,12.4919142173248));
#19565=CARTESIAN_POINT('Ctrl Pts',(6.70462241331237,4.07300771627025,12.6904303347364));
#19566=CARTESIAN_POINT('Ctrl Pts',(9.09779474190718,0.318875355730261,12.8889464521481));
#19567=CARTESIAN_POINT('Ctrl Pts',(7.24052934071316,-3.72727698993507,13.0874625695597));
#19568=CARTESIAN_POINT('Ctrl Pts',(2.83367453520978,-4.36005996854408,13.2859786869714));
#19569=CARTESIAN_POINT('Ctrl Pts',(-0.0870558709899348,-0.999982965095223,
13.4844948043831));
#19570=CARTESIAN_POINT('Ctrl Pts',(1.1530874699283,3.2758594160949,13.6830109217947));
#19571=CARTESIAN_POINT('Ctrl Pts',(5.41840487637927,4.55173205747878,13.8815270392064));
#19572=CARTESIAN_POINT('Ctrl Pts',(8.80279980247531,1.65921506374814,14.080043156618));
#19573=CARTESIAN_POINT('Ctrl Pts',(8.20690775291552,-2.75277952374592,14.2785592740297));
#19574=CARTESIAN_POINT('Ctrl Pts',(4.17643533161801,-4.64383098681233,14.4770753914414));
#19575=CARTESIAN_POINT('Ctrl Pts',(0.402412514292184,-2.28215036718792,
14.675591508853));
#19576=CARTESIAN_POINT('Ctrl Pts',(0.341017607518878,2.16948014760412,14.8741076262646));
#19577=CARTESIAN_POINT('Ctrl Pts',(4.04847489906614,4.63434201110855,15.0726237436763));
#19578=CARTESIAN_POINT('Ctrl Pts',(8.12956552465056,2.85516161537223,15.271139861088));
#19579=CARTESIAN_POINT('Ctrl Pts',(8.84690431993714,-1.53872147678918,15.4696559784996));
#19580=CARTESIAN_POINT('Ctrl Pts',(5.54356606143321,-4.52347271009317,15.6681720959113));
#19581=CARTESIAN_POINT('Ctrl Pts',(1.24468509012015,-3.36571368106855,15.8666882133229));
#19582=CARTESIAN_POINT('Ctrl Pts',(-0.112905173860372,0.874301914415817,
16.0652043307346));
#19583=CARTESIAN_POINT('Ctrl Pts',(2.71405060913991,4.31364844766405,16.2637204481462));
#19584=CARTESIAN_POINT('Ctrl Pts',(7.1366801074503,3.80263778683562,16.4622365655579));
#19585=CARTESIAN_POINT('Ctrl Pts',(9.10482335385156,-0.190756225336315,
16.6607526829696));
#19586=CARTESIAN_POINT('Ctrl Pts',(6.81609220134375,-4.00945931491334,16.8592688003812));
#19587=CARTESIAN_POINT('Ctrl Pts',(2.36646310311057,-4.15637583189606,17.0577849177929));
#19588=CARTESIAN_POINT('Ctrl Pts',(-0.16917825360623,-0.496962424679848,
17.2563010352045));
#19589=CARTESIAN_POINT('Ctrl Pts',(1.53126025266144,3.61755971783011,17.4548171526162));
#19590=CARTESIAN_POINT('Ctrl Pts',(5.91054938364417,4.41918948403437,17.6533332700278));
#19591=CARTESIAN_POINT('Ctrl Pts',(8.95821945609951,1.17380958265607,17.8518493874395));
#19592=CARTESIAN_POINT('Ctrl Pts',(7.88327219050615,-3.14652280629029,18.0503655048511));
#19593=CARTESIAN_POINT('Ctrl Pts',(3.67012384502666,-4.58532946245115,18.2488816222628));
#19594=CARTESIAN_POINT('Ctrl Pts',(0.177095531876928,-1.82497861910485,
18.4473977396744));
#19595=CARTESIAN_POINT('Ctrl Pts',(0.603036135785551,2.60665292882547,18.6459138570862));
#19596=CARTESIAN_POINT('Ctrl Pts',(4.55787735396168,4.65116130836808,18.8444299744978));
#19597=CARTESIAN_POINT('Ctrl Pts',(8.41985082781949,2.43622463611074,19.0429460919094));
#19598=CARTESIAN_POINT('Ctrl Pts',(8.65223471259592,-2.00976021586402,19.2414622093211));
#19599=CARTESIAN_POINT('Ctrl Pts',(5.04221626688697,-4.61524489208584,19.4399783267328));
#19600=CARTESIAN_POINT('Ctrl Pts',(0.895781713701428,-2.99417608693739,
19.6384944441444));
#19601=CARTESIAN_POINT('Ctrl Pts',(0.0101569427980723,1.36890222246852,
19.8370105615561));
#19602=CARTESIAN_POINT('Ctrl Pts',(3.1963802739596,4.47836591752857,20.0355266789677));
#19603=CARTESIAN_POINT('Ctrl Pts',(7.53656898706393,3.48662728959027,20.2340427963793));
#19604=CARTESIAN_POINT('Ctrl Pts',(9.05606082131957,-0.698098281184544,
20.432558913791));
#19605=CARTESIAN_POINT('Ctrl Pts',(6.36333405195284,-4.24351873734398,20.6310750312027));
#19606=CARTESIAN_POINT('Ctrl Pts',(1.9243366462227,-3.90280543100934,20.8295911486144));
#19607=CARTESIAN_POINT('Ctrl Pts',(-0.195782035254683,0.0120228054752082,
21.028107266026));
#19608=CARTESIAN_POINT('Ctrl Pts',(1.94454241477252,3.91584087042925,21.2266233834376));
#19609=CARTESIAN_POINT('Ctrl Pts',(6.38524148680512,4.23360619038166,21.4251395008493));
#19610=CARTESIAN_POINT('Ctrl Pts',(9.05960761710739,0.674315805600993,21.623655618261));
#19611=CARTESIAN_POINT('Ctrl Pts',(7.5185068390623,-3.50250076674849,21.8221717356726));
#19612=CARTESIAN_POINT('Ctrl Pts',(3.17325057532877,-4.47179261159471,22.0206878530843));
#19613=CARTESIAN_POINT('Ctrl Pts',(0.0031406198327811,-1.34590405051051,
22.2192039704959));
#19614=CARTESIAN_POINT('Ctrl Pts',(0.911305739869395,3.01254206724522,22.4177200879076));
#19615=CARTESIAN_POINT('Ctrl Pts',(5.06606104496655,4.6121513544261,22.6162362053192));
#19616=CARTESIAN_POINT('Ctrl Pts',(8.66256938155685,1.98805571626367,22.8147523227309));
#19617=CARTESIAN_POINT('Ctrl Pts',(8.4072000996685,-2.45669335535235,23.0132684401425));
#19618=CARTESIAN_POINT('Ctrl Pts',(4.53384760969594,-4.65159218721967,23.2117845575542));
#19619=CARTESIAN_POINT('Ctrl Pts',(0.589592923617338,-2.58676106216746,
23.4103006749659));
#19620=CARTESIAN_POINT('Ctrl Pts',(0.186627431348294,1.84718698340797,23.6088167923775));
#19621=CARTESIAN_POINT('Ctrl Pts',(3.69375302108596,4.58911293885384,23.8073329097892));
#19622=CARTESIAN_POINT('Ctrl Pts',(7.89964467060016,3.12919021086655,24.0058490272008));
#19623=CARTESIAN_POINT('Ctrl Pts',(8.95179466357075,-1.19786968887199,24.2043651446125));
#19624=CARTESIAN_POINT('Ctrl Pts',(5.88826072308503,-4.42509080397621,24.4028812620241));
#19625=CARTESIAN_POINT('Ctrl Pts',(1.51149918181804,-3.60542346049212,24.6013973794358));
#19626=CARTESIAN_POINT('Ctrl Pts',(-0.164376056275096,0.527120914407128,
24.7999134968474));
#19627=CARTESIAN_POINT('Ctrl Pts',(1.53399129555416,2.94325066577138,24.9322575751219));
#19628=CARTESIAN_POINT('Ctrl Pts',(2.70656526709436,3.52529833870864,24.9984296142591));
#19629=CARTESIAN_POINT('Ctrl Pts',(2.31196529717974,-3.01041142380583,-0.273445981108207));
#19630=CARTESIAN_POINT('Ctrl Pts',(1.30993489857133,-2.29668186568531,-0.207229831068943));
#19631=CARTESIAN_POINT('Ctrl Pts',(0.0927619053280601,0.197016191301887,
-0.0748416418924601));
#19632=CARTESIAN_POINT('Ctrl Pts',(2.26133350378215,3.78089464452436,0.123718586421241));
#19633=CARTESIAN_POINT('Ctrl Pts',(6.44169010710979,3.89062835157607,0.322234703832897));
#19634=CARTESIAN_POINT('Ctrl Pts',(8.80296690727615,0.442822593209179,0.520750821244553));
#19635=CARTESIAN_POINT('Ctrl Pts',(7.18435323294509,-3.41331277406459,0.719266938656211));
#19636=CARTESIAN_POINT('Ctrl Pts',(3.06730851213489,-4.14214356803415,0.917783056067867));
#19637=CARTESIAN_POINT('Ctrl Pts',(0.222580126422941,-1.07843785456408,
1.11629917347952));
#19638=CARTESIAN_POINT('Ctrl Pts',(1.25508877879203,2.97327688863128,1.31481529089117));
#19639=CARTESIAN_POINT('Ctrl Pts',(5.21940128729496,4.30191464036023,1.51333140830283));
#19640=CARTESIAN_POINT('Ctrl Pts',(8.48501382017349,1.69104851481962,1.71184752571448));
#19641=CARTESIAN_POINT('Ctrl Pts',(8.06137278822348,-2.46850384433775,1.91036364312614));
#19642=CARTESIAN_POINT('Ctrl Pts',(4.33642377308406,-4.36741804808325,2.1088797605378));
#19643=CARTESIAN_POINT('Ctrl Pts',(0.721412996069988,-2.26674915432179,
2.30739587794946));
#19644=CARTESIAN_POINT('Ctrl Pts',(0.526893989166935,1.90977346146706,2.50591199536111));
#19645=CARTESIAN_POINT('Ctrl Pts',(3.93100594327419,4.33735771577206,2.70442811277276));
#19646=CARTESIAN_POINT('Ctrl Pts',(7.81632664047099,2.79287444498747,2.90294423018442));
#19647=CARTESIAN_POINT('Ctrl Pts',(8.62475394129306,-1.30927124574203,3.10146034759608));
#19648=CARTESIAN_POINT('Ctrl Pts',(5.61594516345689,-4.21241064570382,3.29997646500774));
#19649=CARTESIAN_POINT('Ctrl Pts',(1.54531032840212,-3.25790481196126,3.49849258241939));
#19650=CARTESIAN_POINT('Ctrl Pts',(0.140659294449413,0.680128436785933,
3.69700869983105));
#19651=CARTESIAN_POINT('Ctrl Pts',(2.68834480713824,3.99531291703776,3.8955248172427));
#19652=CARTESIAN_POINT('Ctrl Pts',(6.85524491106594,3.65166587031902,4.09404093465435));
#19653=CARTESIAN_POINT('Ctrl Pts',(8.82539176693615,-0.0361073410931478,
4.29255705206602));
#19654=CARTESIAN_POINT('Ctrl Pts',(6.79456235351217,-3.69081412452673,4.49107316947766));
#19655=CARTESIAN_POINT('Ctrl Pts',(2.62255162068078,-3.96554354562172,4.68958928688933));
#19656=CARTESIAN_POINT('Ctrl Pts',(0.130007635661538,-0.608703617053558,
4.88810540430098));
#19657=CARTESIAN_POINT('Ctrl Pts',(1.59955476768487,3.30557550356288,5.08662152171263));
#19658=CARTESIAN_POINT('Ctrl Pts',(5.68540970649173,4.19267145760527,5.28513763912429));
#19659=CARTESIAN_POINT('Ctrl Pts',(8.64582422058695,1.24019864338394,5.48365375653594));
#19660=CARTESIAN_POINT('Ctrl Pts',(7.76970701088062,-2.84802449713069,5.68216987394761));
#19661=CARTESIAN_POINT('Ctrl Pts',(3.85938955257665,-4.32808097846753,5.88068599135924));
#19662=CARTESIAN_POINT('Ctrl Pts',(0.495866191827503,-1.844563228489,6.07920210877092));
#19663=CARTESIAN_POINT('Ctrl Pts',(0.759387641428115,2.32817043879295,6.27771822618256));
#19664=CARTESIAN_POINT('Ctrl Pts',(4.40862597053364,4.36880990474354,6.47623434359423));
#19665=CARTESIAN_POINT('Ctrl Pts',(8.10167813322798,2.40857636349708,6.67475046100588));
#19666=CARTESIAN_POINT('Ctrl Pts',(8.45651720821394,-1.75738559545474,6.87326657841754));
#19667=CARTESIAN_POINT('Ctrl Pts',(5.14818832037566,-4.31396725511023,7.0717826958292));
#19668=CARTESIAN_POINT('Ctrl Pts',(1.20639613410644,-2.9198997628929,7.27029881324085));
#19669=CARTESIAN_POINT('Ctrl Pts',(0.240958952754043,1.14815638979818,7.4688149306525));
#19670=CARTESIAN_POINT('Ctrl Pts',(3.13600578243834,4.16475276096279,7.66733104806417));
#19671=CARTESIAN_POINT('Ctrl Pts',(7.24030780616454,3.36734777563528,7.86584716547581));
#19672=CARTESIAN_POINT('Ctrl Pts',(8.79522330270695,-0.513810248872322,
8.06436328288747));
#19673=CARTESIAN_POINT('Ctrl Pts',(6.37679023796107,-3.92443062116999,8.26287940029913));
#19674=CARTESIAN_POINT('Ctrl Pts',(2.1997636091463,-3.74113208118609,8.46139551771078));
#19675=CARTESIAN_POINT('Ctrl Pts',(0.089384947459713,-0.131775945129999,
8.65991163512245));
#19676=CARTESIAN_POINT('Ctrl Pts',(1.97829888761515,3.5982580948319,8.8584277525341));
#19677=CARTESIAN_POINT('Ctrl Pts',(6.13667397417128,4.03307581767334,9.05694386994575));
#19678=CARTESIAN_POINT('Ctrl Pts',(8.75634940354159,0.774479423926291,9.2554599873574));
#19679=CARTESIAN_POINT('Ctrl Pts',(7.43827624901926,-3.19337049409171,9.45397610476906));
#19680=CARTESIAN_POINT('Ctrl Pts',(3.38952083310589,-4.23679245796831,9.65249222218073));
#19681=CARTESIAN_POINT('Ctrl Pts',(0.317856350200649,-1.40024048117564,
9.85100833959237));
#19682=CARTESIAN_POINT('Ctrl Pts',(1.03625470449417,2.71862509287945,10.049524457004));
#19683=CARTESIAN_POINT('Ctrl Pts',(4.88682034851015,4.34782552060827,10.2480405744157));
#19684=CARTESIAN_POINT('Ctrl Pts',(8.34327851098385,1.99537004097493,10.4465566918273));
#19685=CARTESIAN_POINT('Ctrl Pts',(8.24027055552775,-2.18440736622039,10.645072809239));
#19686=CARTESIAN_POINT('Ctrl Pts',(4.67212920832948,-4.36374605926514,10.8435889266506));
#19687=CARTESIAN_POINT('Ctrl Pts',(0.906490441907856,-2.54684911848653,
11.0421050440623));
#19688=CARTESIAN_POINT('Ctrl Pts',(0.391854608507251,1.60240379879482,11.2406211614739));
#19689=CARTESIAN_POINT('Ctrl Pts',(3.59951541494433,4.28420579809219,11.4391372788856));
#19690=CARTESIAN_POINT('Ctrl Pts',(7.59195811086242,3.04261362173219,11.6376533962972));
#19691=CARTESIAN_POINT('Ctrl Pts',(8.71297961965247,-0.98534623276214,11.8361695137089));
#19692=CARTESIAN_POINT('Ctrl Pts',(5.93596976765481,-4.11094475056566,12.0346856311206));
#19693=CARTESIAN_POINT('Ctrl Pts',(1.80406135300024,-3.47181826426207,12.2332017485322));
#19694=CARTESIAN_POINT('Ctrl Pts',(0.101177504597399,0.346733347466743,
12.4317178659439));
#19695=CARTESIAN_POINT('Ctrl Pts',(2.38678685852808,3.84775315515312,12.6302339833555));
#19696=CARTESIAN_POINT('Ctrl Pts',(6.56777184536255,3.82507381537617,12.8287501007672));
#19697=CARTESIAN_POINT('Ctrl Pts',(8.81526594492522,0.29946463609684,13.0272662181788));
#19698=CARTESIAN_POINT('Ctrl Pts',(7.07105681270762,-3.5003885604986,13.2257823355905));
#19699=CARTESIAN_POINT('Ctrl Pts',(2.93245799361878,-4.09465249784007,13.4242984530022));
#19700=CARTESIAN_POINT('Ctrl Pts',(0.189519561683291,-0.939111566208993,
13.6228145704138));
#19701=CARTESIAN_POINT('Ctrl Pts',(1.35417235664619,3.07644987396012,13.8213306878255));
#19702=CARTESIAN_POINT('Ctrl Pts',(5.3598495029257,4.27465703983832,14.0198468052371));
#19703=CARTESIAN_POINT('Ctrl Pts',(8.53822806601778,1.55821460123144,14.2183629226488));
#19704=CARTESIAN_POINT('Ctrl Pts',(7.97860941701375,-2.58521112879858,14.4168790400604));
#19705=CARTESIAN_POINT('Ctrl Pts',(4.19348166959603,-4.36114968300486,14.6153951574721));
#19706=CARTESIAN_POINT('Ctrl Pts',(0.649192814085452,-2.14323031537866,
14.8139112748837));
#19707=CARTESIAN_POINT('Ctrl Pts',(0.59153516483578,2.03741860650786,15.0124273922954));
#19708=CARTESIAN_POINT('Ctrl Pts',(4.07331050026509,4.35223832436584,15.2109435097071));
#19709=CARTESIAN_POINT('Ctrl Pts',(7.9059751985768,2.68136097312093,15.4094596271187));
#19710=CARTESIAN_POINT('Ctrl Pts',(8.57964783407003,-1.44505575241412,15.6079757445304));
#19711=CARTESIAN_POINT('Ctrl Pts',(5.47739182177246,-4.24811790776339,15.806491861942));
#19712=CARTESIAN_POINT('Ctrl Pts',(1.44019420657955,-3.16083449095397,16.0050079793537));
#19713=CARTESIAN_POINT('Ctrl Pts',(0.165243768843413,0.821081027223728,
16.2035240967653));
#19714=CARTESIAN_POINT('Ctrl Pts',(2.82011586731386,4.05106615928717,16.402040214177));
#19715=CARTESIAN_POINT('Ctrl Pts',(6.97352913523386,3.57116196212476,16.6005563315886));
#19716=CARTESIAN_POINT('Ctrl Pts',(8.82186670813997,-0.17914442924803,16.7990724490003));
#19717=CARTESIAN_POINT('Ctrl Pts',(6.67245619587356,-3.76539376000376,16.997588566412));
#19718=CARTESIAN_POINT('Ctrl Pts',(2.49368685944485,-3.90336711073225,17.1961046838236));
#19719=CARTESIAN_POINT('Ctrl Pts',(0.112396168534027,-0.466711111367439,
17.3946208012353));
#19720=CARTESIAN_POINT('Ctrl Pts',(1.70932484092508,3.39735004600064,17.5931369186469));
#19721=CARTESIAN_POINT('Ctrl Pts',(5.82203597524696,4.15018265569229,17.7916530360586));
#19722=CARTESIAN_POINT('Ctrl Pts',(8.68418694674809,1.10235693414467,17.9901691534703));
#19723=CARTESIAN_POINT('Ctrl Pts',(7.67467433961344,-2.9549862986379,18.1886852708819));
#19724=CARTESIAN_POINT('Ctrl Pts',(3.71799059648846,-4.30620928893205,18.3872013882936));
#19725=CARTESIAN_POINT('Ctrl Pts',(0.437591425226463,-1.7138877251997,18.5857175057052));
#19726=CARTESIAN_POINT('Ctrl Pts',(0.837603987051035,2.44797961565228,18.7842336231169));
#19727=CARTESIAN_POINT('Ctrl Pts',(4.55170438690705,4.36803379003202,18.9827497405285));
#19728=CARTESIAN_POINT('Ctrl Pts',(8.17859012825258,2.28792570825151,19.1812658579402));
#19729=CARTESIAN_POINT('Ctrl Pts',(8.39682823991214,-1.88742121606535,19.3797819753518));
#19730=CARTESIAN_POINT('Ctrl Pts',(5.0065604104293,-4.33430369349561,19.5782980927635));
#19731=CARTESIAN_POINT('Ctrl Pts',(1.11252942855707,-2.81191329518458,19.7768142101752));
#19732=CARTESIAN_POINT('Ctrl Pts',(0.280814794700937,1.28557380975688,19.9753303275868));
#19733=CARTESIAN_POINT('Ctrl Pts',(3.27308495055695,4.20575687553525,20.1738464449984));
#19734=CARTESIAN_POINT('Ctrl Pts',(7.34907580467911,3.27438779359847,20.3723625624101));
#19735=CARTESIAN_POINT('Ctrl Pts',(8.77607246974106,-0.65560333835151,20.5708786798217));
#19736=CARTESIAN_POINT('Ctrl Pts',(6.24725853788356,-3.98520541525919,20.7693947972334));
#19737=CARTESIAN_POINT('Ctrl Pts',(2.07847371693811,-3.66523215780504,20.9679109146451));
#19738=CARTESIAN_POINT('Ctrl Pts',(0.0874118238771355,0.0112909480203034,
21.1664270320568));
#19739=CARTESIAN_POINT('Ctrl Pts',(2.09744951113826,3.6774740982752,21.3649431494684));
#19740=CARTESIAN_POINT('Ctrl Pts',(6.26783241381338,3.97589626917586,21.56345926688));
#19741=CARTESIAN_POINT('Ctrl Pts',(8.77940336342984,0.633268559987037,21.7619753842917));
#19742=CARTESIAN_POINT('Ctrl Pts',(7.33211314362288,-3.28929501353682,21.9604915017033));
#19743=CARTESIAN_POINT('Ctrl Pts',(3.25136321302202,-4.1995837027451,22.159007619115));
#19744=CARTESIAN_POINT('Ctrl Pts',(0.274225572405194,-1.26397559254583,
22.3575237365266));
#19745=CARTESIAN_POINT('Ctrl Pts',(1.12710846943813,2.82916129353447,22.5560398539383));
#19746=CARTESIAN_POINT('Ctrl Pts',(5.0289536987851,4.33139846700858,22.75455597135));
#19747=CARTESIAN_POINT('Ctrl Pts',(8.40653381239982,1.86703792222437,22.9530720887616));
#19748=CARTESIAN_POINT('Ctrl Pts',(8.1667094807393,-2.30714844669435,23.1515882061733));
#19749=CARTESIAN_POINT('Ctrl Pts',(4.52913739170739,-4.36843844023836,23.3501043235849));
#19750=CARTESIAN_POINT('Ctrl Pts',(0.824979095953012,-2.42929861537115,
23.5486204409966));
#19751=CARTESIAN_POINT('Ctrl Pts',(0.44654309475883,1.73474421227166,23.7471365584082));
#19752=CARTESIAN_POINT('Ctrl Pts',(3.74018140704413,4.30976245591016,23.9456526758199));
#19753=CARTESIAN_POINT('Ctrl Pts',(7.69005018696339,2.93870878051704,24.1441687932315));
#19754=CARTESIAN_POINT('Ctrl Pts',(8.67815324699032,-1.12495244308866,24.3426849106432));
#19755=CARTESIAN_POINT('Ctrl Pts',(5.80110407974766,-4.15572474791461,24.5412010280549));
#19756=CARTESIAN_POINT('Ctrl Pts',(1.69076667459873,-3.38595255220879,24.7397171454665));
#19757=CARTESIAN_POINT('Ctrl Pts',(0.116906044416222,0.495033780363739,
24.9382332628782));
#19758=CARTESIAN_POINT('Ctrl Pts',(1.71188963858453,2.76408782845127,25.0705773411526));
#19759=CARTESIAN_POINT('Ctrl Pts',(2.81308617627174,3.31070484176046,25.1367493802898));
#19760=CARTESIAN_POINT('Ctrl Pts',(2.45096789438968,-2.81528236653118,-0.135126215077433));
#19761=CARTESIAN_POINT('Ctrl Pts',(1.5138871719268,-2.14781538060387,-0.0689100650381678));
#19762=CARTESIAN_POINT('Ctrl Pts',(0.375608982507884,0.184245982096433,
0.0634781241383155));
#19763=CARTESIAN_POINT('Ctrl Pts',(2.40361795610193,3.53582435220265,0.262038352452016));
#19764=CARTESIAN_POINT('Ctrl Pts',(6.31301191404873,3.63844533219021,0.460554469863673));
#19765=CARTESIAN_POINT('Ctrl Pts',(8.52123531017291,0.41411968753004,0.659070587275328));
#19766=CARTESIAN_POINT('Ctrl Pts',(7.00753704968407,-3.19206842901602,0.857586704686986));
#19767=CARTESIAN_POINT('Ctrl Pts',(3.15735122024546,-3.87365781783563,1.05610282209864));
#19768=CARTESIAN_POINT('Ctrl Pts',(0.497012637108953,-1.00853559461836,
1.25461893951029));
#19769=CARTESIAN_POINT('Ctrl Pts',(1.46259607175817,2.78055482024318,1.45313505692195));
#19770=CARTESIAN_POINT('Ctrl Pts',(5.16994949606116,4.02307283767128,1.6516511743336));
#19771=CARTESIAN_POINT('Ctrl Pts',(8.22389132840824,1.58143801444312,1.85016729174526));
#19772=CARTESIAN_POINT('Ctrl Pts',(7.82770989036406,-2.30850019028058,2.04868340915692));
#19773=CARTESIAN_POINT('Ctrl Pts',(4.34420487984554,-4.08433044095169,2.24719952656857));
#19774=CARTESIAN_POINT('Ctrl Pts',(0.963512123078899,-2.11982284980964,
2.44571564398023));
#19775=CARTESIAN_POINT('Ctrl Pts',(0.781601462709117,1.78598563226962,2.64423176139188));
#19776=CARTESIAN_POINT('Ctrl Pts',(3.96506545115642,4.05621856135326,2.84274787880354));
#19777=CARTESIAN_POINT('Ctrl Pts',(7.59854716087849,2.61184571475234,3.0412639962152));
#19778=CARTESIAN_POINT('Ctrl Pts',(8.35457376462735,-1.22440681097471,3.23978011362686));
#19779=CARTESIAN_POINT('Ctrl Pts',(5.54079016364776,-3.93937031917242,3.43829623103851));
#19780=CARTESIAN_POINT('Ctrl Pts',(1.7340060207583,-3.04673371102089,3.63681234845017));
#19781=CARTESIAN_POINT('Ctrl Pts',(0.420401755326215,0.636043824414959,
3.83532846586182));
#19782=CARTESIAN_POINT('Ctrl Pts',(2.8029512110655,3.73634444619894,4.03384458327349));
#19783=CARTESIAN_POINT('Ctrl Pts',(6.6997608939274,3.41497193768155,4.23236070068513));
#19784=CARTESIAN_POINT('Ctrl Pts',(8.54220663371807,-0.0337669329441494,
4.4308768180968));
#19785=CARTESIAN_POINT('Ctrl Pts',(6.64301166261426,-3.45158267762228,4.62939293550844));
#19786=CARTESIAN_POINT('Ctrl Pts',(2.74142261194879,-3.70850466797209,4.82790905292011));
#19787=CARTESIAN_POINT('Ctrl Pts',(0.410440516499291,-0.569248623621048,
5.02642517033176));
#19788=CARTESIAN_POINT('Ctrl Pts',(1.78473444019877,3.09131448041513,5.22494128774342));
#19789=CARTESIAN_POINT('Ctrl Pts',(5.60575214909559,3.92091058714242,5.42345740515506));
#19790=CARTESIAN_POINT('Ctrl Pts',(8.37427830909092,1.15981136136555,5.62197352256674));
#19791=CARTESIAN_POINT('Ctrl Pts',(7.55494932568486,-2.66342104697584,5.82048963997839));
#19792=CARTESIAN_POINT('Ctrl Pts',(3.89809109665752,-4.04754312425325,6.01900575739004));
#19793=CARTESIAN_POINT('Ctrl Pts',(0.752584827297987,-1.72500220071308,
6.21752187480171));
#19794=CARTESIAN_POINT('Ctrl Pts',(0.999025325230166,2.17726292518741,6.41603799221334));
#19795=CARTESIAN_POINT('Ctrl Pts',(4.41172707023364,4.08563208015006,6.61455410962502));
#19796=CARTESIAN_POINT('Ctrl Pts',(7.86540272070975,2.25245709306557,6.81307022703666));
#19797=CARTESIAN_POINT('Ctrl Pts',(8.1972418118268,-1.64347525356681,7.01158634444832));
#19798=CARTESIAN_POINT('Ctrl Pts',(5.10335241618994,-4.03434422519923,7.21010246185998));
#19799=CARTESIAN_POINT('Ctrl Pts',(1.4170595903061,-2.73063749675737,7.40861857927163));
#19800=CARTESIAN_POINT('Ctrl Pts',(0.514200183395272,1.07373510898141,7.60713469668328));
#19801=CARTESIAN_POINT('Ctrl Pts',(3.22159566609925,3.89480152652282,7.80565081409495));
#19802=CARTESIAN_POINT('Ctrl Pts',(7.05986475548066,3.14908279305528,8.0041669315066));
#19803=CARTESIAN_POINT('Ctrl Pts',(8.51399363110384,-0.480506060385796,
8.20268304891826));
#19804=CARTESIAN_POINT('Ctrl Pts',(6.25231872913724,-3.67005660392007,8.40119916632992));
#19805=CARTESIAN_POINT('Ctrl Pts',(2.34603890318347,-3.49863912146337,8.59971528374156));
#19806=CARTESIAN_POINT('Ctrl Pts',(0.372450912529775,-0.123234482743352,
8.79823140115322));
#19807=CARTESIAN_POINT('Ctrl Pts',(2.13892909739252,3.36502595110463,8.99674751856487));
#19808=CARTESIAN_POINT('Ctrl Pts',(6.02776633805246,3.77165962851178,9.19526363597655));
#19809=CARTESIAN_POINT('Ctrl Pts',(8.47763946304124,0.72427916270141,9.39377975338818));
#19810=CARTESIAN_POINT('Ctrl Pts',(7.24500126602242,-2.98638238306039,9.59229587079984));
#19811=CARTESIAN_POINT('Ctrl Pts',(3.45867836056103,-3.9621717494319,9.79081198821151));
#19812=CARTESIAN_POINT('Ctrl Pts',(0.586113239980029,-1.30947959617202,
9.98932810562315));
#19813=CARTESIAN_POINT('Ctrl Pts',(1.25794639972494,2.54240906231909,10.1878442230349));
#19814=CARTESIAN_POINT('Ctrl Pts',(4.85892581172318,4.06600786328675,10.3863603404465));
#19815=CARTESIAN_POINT('Ctrl Pts',(8.09134302835829,1.86603400672705,10.5848764578582));
#19816=CARTESIAN_POINT('Ctrl Pts',(7.99501184973105,-2.04281829746266,10.7833925752698));
#19817=CARTESIAN_POINT('Ctrl Pts',(4.658150536815,-4.08089646336047,10.9819086926815));
#19818=CARTESIAN_POINT('Ctrl Pts',(1.13659320614603,-2.38176727499459,11.1804248100931));
#19819=CARTESIAN_POINT('Ctrl Pts',(0.655315074027438,1.49853907779376,11.3789409275048));
#19820=CARTESIAN_POINT('Ctrl Pts',(3.6550614989726,4.00651184837438,11.5774570449165));
#19821=CARTESIAN_POINT('Ctrl Pts',(7.38872176624422,2.84539728015019,11.7759731623281));
#19822=CARTESIAN_POINT('Ctrl Pts',(8.43708082482397,-0.921477992040132,
11.9744892797398));
#19823=CARTESIAN_POINT('Ctrl Pts',(5.84007139076835,-3.84448124749012,12.1730053971514));
#19824=CARTESIAN_POINT('Ctrl Pts',(1.97598530342792,-3.24678170627628,12.3715215145631));
#19825=CARTESIAN_POINT('Ctrl Pts',(0.383479098877827,0.324258761208613,
12.5700376319747));
#19826=CARTESIAN_POINT('Ctrl Pts',(2.52093966656498,3.59834922323431,12.7685537493864));
#19827=CARTESIAN_POINT('Ctrl Pts',(6.43092127741269,3.5771399144821,12.967069866798));
#19828=CARTESIAN_POINT('Ctrl Pts',(8.53273714794332,0.280053916463419,13.1655859842097));
#19829=CARTESIAN_POINT('Ctrl Pts',(6.90158428470204,-3.27350013106212,13.3641021016213));
#19830=CARTESIAN_POINT('Ctrl Pts',(3.0312414520278,-3.82924502713605,13.562618219033));
#19831=CARTESIAN_POINT('Ctrl Pts',(0.466094994356506,-0.878240167322765,
13.7611343364446));
#19832=CARTESIAN_POINT('Ctrl Pts',(1.55525724336407,2.87704033182534,13.9596504538563));
#19833=CARTESIAN_POINT('Ctrl Pts',(5.30129412947213,3.99758202219787,14.1581665712679));
#19834=CARTESIAN_POINT('Ctrl Pts',(8.27365632956023,1.45721413871475,14.3566826886797));
#19835=CARTESIAN_POINT('Ctrl Pts',(7.75031108111198,-2.41764273385123,14.5551988060912));
#19836=CARTESIAN_POINT('Ctrl Pts',(4.21052800757405,-4.07846837919741,14.753714923503));
#19837=CARTESIAN_POINT('Ctrl Pts',(0.895973113878727,-2.00431026356939,
14.9522310409146));
#19838=CARTESIAN_POINT('Ctrl Pts',(0.842052722152676,1.9053570654116,15.1507471583263));
#19839=CARTESIAN_POINT('Ctrl Pts',(4.09814610146403,4.07013463762311,15.3492632757379));
#19840=CARTESIAN_POINT('Ctrl Pts',(7.682384872503,2.50756033086961,15.5477793931496));
#19841=CARTESIAN_POINT('Ctrl Pts',(8.31239134820293,-1.35139002803904,15.7462955105612));
#19842=CARTESIAN_POINT('Ctrl Pts',(5.41121758211169,-3.97276310543362,15.9448116279729));
#19843=CARTESIAN_POINT('Ctrl Pts',(1.63570332303896,-2.95595530083938,16.1433277453845));
#19844=CARTESIAN_POINT('Ctrl Pts',(0.443392711547191,0.767860140031627,
16.3418438627962));
#19845=CARTESIAN_POINT('Ctrl Pts',(2.92618112548781,3.7884838709103,16.5403599802078));
#19846=CARTESIAN_POINT('Ctrl Pts',(6.8103781630174,3.33968613741389,16.7388760976195));
#19847=CARTESIAN_POINT('Ctrl Pts',(8.5389100624284,-0.167532633159739,16.9373922150311));
#19848=CARTESIAN_POINT('Ctrl Pts',(6.52882019040339,-3.5213282050942,17.1359083324428));
#19849=CARTESIAN_POINT('Ctrl Pts',(2.62091061577914,-3.65035838956845,17.3344244498544));
#19850=CARTESIAN_POINT('Ctrl Pts',(0.393970590674286,-0.43645979805503,
17.5329405672661));
#19851=CARTESIAN_POINT('Ctrl Pts',(1.88738942918871,3.17714037417117,17.7314566846778));
#19852=CARTESIAN_POINT('Ctrl Pts',(5.73352256684974,3.8811758273502,17.9299728020894));
#19853=CARTESIAN_POINT('Ctrl Pts',(8.41015443739666,1.03090428563328,18.1284889195011));
#19854=CARTESIAN_POINT('Ctrl Pts',(7.46607648872073,-2.76344979098553,18.3270050369127));
#19855=CARTESIAN_POINT('Ctrl Pts',(3.76585734795025,-4.02708911541293,18.5255211543244));
#19856=CARTESIAN_POINT('Ctrl Pts',(0.698087318576006,-1.60279683129456,
18.724037271736));
#19857=CARTESIAN_POINT('Ctrl Pts',(1.07217183831651,2.28930630247911,18.9225533891477));
#19858=CARTESIAN_POINT('Ctrl Pts',(4.54553141985243,4.08490627169594,19.1210695065593));
#19859=CARTESIAN_POINT('Ctrl Pts',(7.93732942868568,2.13962678039228,19.319585623971));
#19860=CARTESIAN_POINT('Ctrl Pts',(8.14142176722837,-1.76508221626667,19.5181017413827));
#19861=CARTESIAN_POINT('Ctrl Pts',(4.97090455397163,-4.05336249490537,19.7166178587943));
#19862=CARTESIAN_POINT('Ctrl Pts',(1.3292771434127,-2.62965050343175,19.915133976206));
#19863=CARTESIAN_POINT('Ctrl Pts',(0.551472646603815,1.20224539704524,20.1136500936177));
#19864=CARTESIAN_POINT('Ctrl Pts',(3.3497896271543,3.93314783354192,20.3121662110293));
#19865=CARTESIAN_POINT('Ctrl Pts',(7.16158262229433,3.06214829760668,20.510682328441));
#19866=CARTESIAN_POINT('Ctrl Pts',(8.49608411816253,-0.613108395518473,
20.7091984458526));
#19867=CARTESIAN_POINT('Ctrl Pts',(6.13118302381429,-3.72689209317441,20.9077145632643));
#19868=CARTESIAN_POINT('Ctrl Pts',(2.23261078765349,-3.42765888460072,21.1062306806759));
#19869=CARTESIAN_POINT('Ctrl Pts',(0.370605683008962,0.0105590905653954,
21.3047467980876));
#19870=CARTESIAN_POINT('Ctrl Pts',(2.250356607504,3.43910732612115,21.5032629154992));
#19871=CARTESIAN_POINT('Ctrl Pts',(6.15042334082164,3.71818634797007,21.7017790329109));
#19872=CARTESIAN_POINT('Ctrl Pts',(8.49919910975228,0.592221314373082,21.9002951503225));
#19873=CARTESIAN_POINT('Ctrl Pts',(7.14571944818345,-3.07608926032515,22.0988112677342));
#19874=CARTESIAN_POINT('Ctrl Pts',(3.32947585071529,-3.92737479389549,22.2973273851459));
#19875=CARTESIAN_POINT('Ctrl Pts',(0.545310524977601,-1.18204713458114,
22.4958435025575));
#19876=CARTESIAN_POINT('Ctrl Pts',(1.34291119900688,2.64578051982372,22.6943596199692));
#19877=CARTESIAN_POINT('Ctrl Pts',(4.99184635260365,4.05064557959106,22.8928757373808));
#19878=CARTESIAN_POINT('Ctrl Pts',(8.15049824324278,1.74602012818506,23.0913918547925));
#19879=CARTESIAN_POINT('Ctrl Pts',(7.92621886181009,-2.15760353803636,23.2899079722041));
#19880=CARTESIAN_POINT('Ctrl Pts',(4.52442717371885,-4.08528469325705,23.4884240896158));
#19881=CARTESIAN_POINT('Ctrl Pts',(1.06036526828869,-2.27183616857484,23.6869402070274));
#19882=CARTESIAN_POINT('Ctrl Pts',(0.706458758169362,1.62230144113535,23.8854563244391));
#19883=CARTESIAN_POINT('Ctrl Pts',(3.78660979300229,4.03041197296648,24.0839724418507));
#19884=CARTESIAN_POINT('Ctrl Pts',(7.48045570332662,2.74822735016753,24.2824885592624));
#19885=CARTESIAN_POINT('Ctrl Pts',(8.40451183040988,-1.05203519730533,24.481004676674));
#19886=CARTESIAN_POINT('Ctrl Pts',(5.71394743641032,-3.88635869185298,24.6795207940858));
#19887=CARTESIAN_POINT('Ctrl Pts',(1.87003416737941,-3.16648164392546,24.8780369114974));
#19888=CARTESIAN_POINT('Ctrl Pts',(0.398188145107553,0.462946646320358,
25.076553028909));
#19889=CARTESIAN_POINT('Ctrl Pts',(1.88978798161488,2.58492499113116,25.2088971071835));
#19890=CARTESIAN_POINT('Ctrl Pts',(2.91960708544911,3.09611134481228,25.2750691463207));
#19891=CARTESIAN_POINT('Ctrl Pts',(2.58997049159961,-2.62015330925654,0.00319355095334283));
#19892=CARTESIAN_POINT('Ctrl Pts',(1.71783944528228,-1.99894889552244,0.0694097009926075));
#19893=CARTESIAN_POINT('Ctrl Pts',(0.65845605968771,0.171475772890977,0.20179789016909));
#19894=CARTESIAN_POINT('Ctrl Pts',(2.5459024084217,3.29075405988094,0.400358118482792));
#19895=CARTESIAN_POINT('Ctrl Pts',(6.18433372098768,3.38626231280436,0.598874235894448));
#19896=CARTESIAN_POINT('Ctrl Pts',(8.23950371306965,0.385416781850904,0.797390353306103));
#19897=CARTESIAN_POINT('Ctrl Pts',(6.83072086642306,-2.97082408396747,0.995906470717762));
#19898=CARTESIAN_POINT('Ctrl Pts',(3.24739392835603,-3.60517206763711,1.19442258812942));
#19899=CARTESIAN_POINT('Ctrl Pts',(0.771445147794971,-0.938633334672633,
1.39293870554108));
#19900=CARTESIAN_POINT('Ctrl Pts',(1.6701033647243,2.58783275185508,1.59145482295273));
#19901=CARTESIAN_POINT('Ctrl Pts',(5.12049770482736,3.74423103498232,1.78997094036439));
#19902=CARTESIAN_POINT('Ctrl Pts',(7.96276883664299,1.47182751406662,1.98848705777604));
#19903=CARTESIAN_POINT('Ctrl Pts',(7.59404699250464,-2.14849653622342,2.1870031751877));
#19904=CARTESIAN_POINT('Ctrl Pts',(4.35198598660702,-3.80124283382013,2.38551929259936));
#19905=CARTESIAN_POINT('Ctrl Pts',(1.20561125008781,-1.97289654529749,2.58403541001101));
#19906=CARTESIAN_POINT('Ctrl Pts',(1.0363089362513,1.66219780307218,2.78255152742267));
#19907=CARTESIAN_POINT('Ctrl Pts',(3.99912495903867,3.77507940693446,2.98106764483432));
#19908=CARTESIAN_POINT('Ctrl Pts',(7.38076768128599,2.43081698451723,3.17958376224598));
#19909=CARTESIAN_POINT('Ctrl Pts',(8.08439358796167,-1.13954237620741,3.37809987965763));
#19910=CARTESIAN_POINT('Ctrl Pts',(5.4656351638386,-3.66632999264102,3.5766159970693));
#19911=CARTESIAN_POINT('Ctrl Pts',(1.92270171311447,-2.83556261008053,3.77513211448094));
#19912=CARTESIAN_POINT('Ctrl Pts',(0.700144216203009,0.591959212043988,
3.97364823189261));
#19913=CARTESIAN_POINT('Ctrl Pts',(2.91755761499276,3.47737597536012,4.17216434930425));
#19914=CARTESIAN_POINT('Ctrl Pts',(6.54427687678886,3.1782780050441,4.37068046671592));
#19915=CARTESIAN_POINT('Ctrl Pts',(8.2590215005,-0.0314265247951463,4.56919658412757));
#19916=CARTESIAN_POINT('Ctrl Pts',(6.49146097171637,-3.21235123071783,4.76771270153922));
#19917=CARTESIAN_POINT('Ctrl Pts',(2.86029360321679,-3.45146579032245,4.96622881895089));
#19918=CARTESIAN_POINT('Ctrl Pts',(0.690873397337037,-0.529793630188544,
5.16474493636253));
#19919=CARTESIAN_POINT('Ctrl Pts',(1.96991411271267,2.8770534572674,5.36326105377419));
#19920=CARTESIAN_POINT('Ctrl Pts',(5.52609459169944,3.64914971667956,5.56177717118585));
#19921=CARTESIAN_POINT('Ctrl Pts',(8.1027323975949,1.07942407934716,5.7602932885975));
#19922=CARTESIAN_POINT('Ctrl Pts',(7.34019164048911,-2.47881759682101,5.95880940600916));
#19923=CARTESIAN_POINT('Ctrl Pts',(3.93679264073839,-3.76700527003896,6.15732552342081));
#19924=CARTESIAN_POINT('Ctrl Pts',(1.00930346276847,-1.60544117293717,6.35584164083248));
#19925=CARTESIAN_POINT('Ctrl Pts',(1.23866300903221,2.02635541158186,6.55435775824412));
#19926=CARTESIAN_POINT('Ctrl Pts',(4.41482816993367,3.80245425555658,6.75287387565579));
#19927=CARTESIAN_POINT('Ctrl Pts',(7.6291273081915,2.09633782263408,6.95138999306744));
#19928=CARTESIAN_POINT('Ctrl Pts',(7.93796641543966,-1.5295649116789,7.14990611047909));
#19929=CARTESIAN_POINT('Ctrl Pts',(5.05851651200422,-3.75472119528823,7.34842222789076));
#19930=CARTESIAN_POINT('Ctrl Pts',(1.62772304650576,-2.54137523062185,7.5469383453024));
#19931=CARTESIAN_POINT('Ctrl Pts',(0.787441414036509,0.999313828164636,
7.74545446271406));
#19932=CARTESIAN_POINT('Ctrl Pts',(3.30718554976015,3.62485029208286,7.94397058012572));
#19933=CARTESIAN_POINT('Ctrl Pts',(6.8794217047968,2.93081781047529,8.14248669753737));
#19934=CARTESIAN_POINT('Ctrl Pts',(8.23276395950072,-0.447201871899268,
8.34100281494903));
#19935=CARTESIAN_POINT('Ctrl Pts',(6.12784722031342,-3.41568258667014,8.53951893236069));
#19936=CARTESIAN_POINT('Ctrl Pts',(2.49231419722064,-3.25614616174064,8.73803504977233));
#19937=CARTESIAN_POINT('Ctrl Pts',(0.655516877599837,-0.114693020356707,
8.93655116718401));
#19938=CARTESIAN_POINT('Ctrl Pts',(2.29955930716991,3.13179380737736,9.13506728459565));
#19939=CARTESIAN_POINT('Ctrl Pts',(5.9188587019336,3.51024343935022,9.33358340200731));
#19940=CARTESIAN_POINT('Ctrl Pts',(8.19892952254092,0.674078901476532,9.53209951941897));
#19941=CARTESIAN_POINT('Ctrl Pts',(7.05172628302556,-2.77939427202906,9.73061563683061));
#19942=CARTESIAN_POINT('Ctrl Pts',(3.52783588801619,-3.68755104089551,9.92913175424228));
#19943=CARTESIAN_POINT('Ctrl Pts',(0.854370129759403,-1.21871871116838,
10.1276478716539));
#19944=CARTESIAN_POINT('Ctrl Pts',(1.47963809495571,2.36619303175871,10.3261639890656));
#19945=CARTESIAN_POINT('Ctrl Pts',(4.83103127493619,3.78419020596524,10.5246801064772));
#19946=CARTESIAN_POINT('Ctrl Pts',(7.83940754573271,1.73669797247918,10.7231962238889));
#19947=CARTESIAN_POINT('Ctrl Pts',(7.74975314393437,-1.90122922870495,10.9217123413006));
#19948=CARTESIAN_POINT('Ctrl Pts',(4.64417186530054,-3.79804686745578,11.1202284587122));
#19949=CARTESIAN_POINT('Ctrl Pts',(1.36669597038421,-2.21668543150265,11.3187445761239));
#19950=CARTESIAN_POINT('Ctrl Pts',(0.91877553954763,1.39467435679268,11.5172606935355));
#19951=CARTESIAN_POINT('Ctrl Pts',(3.71060758300086,3.72881789865659,11.7157768109472));
#19952=CARTESIAN_POINT('Ctrl Pts',(7.18548542162604,2.64818093856821,11.9142929283589));
#19953=CARTESIAN_POINT('Ctrl Pts',(8.16118202999545,-0.857609751318129,
12.1128090457705));
#19954=CARTESIAN_POINT('Ctrl Pts',(5.74417301388192,-3.57801774441457,12.3113251631822));
#19955=CARTESIAN_POINT('Ctrl Pts',(2.14790925385559,-3.02174514829049,12.5098412805938));
#19956=CARTESIAN_POINT('Ctrl Pts',(0.665780693158256,0.301784174950485,
12.7083573980055));
#19957=CARTESIAN_POINT('Ctrl Pts',(2.65509247460188,3.34894529131551,12.9068735154171));
#19958=CARTESIAN_POINT('Ctrl Pts',(6.29407070946287,3.32920601358802,13.1053896328288));
#19959=CARTESIAN_POINT('Ctrl Pts',(8.25020835096136,0.260643196829997,13.3039057502404));
#19960=CARTESIAN_POINT('Ctrl Pts',(6.7321117566965,-3.04661170162563,13.5024218676521));
#19961=CARTESIAN_POINT('Ctrl Pts',(3.1300249104368,-3.56383755643203,13.7009379850637));
#19962=CARTESIAN_POINT('Ctrl Pts',(0.742670427029733,-0.817368768436538,
13.8994541024754));
#19963=CARTESIAN_POINT('Ctrl Pts',(1.75634213008195,2.67763078969056,14.0979702198871));
#19964=CARTESIAN_POINT('Ctrl Pts',(5.24273875601857,3.7205070045574,14.2964863372987));
#19965=CARTESIAN_POINT('Ctrl Pts',(8.0090845931027,1.35621367619806,14.4950024547104));
#19966=CARTESIAN_POINT('Ctrl Pts',(7.52201274521021,-2.25007433890389,14.693518572122));
#19967=CARTESIAN_POINT('Ctrl Pts',(4.22757434555207,-3.79578707538995,14.8920346895337));
#19968=CARTESIAN_POINT('Ctrl Pts',(1.14275341367199,-1.86539021176013,15.0905508069453));
#19969=CARTESIAN_POINT('Ctrl Pts',(1.09257027946957,1.77329552431533,15.289066924357));
#19970=CARTESIAN_POINT('Ctrl Pts',(4.12298170266298,3.78803095088039,15.4875830417686));
#19971=CARTESIAN_POINT('Ctrl Pts',(7.45879454642923,2.3337596886183,15.6860991591803));
#19972=CARTESIAN_POINT('Ctrl Pts',(8.04513486233581,-1.25772430366396,15.8846152765919));
#19973=CARTESIAN_POINT('Ctrl Pts',(5.34504334245093,-3.69740830310385,16.0831313940036));
#19974=CARTESIAN_POINT('Ctrl Pts',(1.83121243949837,-2.75107611072479,16.2816475114153));
#19975=CARTESIAN_POINT('Ctrl Pts',(0.721541654250978,0.714639252839528,
16.4801636288269));
#19976=CARTESIAN_POINT('Ctrl Pts',(3.03224638366176,3.52590158253341,16.6786797462386));
#19977=CARTESIAN_POINT('Ctrl Pts',(6.64722719080097,3.10821031270302,16.8771958636502));
#19978=CARTESIAN_POINT('Ctrl Pts',(8.25595341671681,-0.155920837071448,
17.0757119810619));
#19979=CARTESIAN_POINT('Ctrl Pts',(6.38518418493321,-3.27726265018464,17.2742280984735));
#19980=CARTESIAN_POINT('Ctrl Pts',(2.74813437211341,-3.39734966840464,17.4727442158852));
#19981=CARTESIAN_POINT('Ctrl Pts',(0.675545012814546,-0.406208484742623,
17.6712603332969));
#19982=CARTESIAN_POINT('Ctrl Pts',(2.06545401745235,2.9569307023417,17.8697764507085));
#19983=CARTESIAN_POINT('Ctrl Pts',(5.64500915845253,3.61216899900811,18.0682925681202));
#19984=CARTESIAN_POINT('Ctrl Pts',(8.13612192804524,0.959451637121888,18.2668086855318));
#19985=CARTESIAN_POINT('Ctrl Pts',(7.25747863782803,-2.57191328333314,18.4653248029435));
#19986=CARTESIAN_POINT('Ctrl Pts',(3.81372409941205,-3.74796894189382,18.6638409203551));
#19987=CARTESIAN_POINT('Ctrl Pts',(0.958583211925542,-1.49170593738941,
18.8623570377668));
#19988=CARTESIAN_POINT('Ctrl Pts',(1.306739689582,2.13063298930591,19.0608731551785));
#19989=CARTESIAN_POINT('Ctrl Pts',(4.53935845279781,3.80177875335989,19.2593892725901));
#19990=CARTESIAN_POINT('Ctrl Pts',(7.69606872911877,1.99132785253305,19.4579053900018));
#19991=CARTESIAN_POINT('Ctrl Pts',(7.88601529454458,-1.64274321646801,19.6564215074134));
#19992=CARTESIAN_POINT('Ctrl Pts',(4.93524869751396,-3.77242129631514,19.8549376248251));
#19993=CARTESIAN_POINT('Ctrl Pts',(1.54602485826833,-2.44738771167893,20.0534537422367));
#19994=CARTESIAN_POINT('Ctrl Pts',(0.822130498506685,1.11891698433359,20.2519698596484));
#19995=CARTESIAN_POINT('Ctrl Pts',(3.42649430375165,3.66053879154859,20.45048597706));
#19996=CARTESIAN_POINT('Ctrl Pts',(6.97408943990954,2.84990880161489,20.6490020944717));
#19997=CARTESIAN_POINT('Ctrl Pts',(8.21609576658401,-0.570613452685432,
20.8475182118833));
#19998=CARTESIAN_POINT('Ctrl Pts',(6.015107509745,-3.46857877108964,21.046034329295));
#19999=CARTESIAN_POINT('Ctrl Pts',(2.38674785836889,-3.19008561139642,21.2445504467067));
#20000=CARTESIAN_POINT('Ctrl Pts',(0.653799542140776,0.00982723311048271,
21.4430665641183));
#20001=CARTESIAN_POINT('Ctrl Pts',(2.40326370386975,3.2007405539671,21.64158268153));
#20002=CARTESIAN_POINT('Ctrl Pts',(6.03301426782987,3.46047642676426,21.8400987989417));
#20003=CARTESIAN_POINT('Ctrl Pts',(8.21899485607472,0.551174068759129,22.0386149163533));
#20004=CARTESIAN_POINT('Ctrl Pts',(6.95932575274402,-2.86288350711349,22.2371310337649));
#20005=CARTESIAN_POINT('Ctrl Pts',(3.40758848840856,-3.65516588504588,22.4356471511766));
#20006=CARTESIAN_POINT('Ctrl Pts',(0.816395477550012,-1.10011867661645,
22.6341632685882));
#20007=CARTESIAN_POINT('Ctrl Pts',(1.55871392857562,2.46239974611297,22.8326793859999));
#20008=CARTESIAN_POINT('Ctrl Pts',(4.95473900642221,3.76989269217354,23.0311955034116));
#20009=CARTESIAN_POINT('Ctrl Pts',(7.89446267408575,1.62500233414576,23.2297116208232));
#20010=CARTESIAN_POINT('Ctrl Pts',(7.68572824288089,-2.00805862937836,23.4282277382349));
#20011=CARTESIAN_POINT('Ctrl Pts',(4.5197169557303,-3.80213094627573,23.6267438556465));
#20012=CARTESIAN_POINT('Ctrl Pts',(1.29575144062437,-2.11437372177854,23.8252599730582));
#20013=CARTESIAN_POINT('Ctrl Pts',(0.966374421579891,1.50985866999905,24.0237760904698));
#20014=CARTESIAN_POINT('Ctrl Pts',(3.83303817896047,3.7510614900228,24.2222922078815));
#20015=CARTESIAN_POINT('Ctrl Pts',(7.27086121968984,2.55774591981802,24.4208083252931));
#20016=CARTESIAN_POINT('Ctrl Pts',(8.13087041382945,-0.979117951521988,
24.6193244427048));
#20017=CARTESIAN_POINT('Ctrl Pts',(5.62679079307294,-3.61699263579137,24.8178405601165));
#20018=CARTESIAN_POINT('Ctrl Pts',(2.04930166016011,-2.94701073564213,25.0163566775281));
#20019=CARTESIAN_POINT('Ctrl Pts',(0.679470245798868,0.430859512276974,
25.2148727949398));
#20020=CARTESIAN_POINT('Ctrl Pts',(2.06768632464525,2.40576215381105,25.3472168732142));
#20021=CARTESIAN_POINT('Ctrl Pts',(3.02612799462649,2.8815178478641,25.4133889123514));
#20022=CARTESIAN_POINT('Ctrl Pts',(6.37918160141763,2.58636699315934,3.1286030352177));
#20023=CARTESIAN_POINT('Ctrl Pts',(6.30741621831574,2.63971758075101,3.12256282893198));
#20024=CARTESIAN_POINT('Ctrl Pts',(6.23342241705917,2.69008701405223,3.11654829135272));
#20025=CARTESIAN_POINT('Ctrl Pts',(6.07812215225983,2.78658711682447,3.10441138359402));
#20026=CARTESIAN_POINT('Ctrl Pts',(5.99675027082823,2.83237759333759,3.09830425807943));
#20027=CARTESIAN_POINT('Ctrl Pts',(5.87725019107504,2.89294836706277,3.08970510167227));
#20028=CARTESIAN_POINT('Ctrl Pts',(5.84065556149054,2.91063519540686,3.08711917555247));
#20029=CARTESIAN_POINT('Ctrl Pts',(5.77476040826474,2.94095952209419,3.08254573546535));
#20030=CARTESIAN_POINT('Ctrl Pts',(5.74558885575873,2.95386276872368,3.08054945346403));
#20031=CARTESIAN_POINT('Ctrl Pts',(5.70078278328311,2.97289129927177,3.07752534154838));
#20032=CARTESIAN_POINT('Ctrl Pts',(5.68528464289493,2.97933072989385,3.07648689840741));
#20033=CARTESIAN_POINT('Ctrl Pts',(5.66962384056547,2.98569475463646,3.07544503925855));
#20034=CARTESIAN_POINT('Ctrl Pts',(5.66951100782513,2.9857405986252,3.07543753327549));
#20035=CARTESIAN_POINT('Ctrl Pts',(5.66927747768848,2.98583546659269,3.07542199893488));
#20036=CARTESIAN_POINT('Ctrl Pts',(5.66915677994456,2.98588448963843,3.07541397061041));
#20037=CARTESIAN_POINT('Ctrl Pts',(5.66890694243952,2.98598594692363,3.07539735335573));
#20038=CARTESIAN_POINT('Ctrl Pts',(5.66877780222149,2.98603838011524,3.07538876445963));
#20039=CARTESIAN_POINT('Ctrl Pts',(5.66851045644071,2.98614690698533,3.07537098480326));
#20040=CARTESIAN_POINT('Ctrl Pts',(5.66837225039046,2.98620299944473,3.07536179408465));
#20041=CARTESIAN_POINT('Ctrl Pts',(5.66808609964525,2.98631911376347,3.07534276623617));
#20042=CARTESIAN_POINT('Ctrl Pts',(5.66793815437648,2.98637913422672,3.0753329291533));
#20043=CARTESIAN_POINT('Ctrl Pts',(5.66763179751311,2.9865033947639,3.07531256045323));
#20044=CARTESIAN_POINT('Ctrl Pts',(5.66747338527249,2.98656763322601,3.07530202889102));
#20045=CARTESIAN_POINT('Ctrl Pts',(5.66714530760974,2.98670064308427,3.07528021922124));
#20046=CARTESIAN_POINT('Ctrl Pts',(5.66697564141815,2.98676941263535,3.07526894117525));
#20047=CARTESIAN_POINT('Ctrl Pts',(5.66662420452476,2.9869118231053,3.07524558229451));
#20048=CARTESIAN_POINT('Ctrl Pts',(5.66644243297915,2.98698546188136,3.07523350153351));
#20049=CARTESIAN_POINT('Ctrl Pts',(5.66606586392061,2.9871379764623,3.0752084763802));
#20050=CARTESIAN_POINT('Ctrl Pts',(5.66587106538793,2.98721684981588,3.07519553206976));
#20051=CARTESIAN_POINT('Ctrl Pts',(5.66546744449525,2.9873802287776,3.07516871396948));
#20052=CARTESIAN_POINT('Ctrl Pts',(5.66525862099383,2.98746473154354,3.07515484027637));
#20053=CARTESIAN_POINT('Ctrl Pts',(5.66482586918937,2.98763979659986,3.07512609212352));
#20054=CARTESIAN_POINT('Ctrl Pts',(5.66460193955519,2.9877303556142,3.07511121777453));
#20055=CARTESIAN_POINT('Ctrl Pts',(5.6641378041319,2.98791799514358,3.07508039111529));
#20056=CARTESIAN_POINT('Ctrl Pts',(5.66389759679584,2.98801507187713,3.07506443893236));
#20057=CARTESIAN_POINT('Ctrl Pts',(5.66339963639431,2.98821624637538,3.0750313729991));
#20058=CARTESIAN_POINT('Ctrl Pts',(5.6631418815587,2.9883203397603,3.07501425939714));
#20059=CARTESIAN_POINT('Ctrl Pts',(5.66260745005453,2.98853608762625,3.07497878007606));
#20060=CARTESIAN_POINT('Ctrl Pts',(5.6623307713298,2.9886477370428,3.07496041452798));
#20061=CARTESIAN_POINT('Ctrl Pts',(5.6617570005945,2.98887918069369,3.07492233325841));
#20062=CARTESIAN_POINT('Ctrl Pts',(5.66145990620808,2.98899896906207,3.07490261773515));
#20063=CARTESIAN_POINT('Ctrl Pts',(5.66092414283189,2.98921489583492,3.07486706870618));
#20064=CARTESIAN_POINT('Ctrl Pts',(5.66068548022041,2.98931104993951,3.07485123467112));
#20065=CARTESIAN_POINT('Ctrl Pts',(5.66011191373954,2.98954205268078,3.07481318565032));
#20066=CARTESIAN_POINT('Ctrl Pts',(5.65977699866029,2.98967687364897,3.07479097159834));
#20067=CARTESIAN_POINT('Ctrl Pts',(5.65897213208931,2.99000071770139,3.07473759506564));
#20068=CARTESIAN_POINT('Ctrl Pts',(5.65850215856685,2.99018968631521,3.07470643442356));
#20069=CARTESIAN_POINT('Ctrl Pts',(5.65678508330488,2.99087962376996,3.07459261171173));
#20070=CARTESIAN_POINT('Ctrl Pts',(5.65553771149205,2.99137992381229,3.07450997221269));
#20071=CARTESIAN_POINT('Ctrl Pts',(5.64115186888314,2.9971394016061,3.07355744020205));
#20072=CARTESIAN_POINT('Ctrl Pts',(5.62797904602356,3.00231282711055,3.0726904470855));
#20073=CARTESIAN_POINT('Ctrl Pts',(5.59742155520105,3.0140820795246,3.07069108338549));
#20074=CARTESIAN_POINT('Ctrl Pts',(5.58001292423118,3.0206146037519,3.06956084978733));
#20075=CARTESIAN_POINT('Ctrl Pts',(5.52316140676146,3.04138842854456,3.06589760916342));
#20076=CARTESIAN_POINT('Ctrl Pts',(5.48349593535826,3.05501099402468,3.06338507493675));
#20077=CARTESIAN_POINT('Ctrl Pts',(5.24854294857735,3.13060885443019,3.04873495747833));
#20078=CARTESIAN_POINT('Ctrl Pts',(5.04796525040568,3.17462406827909,3.03720476709825));
#20079=CARTESIAN_POINT('Ctrl Pts',(4.63887649500039,3.22424682531855,3.01415537300919));
#20080=CARTESIAN_POINT('Ctrl Pts',(4.43130577231929,3.22930105445226,3.00267951248));
#20081=CARTESIAN_POINT('Ctrl Pts',(4.19223620995792,3.2120646007964,2.98837875207932));
#20082=CARTESIAN_POINT('Ctrl Pts',(4.1597945784986,3.20923075863535,2.9864143575472));
#20083=CARTESIAN_POINT('Ctrl Pts',(4.11549503930727,3.20468368787138,2.98369260973874));
#20084=CARTESIAN_POINT('Ctrl Pts',(4.10359429724189,3.20339510712159,2.98295753886961));
#20085=CARTESIAN_POINT('Ctrl Pts',(4.08361598010529,3.20111923058502,2.98171658371324));
#20086=CARTESIAN_POINT('Ctrl Pts',(4.07553432314849,3.20016756918412,2.98121267470738));
#20087=CARTESIAN_POINT('Ctrl Pts',(4.06015685945751,3.19829770925481,2.9802500622131));
#20088=CARTESIAN_POINT('Ctrl Pts',(4.05286044277384,3.19738513135089,2.97979169207905));
#20089=CARTESIAN_POINT('Ctrl Pts',(4.03551478953637,3.19515535594678,2.97869825952451));
#20090=CARTESIAN_POINT('Ctrl Pts',(4.02546858800257,3.19381571669535,2.97806196649877));
#20091=CARTESIAN_POINT('Ctrl Pts',(3.98991932947084,3.1889045193157,2.97580015828257));
#20092=CARTESIAN_POINT('Ctrl Pts',(3.96445370251704,3.18507479869402,2.97416124471114));
#20093=CARTESIAN_POINT('Ctrl Pts',(3.73354710376588,3.1475141030085,2.95914719429602));
#20094=CARTESIAN_POINT('Ctrl Pts',(3.53179628582646,3.09425724726375,2.94495688384999));
#20095=CARTESIAN_POINT('Ctrl Pts',(3.12245455097615,2.94256399556581,2.91545991982143));
#20096=CARTESIAN_POINT('Ctrl Pts',(2.91730732113421,2.84065043100939,2.90028322806361));
#20097=CARTESIAN_POINT('Ctrl Pts',(2.69790851115881,2.70084919901108,2.88388698218973));
#20098=CARTESIAN_POINT('Ctrl Pts',(2.67143566419799,2.68342644549244,2.88190427482752));
#20099=CARTESIAN_POINT('Ctrl Pts',(2.63131027830807,2.65616184759386,2.87889144865722));
#20100=CARTESIAN_POINT('Ctrl Pts',(2.61747125921,2.64659922231818,2.87785092388267));
#20101=CARTESIAN_POINT('Ctrl Pts',(2.59241816647276,2.62899639125184,2.87596441246112));
#20102=CARTESIAN_POINT('Ctrl Pts',(2.5811797214581,2.62099173290751,2.87511710091933));
#20103=CARTESIAN_POINT('Ctrl Pts',(2.55677377061703,2.60337108892213,2.87327455540356));
#20104=CARTESIAN_POINT('Ctrl Pts',(2.54362708372376,2.5937268181082,2.87228044056938));
#20105=CARTESIAN_POINT('Ctrl Pts',(2.50774061716639,2.56697962664781,2.86956197260998));
#20106=CARTESIAN_POINT('Ctrl Pts',(2.48515292268647,2.54967443228986,2.86784552822854));
#20107=CARTESIAN_POINT('Ctrl Pts',(2.36017613199945,2.45127171250288,2.85831254494002));
#20108=CARTESIAN_POINT('Ctrl Pts',(2.2625556945755,2.3643026245916,2.85073616686963));
#20109=CARTESIAN_POINT('Ctrl Pts',(2.01559144488247,2.11577774383062,2.83080029611922));
#20110=CARTESIAN_POINT('Ctrl Pts',(1.87706289127506,1.94449379476505,2.81878285706658));
#20111=CARTESIAN_POINT('Ctrl Pts',(1.69966627522793,1.67247945703279,2.80024810077018));
#20112=CARTESIAN_POINT('Ctrl Pts',(1.64663236578805,1.58175922024594,2.79413722795883));
#20113=CARTESIAN_POINT('Ctrl Pts',(1.59014539348432,1.47329715792194,2.78672200435909));
#20114=CARTESIAN_POINT('Ctrl Pts',(1.58228742048877,1.45790800427642,2.78566739911584));
#20115=CARTESIAN_POINT('Ctrl Pts',(1.57039380379087,1.43414549275553,2.78403401280563));
#20116=CARTESIAN_POINT('Ctrl Pts',(1.56626986278352,1.4258163534841,2.78346055499314));
#20117=CARTESIAN_POINT('Ctrl Pts',(1.55873910949178,1.41043954299495,2.78239994589603));
#20118=CARTESIAN_POINT('Ctrl Pts',(1.55532189262773,1.40339719231727,2.78191344691955));
#20119=CARTESIAN_POINT('Ctrl Pts',(1.54762732448303,1.38739168360427,2.78080606040031));
#20120=CARTESIAN_POINT('Ctrl Pts',(1.54336575165569,1.37842121079492,2.78018423162992));
#20121=CARTESIAN_POINT('Ctrl Pts',(1.53240116583824,1.35506316324844,2.77856227815285));
#20122=CARTESIAN_POINT('Ctrl Pts',(1.5257629514458,1.34064570526993,2.77755841617804));
#20123=CARTESIAN_POINT('Ctrl Pts',(1.48113244221961,1.24179759375036,2.77066013185173));
#20124=CARTESIAN_POINT('Ctrl Pts',(1.44669071043467,1.15582015859053,2.76458329457475));
#20125=CARTESIAN_POINT('Ctrl Pts',(1.38869762157164,0.990796268431566,2.75292599013063));
#20126=CARTESIAN_POINT('Ctrl Pts',(1.36438349275767,0.912088182955032,2.74736875828496));
#20127=CARTESIAN_POINT('Ctrl Pts',(1.30882384929709,0.704317436087036,2.73282385412915));
#20128=CARTESIAN_POINT('Ctrl Pts',(1.28248865597636,0.574094932078838,2.72383562217646));
#20129=CARTESIAN_POINT('Ctrl Pts',(1.2508203206929,0.345697770631459,2.70849869969516));
#20130=CARTESIAN_POINT('Ctrl Pts',(1.24180200072098,0.248212341007797,2.7020832132299));
#20131=CARTESIAN_POINT('Ctrl Pts',(1.23527469584318,0.108554355449584,2.69309941890341));
#20132=CARTESIAN_POINT('Ctrl Pts',(1.23413448035723,0.0666130458958216,
2.69042765331163));
#20133=CARTESIAN_POINT('Ctrl Pts',(1.23356090963365,-0.00834375021116602,
2.68569865564482));
#20134=CARTESIAN_POINT('Ctrl Pts',(1.23381536220876,-0.0413501889883888,
2.68363217820089));
#20135=CARTESIAN_POINT('Ctrl Pts',(1.23497111062394,-0.0914349446359473,
2.68051956925222));
#20136=CARTESIAN_POINT('Ctrl Pts',(1.23550133759388,-0.108518828846837,
2.67946193803549));
#20137=CARTESIAN_POINT('Ctrl Pts',(1.2367107390131,-0.139527593404653,2.67754941078168));
#20138=CARTESIAN_POINT('Ctrl Pts',(1.23734440303871,-0.153453731036658,
2.67669311465616));
#20139=CARTESIAN_POINT('Ctrl Pts',(1.23890609070547,-0.183482838240074,
2.6748521559889));
#20140=CARTESIAN_POINT('Ctrl Pts',(1.23986468595636,-0.199583889762953,
2.67386847260931));
#20141=CARTESIAN_POINT('Ctrl Pts',(1.24279664800391,-0.243296405000552,
2.67120672575759));
#20142=CARTESIAN_POINT('Ctrl Pts',(1.24500497259703,-0.270891122387398,
2.66953602686988));
#20143=CARTESIAN_POINT('Ctrl Pts',(1.25842914610231,-0.415224071405668,
2.66084307307456));
#20144=CARTESIAN_POINT('Ctrl Pts',(1.27565585472896,-0.531321008860896,
2.65401152422393));
#20145=CARTESIAN_POINT('Ctrl Pts',(1.30331604619479,-0.666460605696267,
2.64612661267374));
#20146=CARTESIAN_POINT('Ctrl Pts',(1.30765106493071,-0.686650507227025,
2.64495025211349));
#20147=CARTESIAN_POINT('Ctrl Pts',(1.35935395958566,-0.916658171206028,
2.63155920811023));
#20148=CARTESIAN_POINT('Ctrl Pts',(1.42741642687149,-1.12125714703055,2.61978619998866));
#20149=CARTESIAN_POINT('Ctrl Pts',(1.55778818771961,-1.41228301117058,2.60157650003628));
#20150=CARTESIAN_POINT('Ctrl Pts',(1.60477755459001,-1.50490702726582,2.59553343467051));
#20151=CARTESIAN_POINT('Ctrl Pts',(1.66467872842147,-1.61006866754962,2.58819446978672));
#20152=CARTESIAN_POINT('Ctrl Pts',(1.67332922825673,-1.62497600520683,2.58714249670317));
#20153=CARTESIAN_POINT('Ctrl Pts',(1.68682299455371,-1.64780587028186,2.58551234586619));
#20154=CARTESIAN_POINT('Ctrl Pts',(1.69158177488011,-1.65577830942292,2.58493945869309));
#20155=CARTESIAN_POINT('Ctrl Pts',(1.70041631222551,-1.67043462760341,2.58387937591637));
#20156=CARTESIAN_POINT('Ctrl Pts',(1.70448203217375,-1.67712432114842,2.58339282777401));
#20157=CARTESIAN_POINT('Ctrl Pts',(1.71376709020406,-1.69227718744503,2.58228464975907));
#20158=CARTESIAN_POINT('Ctrl Pts',(1.71900121778882,-1.7007310138355,2.58166207275952));
#20159=CARTESIAN_POINT('Ctrl Pts',(1.73271280215099,-1.72264979961774,2.58003688685625));
#20160=CARTESIAN_POINT('Ctrl Pts',(1.74125089231552,-1.73607625498422,2.57903051681592));
#20161=CARTESIAN_POINT('Ctrl Pts',(1.80066398761422,-1.82799509605761,2.57206877508557));
#20162=CARTESIAN_POINT('Ctrl Pts',(1.85483145816809,-1.90429647461469,2.5659272563331));
#20163=CARTESIAN_POINT('Ctrl Pts',(2.08422358152577,-2.19933697750453,2.54101240626791));
#20164=CARTESIAN_POINT('Ctrl Pts',(2.28436635280362,-2.39721522570006,2.52172622563897));
#20165=CARTESIAN_POINT('Ctrl Pts',(2.57818580305259,-2.62031054042873,2.49771522136086));
#20166=CARTESIAN_POINT('Ctrl Pts',(2.65097210029443,-2.67098455573032,2.49204668875813));
#20167=CARTESIAN_POINT('Ctrl Pts',(2.74665962795413,-2.73190095811372,2.48493854416513));
#20168=CARTESIAN_POINT('Ctrl Pts',(2.76771096851286,-2.74496398961727,2.48339505347836));
#20169=CARTESIAN_POINT('Ctrl Pts',(2.80203223493242,-2.76571714131716,2.48091071307703));
#20170=CARTESIAN_POINT('Ctrl Pts',(2.81520977258424,-2.77355736907932,2.47996439918888));
#20171=CARTESIAN_POINT('Ctrl Pts',(2.84059051386314,-2.78841389688691,2.47815594770866));
#20172=CARTESIAN_POINT('Ctrl Pts',(2.85278468263975,-2.79544485996068,2.47729329309791));
#20173=CARTESIAN_POINT('Ctrl Pts',(2.88076266824742,-2.81133319713251,2.47532798519566));
#20174=CARTESIAN_POINT('Ctrl Pts',(2.89657590831167,-2.82013800297365,2.47422723637995));
#20175=CARTESIAN_POINT('Ctrl Pts',(2.94685108544774,-2.84757894589775,2.47075855783552));
#20176=CARTESIAN_POINT('Ctrl Pts',(2.98157988881301,-2.86572057576469,2.46840813149915));
#20177=CARTESIAN_POINT('Ctrl Pts',(3.25096246978223,-3.0002459839599,2.4505022776045));
#20178=CARTESIAN_POINT('Ctrl Pts',(3.49868123701998,-3.08826468039805,2.43601843119229));
#20179=CARTESIAN_POINT('Ctrl Pts',(3.87332352426088,-3.17189551675349,2.41450529306424));
#20180=CARTESIAN_POINT('Ctrl Pts',(3.99370935379962,-3.19168122391711,2.40762930714677));
#20181=CARTESIAN_POINT('Ctrl Pts',(4.15422487698384,-3.20878928709383,2.39819188963642));
#20182=CARTESIAN_POINT('Ctrl Pts',(4.19360528869756,-3.21225506458201,2.39585503409401));
#20183=CARTESIAN_POINT('Ctrl Pts',(4.26024427348816,-3.21688625083731,2.39184954874845));
#20184=CARTESIAN_POINT('Ctrl Pts',(4.28747274326101,-3.21843152065529,2.39019854321635));
#20185=CARTESIAN_POINT('Ctrl Pts',(4.32587031984897,-3.22012207349703,2.38784594822452));
#20186=CARTESIAN_POINT('Ctrl Pts',(4.33702641884141,-3.22055517684282,2.38715952706558));
#20187=CARTESIAN_POINT('Ctrl Pts',(4.35616458891464,-3.22119858476464,2.3859766729185));
#20188=CARTESIAN_POINT('Ctrl Pts',(4.36414572619566,-3.22143721203675,2.38548180520032));
#20189=CARTESIAN_POINT('Ctrl Pts',(4.37966778272985,-3.22184357340249,2.38451616088276));
#20190=CARTESIAN_POINT('Ctrl Pts',(4.38720847410977,-3.22201449668491,2.38404558958097));
#20191=CARTESIAN_POINT('Ctrl Pts',(4.40782620165717,-3.22240942316101,2.38275510190075));
#20192=CARTESIAN_POINT('Ctrl Pts',(4.42090394251223,-3.22258029039911,2.38193231311119));
#20193=CARTESIAN_POINT('Ctrl Pts',(4.47159336370544,-3.22293398871823,2.37872769417013));
#20194=CARTESIAN_POINT('Ctrl Pts',(4.50920448875094,-3.22253796461204,2.37631687487083));
#20195=CARTESIAN_POINT('Ctrl Pts',(4.76491580081086,-3.21536793090091,2.35973963632905));
#20196=CARTESIAN_POINT('Ctrl Pts',(4.98183567129539,-3.18711650140904,2.34479680709835));
#20197=CARTESIAN_POINT('Ctrl Pts',(5.32851967263839,-3.10558814585225,2.32080385518719));
#20198=CARTESIAN_POINT('Ctrl Pts',(5.46065884560665,-3.06541348662698,2.31162117477715));
#20199=CARTESIAN_POINT('Ctrl Pts',(5.66357210137934,-2.98918477646024,2.29757783869267));
#20200=CARTESIAN_POINT('Ctrl Pts',(5.73628040224296,-2.9587848926759,2.29255597163309));
#20201=CARTESIAN_POINT('Ctrl Pts',(5.82942901312241,-2.91576163516891,2.28613207406645));
#20202=CARTESIAN_POINT('Ctrl Pts',(5.8509403031124,-2.90553522591516,2.28464918053248));
#20203=CARTESIAN_POINT('Ctrl Pts',(5.88592404100724,-2.88842602875519,2.28223806835214));
#20204=CARTESIAN_POINT('Ctrl Pts',(5.89946459113835,-2.88168533624427,2.28130496590441));
#20205=CARTESIAN_POINT('Ctrl Pts',(5.9255793475553,-2.86845478744269,2.27950540600963));
#20206=CARTESIAN_POINT('Ctrl Pts',(5.93815922901359,-2.86197696686913,2.27863855392636));
#20207=CARTESIAN_POINT('Ctrl Pts',(5.96715234031196,-2.84680499682379,2.27664054066455));
#20208=CARTESIAN_POINT('Ctrl Pts',(5.98353398891745,-2.83805133676436,2.27551150651134));
#20209=CARTESIAN_POINT('Ctrl Pts',(6.0365476703471,-2.80913114818228,2.27185658251019));
#20210=CARTESIAN_POINT('Ctrl Pts',(6.07286399447933,-2.7883927061523,2.26935103130209));
#20211=CARTESIAN_POINT('Ctrl Pts',(6.20193433149682,-2.71131775386986,2.2604271230675));
#20212=CARTESIAN_POINT('Ctrl Pts',(6.29218331063479,-2.65104180749099,2.25415409453453));
#20213=CARTESIAN_POINT('Ctrl Pts',(6.3791823737616,-2.58636641899648,2.24798337798073));
#20214=CARTESIAN_POINT('Ctrl Pts',(2.17296269996979,-3.20554048108048,-0.411765747138983));
#20215=CARTESIAN_POINT('Ctrl Pts',(1.10598262521586,-2.44554835076675,-0.345549597099719));
#20216=CARTESIAN_POINT('Ctrl Pts',(-0.190085171851759,0.209786400507346,
-0.213161407923235));
#20217=CARTESIAN_POINT('Ctrl Pts',(2.11904905146237,4.02596493684606,-0.0146011796095345));
#20218=CARTESIAN_POINT('Ctrl Pts',(6.57036830017086,4.14281137096193,0.183914937802122));
#20219=CARTESIAN_POINT('Ctrl Pts',(9.08469850437939,0.471525498888313,0.382431055213778));
#20220=CARTESIAN_POINT('Ctrl Pts',(7.36116941620609,-3.63455711911314,0.580947172625436));
#20221=CARTESIAN_POINT('Ctrl Pts',(2.97726580402431,-4.41062931823268,0.77946329003709));
#20222=CARTESIAN_POINT('Ctrl Pts',(-0.0518523842630756,-1.14834011450979,
0.977979407448747));
#20223=CARTESIAN_POINT('Ctrl Pts',(1.04758148582589,3.16599895701937,1.1764955248604));
#20224=CARTESIAN_POINT('Ctrl Pts',(5.26885307852876,4.58075644304919,1.37501164227206));
#20225=CARTESIAN_POINT('Ctrl Pts',(8.74613631193873,1.80065901519612,1.57352775968371));
#20226=CARTESIAN_POINT('Ctrl Pts',(8.2950356860829,-2.62850749839492,1.77204387709537));
#20227=CARTESIAN_POINT('Ctrl Pts',(4.32864266632258,-4.6505056552148,1.97055999450703));
#20228=CARTESIAN_POINT('Ctrl Pts',(0.479313869061077,-2.41367545883394,
2.16907611191868));
#20229=CARTESIAN_POINT('Ctrl Pts',(0.272186515624751,2.03356129066451,2.36759222933034));
#20230=CARTESIAN_POINT('Ctrl Pts',(3.89694643539194,4.61849687019083,2.56610834674199));
#20231=CARTESIAN_POINT('Ctrl Pts',(8.03410612006349,2.97390317522259,2.76462446415365));
#20232=CARTESIAN_POINT('Ctrl Pts',(8.89493411795877,-1.39413568050936,2.9631405815653));
#20233=CARTESIAN_POINT('Ctrl Pts',(5.69110016326603,-4.48545097223521,3.16165669897696));
#20234=CARTESIAN_POINT('Ctrl Pts',(1.35661463604595,-3.46907591290164,3.36017281638862));
#20235=CARTESIAN_POINT('Ctrl Pts',(-0.139083166427389,0.724213049156903,
3.55868893380027));
#20236=CARTESIAN_POINT('Ctrl Pts',(2.57373840321099,4.25428138787658,3.75720505121192));
#20237=CARTESIAN_POINT('Ctrl Pts',(7.01072892820446,3.88835980295648,3.95572116862359));
#20238=CARTESIAN_POINT('Ctrl Pts',(9.10857690015422,-0.0384477492421469,
4.15423728603523));
#20239=CARTESIAN_POINT('Ctrl Pts',(6.94611304441007,-3.93004557143118,4.3527534034469));
#20240=CARTESIAN_POINT('Ctrl Pts',(2.50368062941278,-4.22258242327136,4.55126952085854));
#20241=CARTESIAN_POINT('Ctrl Pts',(-0.15042524517621,-0.648158610486061,
4.74978563827021));
#20242=CARTESIAN_POINT('Ctrl Pts',(1.41437509517098,3.51983652671062,4.94830175568186));
#20243=CARTESIAN_POINT('Ctrl Pts',(5.76506726388787,4.46443232806813,5.14681787309352));
#20244=CARTESIAN_POINT('Ctrl Pts',(8.91737013208296,1.32058592540232,5.34533399050517));
#20245=CARTESIAN_POINT('Ctrl Pts',(7.98446469607637,-3.03262794728552,5.54385010791683));
#20246=CARTESIAN_POINT('Ctrl Pts',(3.82068800849579,-4.60861883268182,5.74236622532849));
#20247=CARTESIAN_POINT('Ctrl Pts',(0.239147556357015,-1.9641242562649,5.94088234274014));
#20248=CARTESIAN_POINT('Ctrl Pts',(0.519749957626067,2.47907795239849,6.13939846015179));
#20249=CARTESIAN_POINT('Ctrl Pts',(4.40552487083362,4.65198772933701,6.33791457756345));
#20250=CARTESIAN_POINT('Ctrl Pts',(8.33795354574623,2.56469563392857,6.53643069497511));
#20251=CARTESIAN_POINT('Ctrl Pts',(8.71579260460107,-1.87129593734266,6.73494681238676));
#20252=CARTESIAN_POINT('Ctrl Pts',(5.19302422456139,-4.59359028502123,6.93346292979842));
#20253=CARTESIAN_POINT('Ctrl Pts',(0.995732677906764,-3.10916202902842,
7.13197904721008));
#20254=CARTESIAN_POINT('Ctrl Pts',(-0.0322822778871914,1.22257767061497,
7.33049516462173));
#20255=CARTESIAN_POINT('Ctrl Pts',(3.05041589877745,4.43470399540276,7.52901128203338));
#20256=CARTESIAN_POINT('Ctrl Pts',(7.42075085684839,3.58561275821527,7.72752739944505));
#20257=CARTESIAN_POINT('Ctrl Pts',(9.07645297431008,-0.547114437358846,
7.9260435168567));
#20258=CARTESIAN_POINT('Ctrl Pts',(6.5012617467849,-4.17880463841992,8.12455963426836));
#20259=CARTESIAN_POINT('Ctrl Pts',(2.05348831510913,-3.98362504090881,8.32307575168001));
#20260=CARTESIAN_POINT('Ctrl Pts',(-0.193681017610346,-0.140317407516647,
8.52159186909167));
#20261=CARTESIAN_POINT('Ctrl Pts',(1.81766867783776,3.83149023855917,8.72010798650331));
#20262=CARTESIAN_POINT('Ctrl Pts',(6.24558161029013,4.2944920068349,8.91862410391498));
#20263=CARTESIAN_POINT('Ctrl Pts',(9.03505934404192,0.824679685151172,9.11714022132663));
#20264=CARTESIAN_POINT('Ctrl Pts',(7.6315512320161,-3.40035860512303,9.31565633873829));
#20265=CARTESIAN_POINT('Ctrl Pts',(3.32036330565075,-4.51141316650472,9.51417245614994));
#20266=CARTESIAN_POINT('Ctrl Pts',(0.0495994604212725,-1.49100136617927,
9.71268857356161));
#20267=CARTESIAN_POINT('Ctrl Pts',(0.814563009263402,2.89484112343983,9.91120469097325));
#20268=CARTESIAN_POINT('Ctrl Pts',(4.91471488529713,4.62964317792977,10.1097208083849));
#20269=CARTESIAN_POINT('Ctrl Pts',(8.59521399360942,2.1247060752228,10.3082369257966));
#20270=CARTESIAN_POINT('Ctrl Pts',(8.48552926132444,-2.32599643497811,10.5067530432082));
#20271=CARTESIAN_POINT('Ctrl Pts',(4.68610787984395,-4.64659565516981,10.7052691606199));
#20272=CARTESIAN_POINT('Ctrl Pts',(0.676387677669684,-2.71193096197848,
10.9037852780315));
#20273=CARTESIAN_POINT('Ctrl Pts',(0.128394142987057,1.70626851979591,11.1023013954432));
#20274=CARTESIAN_POINT('Ctrl Pts',(3.54396933091606,4.56189974780998,11.3008175128549));
#20275=CARTESIAN_POINT('Ctrl Pts',(7.79519445548059,3.23982996331418,11.4993336302665));
#20276=CARTESIAN_POINT('Ctrl Pts',(8.98887841448097,-1.04921447348414,11.6978497476782));
#20277=CARTESIAN_POINT('Ctrl Pts',(6.03186814454124,-4.3774082536412,11.8963658650898));
#20278=CARTESIAN_POINT('Ctrl Pts',(1.63213740257258,-3.69685482224785,12.0948819825015));
#20279=CARTESIAN_POINT('Ctrl Pts',(-0.181124089683036,0.369207933724872,
12.2933980999131));
#20280=CARTESIAN_POINT('Ctrl Pts',(2.2526340504912,4.09715708707193,12.4919142173248));
#20281=CARTESIAN_POINT('Ctrl Pts',(6.70462241331237,4.07300771627025,12.6904303347364));
#20282=CARTESIAN_POINT('Ctrl Pts',(9.09779474190718,0.318875355730261,12.8889464521481));
#20283=CARTESIAN_POINT('Ctrl Pts',(7.24052934071316,-3.72727698993507,13.0874625695597));
#20284=CARTESIAN_POINT('Ctrl Pts',(2.83367453520978,-4.36005996854408,13.2859786869714));
#20285=CARTESIAN_POINT('Ctrl Pts',(-0.0870558709899348,-0.999982965095223,
13.4844948043831));
#20286=CARTESIAN_POINT('Ctrl Pts',(1.1530874699283,3.2758594160949,13.6830109217947));
#20287=CARTESIAN_POINT('Ctrl Pts',(5.41840487637927,4.55173205747878,13.8815270392064));
#20288=CARTESIAN_POINT('Ctrl Pts',(8.80279980247531,1.65921506374814,14.080043156618));
#20289=CARTESIAN_POINT('Ctrl Pts',(8.20690775291552,-2.75277952374592,14.2785592740297));
#20290=CARTESIAN_POINT('Ctrl Pts',(4.17643533161801,-4.64383098681233,14.4770753914414));
#20291=CARTESIAN_POINT('Ctrl Pts',(0.402412514292184,-2.28215036718792,
14.675591508853));
#20292=CARTESIAN_POINT('Ctrl Pts',(0.341017607518878,2.16948014760412,14.8741076262646));
#20293=CARTESIAN_POINT('Ctrl Pts',(4.04847489906614,4.63434201110855,15.0726237436763));
#20294=CARTESIAN_POINT('Ctrl Pts',(8.12956552465056,2.85516161537223,15.271139861088));
#20295=CARTESIAN_POINT('Ctrl Pts',(8.84690431993714,-1.53872147678918,15.4696559784996));
#20296=CARTESIAN_POINT('Ctrl Pts',(5.54356606143321,-4.52347271009317,15.6681720959113));
#20297=CARTESIAN_POINT('Ctrl Pts',(1.24468509012015,-3.36571368106855,15.8666882133229));
#20298=CARTESIAN_POINT('Ctrl Pts',(-0.112905173860372,0.874301914415817,
16.0652043307346));
#20299=CARTESIAN_POINT('Ctrl Pts',(2.71405060913991,4.31364844766405,16.2637204481462));
#20300=CARTESIAN_POINT('Ctrl Pts',(7.1366801074503,3.80263778683562,16.4622365655579));
#20301=CARTESIAN_POINT('Ctrl Pts',(9.10482335385156,-0.190756225336315,
16.6607526829696));
#20302=CARTESIAN_POINT('Ctrl Pts',(6.81609220134375,-4.00945931491334,16.8592688003812));
#20303=CARTESIAN_POINT('Ctrl Pts',(2.36646310311057,-4.15637583189606,17.0577849177929));
#20304=CARTESIAN_POINT('Ctrl Pts',(-0.16917825360623,-0.496962424679848,
17.2563010352045));
#20305=CARTESIAN_POINT('Ctrl Pts',(1.53126025266144,3.61755971783011,17.4548171526162));
#20306=CARTESIAN_POINT('Ctrl Pts',(5.91054938364417,4.41918948403437,17.6533332700278));
#20307=CARTESIAN_POINT('Ctrl Pts',(8.95821945609951,1.17380958265607,17.8518493874395));
#20308=CARTESIAN_POINT('Ctrl Pts',(7.88327219050615,-3.14652280629029,18.0503655048511));
#20309=CARTESIAN_POINT('Ctrl Pts',(3.67012384502666,-4.58532946245115,18.2488816222628));
#20310=CARTESIAN_POINT('Ctrl Pts',(0.177095531876928,-1.82497861910485,
18.4473977396744));
#20311=CARTESIAN_POINT('Ctrl Pts',(0.603036135785551,2.60665292882547,18.6459138570862));
#20312=CARTESIAN_POINT('Ctrl Pts',(4.55787735396168,4.65116130836808,18.8444299744978));
#20313=CARTESIAN_POINT('Ctrl Pts',(8.41985082781949,2.43622463611074,19.0429460919094));
#20314=CARTESIAN_POINT('Ctrl Pts',(8.65223471259592,-2.00976021586402,19.2414622093211));
#20315=CARTESIAN_POINT('Ctrl Pts',(5.04221626688697,-4.61524489208584,19.4399783267328));
#20316=CARTESIAN_POINT('Ctrl Pts',(0.895781713701428,-2.99417608693739,
19.6384944441444));
#20317=CARTESIAN_POINT('Ctrl Pts',(0.0101569427980723,1.36890222246852,
19.8370105615561));
#20318=CARTESIAN_POINT('Ctrl Pts',(3.1963802739596,4.47836591752857,20.0355266789677));
#20319=CARTESIAN_POINT('Ctrl Pts',(7.53656898706393,3.48662728959027,20.2340427963793));
#20320=CARTESIAN_POINT('Ctrl Pts',(9.05606082131957,-0.698098281184544,
20.432558913791));
#20321=CARTESIAN_POINT('Ctrl Pts',(6.36333405195284,-4.24351873734398,20.6310750312027));
#20322=CARTESIAN_POINT('Ctrl Pts',(1.9243366462227,-3.90280543100934,20.8295911486144));
#20323=CARTESIAN_POINT('Ctrl Pts',(-0.195782035254683,0.0120228054752082,
21.028107266026));
#20324=CARTESIAN_POINT('Ctrl Pts',(1.94454241477252,3.91584087042925,21.2266233834376));
#20325=CARTESIAN_POINT('Ctrl Pts',(6.38524148680512,4.23360619038166,21.4251395008493));
#20326=CARTESIAN_POINT('Ctrl Pts',(9.05960761710739,0.674315805600993,21.623655618261));
#20327=CARTESIAN_POINT('Ctrl Pts',(7.5185068390623,-3.50250076674849,21.8221717356726));
#20328=CARTESIAN_POINT('Ctrl Pts',(3.17325057532877,-4.47179261159471,22.0206878530843));
#20329=CARTESIAN_POINT('Ctrl Pts',(0.0031406198327811,-1.34590405051051,
22.2192039704959));
#20330=CARTESIAN_POINT('Ctrl Pts',(0.911305739869395,3.01254206724522,22.4177200879076));
#20331=CARTESIAN_POINT('Ctrl Pts',(5.06606104496655,4.6121513544261,22.6162362053192));
#20332=CARTESIAN_POINT('Ctrl Pts',(8.66256938155685,1.98805571626367,22.8147523227309));
#20333=CARTESIAN_POINT('Ctrl Pts',(8.4072000996685,-2.45669335535235,23.0132684401425));
#20334=CARTESIAN_POINT('Ctrl Pts',(4.53384760969594,-4.65159218721967,23.2117845575542));
#20335=CARTESIAN_POINT('Ctrl Pts',(0.589592923617338,-2.58676106216746,
23.4103006749659));
#20336=CARTESIAN_POINT('Ctrl Pts',(0.186627431348294,1.84718698340797,23.6088167923775));
#20337=CARTESIAN_POINT('Ctrl Pts',(3.69375302108596,4.58911293885384,23.8073329097892));
#20338=CARTESIAN_POINT('Ctrl Pts',(7.89964467060016,3.12919021086655,24.0058490272008));
#20339=CARTESIAN_POINT('Ctrl Pts',(8.95179466357075,-1.19786968887199,24.2043651446125));
#20340=CARTESIAN_POINT('Ctrl Pts',(5.88826072308503,-4.42509080397621,24.4028812620241));
#20341=CARTESIAN_POINT('Ctrl Pts',(1.51149918181804,-3.60542346049212,24.6013973794358));
#20342=CARTESIAN_POINT('Ctrl Pts',(-0.164376056275096,0.527120914407128,
24.7999134968474));
#20343=CARTESIAN_POINT('Ctrl Pts',(1.53399129555416,2.94325066577138,24.9322575751219));
#20344=CARTESIAN_POINT('Ctrl Pts',(2.70656526709436,3.52529833870864,24.9984296142591));
#20345=CARTESIAN_POINT('Ctrl Pts',(2.31196529717974,-3.01041142380583,-0.273445981108207));
#20346=CARTESIAN_POINT('Ctrl Pts',(1.30993489857133,-2.29668186568531,-0.207229831068943));
#20347=CARTESIAN_POINT('Ctrl Pts',(0.0927619053280601,0.197016191301887,
-0.0748416418924601));
#20348=CARTESIAN_POINT('Ctrl Pts',(2.26133350378215,3.78089464452436,0.123718586421241));
#20349=CARTESIAN_POINT('Ctrl Pts',(6.44169010710979,3.89062835157607,0.322234703832897));
#20350=CARTESIAN_POINT('Ctrl Pts',(8.80296690727615,0.442822593209179,0.520750821244553));
#20351=CARTESIAN_POINT('Ctrl Pts',(7.18435323294509,-3.41331277406459,0.719266938656211));
#20352=CARTESIAN_POINT('Ctrl Pts',(3.06730851213489,-4.14214356803415,0.917783056067867));
#20353=CARTESIAN_POINT('Ctrl Pts',(0.222580126422941,-1.07843785456408,
1.11629917347952));
#20354=CARTESIAN_POINT('Ctrl Pts',(1.25508877879203,2.97327688863128,1.31481529089117));
#20355=CARTESIAN_POINT('Ctrl Pts',(5.21940128729496,4.30191464036023,1.51333140830283));
#20356=CARTESIAN_POINT('Ctrl Pts',(8.48501382017349,1.69104851481962,1.71184752571448));
#20357=CARTESIAN_POINT('Ctrl Pts',(8.06137278822348,-2.46850384433775,1.91036364312614));
#20358=CARTESIAN_POINT('Ctrl Pts',(4.33642377308406,-4.36741804808325,2.1088797605378));
#20359=CARTESIAN_POINT('Ctrl Pts',(0.721412996069988,-2.26674915432179,
2.30739587794946));
#20360=CARTESIAN_POINT('Ctrl Pts',(0.526893989166935,1.90977346146706,2.50591199536111));
#20361=CARTESIAN_POINT('Ctrl Pts',(3.93100594327419,4.33735771577206,2.70442811277276));
#20362=CARTESIAN_POINT('Ctrl Pts',(7.81632664047099,2.79287444498747,2.90294423018442));
#20363=CARTESIAN_POINT('Ctrl Pts',(8.62475394129306,-1.30927124574203,3.10146034759608));
#20364=CARTESIAN_POINT('Ctrl Pts',(5.61594516345689,-4.21241064570382,3.29997646500774));
#20365=CARTESIAN_POINT('Ctrl Pts',(1.54531032840212,-3.25790481196126,3.49849258241939));
#20366=CARTESIAN_POINT('Ctrl Pts',(0.140659294449413,0.680128436785933,
3.69700869983105));
#20367=CARTESIAN_POINT('Ctrl Pts',(2.68834480713824,3.99531291703776,3.8955248172427));
#20368=CARTESIAN_POINT('Ctrl Pts',(6.85524491106594,3.65166587031902,4.09404093465435));
#20369=CARTESIAN_POINT('Ctrl Pts',(8.82539176693615,-0.0361073410931478,
4.29255705206602));
#20370=CARTESIAN_POINT('Ctrl Pts',(6.79456235351217,-3.69081412452673,4.49107316947766));
#20371=CARTESIAN_POINT('Ctrl Pts',(2.62255162068078,-3.96554354562172,4.68958928688933));
#20372=CARTESIAN_POINT('Ctrl Pts',(0.130007635661538,-0.608703617053558,
4.88810540430098));
#20373=CARTESIAN_POINT('Ctrl Pts',(1.59955476768487,3.30557550356288,5.08662152171263));
#20374=CARTESIAN_POINT('Ctrl Pts',(5.68540970649173,4.19267145760527,5.28513763912429));
#20375=CARTESIAN_POINT('Ctrl Pts',(8.64582422058695,1.24019864338394,5.48365375653594));
#20376=CARTESIAN_POINT('Ctrl Pts',(7.76970701088062,-2.84802449713069,5.68216987394761));
#20377=CARTESIAN_POINT('Ctrl Pts',(3.85938955257665,-4.32808097846753,5.88068599135924));
#20378=CARTESIAN_POINT('Ctrl Pts',(0.495866191827503,-1.844563228489,6.07920210877092));
#20379=CARTESIAN_POINT('Ctrl Pts',(0.759387641428115,2.32817043879295,6.27771822618256));
#20380=CARTESIAN_POINT('Ctrl Pts',(4.40862597053364,4.36880990474354,6.47623434359423));
#20381=CARTESIAN_POINT('Ctrl Pts',(8.10167813322798,2.40857636349708,6.67475046100588));
#20382=CARTESIAN_POINT('Ctrl Pts',(8.45651720821394,-1.75738559545474,6.87326657841754));
#20383=CARTESIAN_POINT('Ctrl Pts',(5.14818832037566,-4.31396725511023,7.0717826958292));
#20384=CARTESIAN_POINT('Ctrl Pts',(1.20639613410644,-2.9198997628929,7.27029881324085));
#20385=CARTESIAN_POINT('Ctrl Pts',(0.240958952754043,1.14815638979818,7.4688149306525));
#20386=CARTESIAN_POINT('Ctrl Pts',(3.13600578243834,4.16475276096279,7.66733104806417));
#20387=CARTESIAN_POINT('Ctrl Pts',(7.24030780616454,3.36734777563528,7.86584716547581));
#20388=CARTESIAN_POINT('Ctrl Pts',(8.79522330270695,-0.513810248872322,
8.06436328288747));
#20389=CARTESIAN_POINT('Ctrl Pts',(6.37679023796107,-3.92443062116999,8.26287940029913));
#20390=CARTESIAN_POINT('Ctrl Pts',(2.1997636091463,-3.74113208118609,8.46139551771078));
#20391=CARTESIAN_POINT('Ctrl Pts',(0.089384947459713,-0.131775945129999,
8.65991163512245));
#20392=CARTESIAN_POINT('Ctrl Pts',(1.97829888761515,3.5982580948319,8.8584277525341));
#20393=CARTESIAN_POINT('Ctrl Pts',(6.13667397417128,4.03307581767334,9.05694386994575));
#20394=CARTESIAN_POINT('Ctrl Pts',(8.75634940354159,0.774479423926291,9.2554599873574));
#20395=CARTESIAN_POINT('Ctrl Pts',(7.43827624901926,-3.19337049409171,9.45397610476906));
#20396=CARTESIAN_POINT('Ctrl Pts',(3.38952083310589,-4.23679245796831,9.65249222218073));
#20397=CARTESIAN_POINT('Ctrl Pts',(0.317856350200649,-1.40024048117564,
9.85100833959237));
#20398=CARTESIAN_POINT('Ctrl Pts',(1.03625470449417,2.71862509287945,10.049524457004));
#20399=CARTESIAN_POINT('Ctrl Pts',(4.88682034851015,4.34782552060827,10.2480405744157));
#20400=CARTESIAN_POINT('Ctrl Pts',(8.34327851098385,1.99537004097493,10.4465566918273));
#20401=CARTESIAN_POINT('Ctrl Pts',(8.24027055552775,-2.18440736622039,10.645072809239));
#20402=CARTESIAN_POINT('Ctrl Pts',(4.67212920832948,-4.36374605926514,10.8435889266506));
#20403=CARTESIAN_POINT('Ctrl Pts',(0.906490441907856,-2.54684911848653,
11.0421050440623));
#20404=CARTESIAN_POINT('Ctrl Pts',(0.391854608507251,1.60240379879482,11.2406211614739));
#20405=CARTESIAN_POINT('Ctrl Pts',(3.59951541494433,4.28420579809219,11.4391372788856));
#20406=CARTESIAN_POINT('Ctrl Pts',(7.59195811086242,3.04261362173219,11.6376533962972));
#20407=CARTESIAN_POINT('Ctrl Pts',(8.71297961965247,-0.98534623276214,11.8361695137089));
#20408=CARTESIAN_POINT('Ctrl Pts',(5.93596976765481,-4.11094475056566,12.0346856311206));
#20409=CARTESIAN_POINT('Ctrl Pts',(1.80406135300024,-3.47181826426207,12.2332017485322));
#20410=CARTESIAN_POINT('Ctrl Pts',(0.101177504597399,0.346733347466743,
12.4317178659439));
#20411=CARTESIAN_POINT('Ctrl Pts',(2.38678685852808,3.84775315515312,12.6302339833555));
#20412=CARTESIAN_POINT('Ctrl Pts',(6.56777184536255,3.82507381537617,12.8287501007672));
#20413=CARTESIAN_POINT('Ctrl Pts',(8.81526594492522,0.29946463609684,13.0272662181788));
#20414=CARTESIAN_POINT('Ctrl Pts',(7.07105681270762,-3.5003885604986,13.2257823355905));
#20415=CARTESIAN_POINT('Ctrl Pts',(2.93245799361878,-4.09465249784007,13.4242984530022));
#20416=CARTESIAN_POINT('Ctrl Pts',(0.189519561683291,-0.939111566208993,
13.6228145704138));
#20417=CARTESIAN_POINT('Ctrl Pts',(1.35417235664619,3.07644987396012,13.8213306878255));
#20418=CARTESIAN_POINT('Ctrl Pts',(5.3598495029257,4.27465703983832,14.0198468052371));
#20419=CARTESIAN_POINT('Ctrl Pts',(8.53822806601778,1.55821460123144,14.2183629226488));
#20420=CARTESIAN_POINT('Ctrl Pts',(7.97860941701375,-2.58521112879858,14.4168790400604));
#20421=CARTESIAN_POINT('Ctrl Pts',(4.19348166959603,-4.36114968300486,14.6153951574721));
#20422=CARTESIAN_POINT('Ctrl Pts',(0.649192814085452,-2.14323031537866,
14.8139112748837));
#20423=CARTESIAN_POINT('Ctrl Pts',(0.59153516483578,2.03741860650786,15.0124273922954));
#20424=CARTESIAN_POINT('Ctrl Pts',(4.07331050026509,4.35223832436584,15.2109435097071));
#20425=CARTESIAN_POINT('Ctrl Pts',(7.9059751985768,2.68136097312093,15.4094596271187));
#20426=CARTESIAN_POINT('Ctrl Pts',(8.57964783407003,-1.44505575241412,15.6079757445304));
#20427=CARTESIAN_POINT('Ctrl Pts',(5.47739182177246,-4.24811790776339,15.806491861942));
#20428=CARTESIAN_POINT('Ctrl Pts',(1.44019420657955,-3.16083449095397,16.0050079793537));
#20429=CARTESIAN_POINT('Ctrl Pts',(0.165243768843413,0.821081027223728,
16.2035240967653));
#20430=CARTESIAN_POINT('Ctrl Pts',(2.82011586731386,4.05106615928717,16.402040214177));
#20431=CARTESIAN_POINT('Ctrl Pts',(6.97352913523386,3.57116196212476,16.6005563315886));
#20432=CARTESIAN_POINT('Ctrl Pts',(8.82186670813997,-0.17914442924803,16.7990724490003));
#20433=CARTESIAN_POINT('Ctrl Pts',(6.67245619587356,-3.76539376000376,16.997588566412));
#20434=CARTESIAN_POINT('Ctrl Pts',(2.49368685944485,-3.90336711073225,17.1961046838236));
#20435=CARTESIAN_POINT('Ctrl Pts',(0.112396168534027,-0.466711111367439,
17.3946208012353));
#20436=CARTESIAN_POINT('Ctrl Pts',(1.70932484092508,3.39735004600064,17.5931369186469));
#20437=CARTESIAN_POINT('Ctrl Pts',(5.82203597524696,4.15018265569229,17.7916530360586));
#20438=CARTESIAN_POINT('Ctrl Pts',(8.68418694674809,1.10235693414467,17.9901691534703));
#20439=CARTESIAN_POINT('Ctrl Pts',(7.67467433961344,-2.9549862986379,18.1886852708819));
#20440=CARTESIAN_POINT('Ctrl Pts',(3.71799059648846,-4.30620928893205,18.3872013882936));
#20441=CARTESIAN_POINT('Ctrl Pts',(0.437591425226463,-1.7138877251997,18.5857175057052));
#20442=CARTESIAN_POINT('Ctrl Pts',(0.837603987051035,2.44797961565228,18.7842336231169));
#20443=CARTESIAN_POINT('Ctrl Pts',(4.55170438690705,4.36803379003202,18.9827497405285));
#20444=CARTESIAN_POINT('Ctrl Pts',(8.17859012825258,2.28792570825151,19.1812658579402));
#20445=CARTESIAN_POINT('Ctrl Pts',(8.39682823991214,-1.88742121606535,19.3797819753518));
#20446=CARTESIAN_POINT('Ctrl Pts',(5.0065604104293,-4.33430369349561,19.5782980927635));
#20447=CARTESIAN_POINT('Ctrl Pts',(1.11252942855707,-2.81191329518458,19.7768142101752));
#20448=CARTESIAN_POINT('Ctrl Pts',(0.280814794700937,1.28557380975688,19.9753303275868));
#20449=CARTESIAN_POINT('Ctrl Pts',(3.27308495055695,4.20575687553525,20.1738464449984));
#20450=CARTESIAN_POINT('Ctrl Pts',(7.34907580467911,3.27438779359847,20.3723625624101));
#20451=CARTESIAN_POINT('Ctrl Pts',(8.77607246974106,-0.65560333835151,20.5708786798217));
#20452=CARTESIAN_POINT('Ctrl Pts',(6.24725853788356,-3.98520541525919,20.7693947972334));
#20453=CARTESIAN_POINT('Ctrl Pts',(2.07847371693811,-3.66523215780504,20.9679109146451));
#20454=CARTESIAN_POINT('Ctrl Pts',(0.0874118238771355,0.0112909480203034,
21.1664270320568));
#20455=CARTESIAN_POINT('Ctrl Pts',(2.09744951113826,3.6774740982752,21.3649431494684));
#20456=CARTESIAN_POINT('Ctrl Pts',(6.26783241381338,3.97589626917586,21.56345926688));
#20457=CARTESIAN_POINT('Ctrl Pts',(8.77940336342984,0.633268559987037,21.7619753842917));
#20458=CARTESIAN_POINT('Ctrl Pts',(7.33211314362288,-3.28929501353682,21.9604915017033));
#20459=CARTESIAN_POINT('Ctrl Pts',(3.25136321302202,-4.1995837027451,22.159007619115));
#20460=CARTESIAN_POINT('Ctrl Pts',(0.274225572405194,-1.26397559254583,
22.3575237365266));
#20461=CARTESIAN_POINT('Ctrl Pts',(1.12710846943813,2.82916129353447,22.5560398539383));
#20462=CARTESIAN_POINT('Ctrl Pts',(5.0289536987851,4.33139846700858,22.75455597135));
#20463=CARTESIAN_POINT('Ctrl Pts',(8.40653381239982,1.86703792222437,22.9530720887616));
#20464=CARTESIAN_POINT('Ctrl Pts',(8.1667094807393,-2.30714844669435,23.1515882061733));
#20465=CARTESIAN_POINT('Ctrl Pts',(4.52913739170739,-4.36843844023836,23.3501043235849));
#20466=CARTESIAN_POINT('Ctrl Pts',(0.824979095953012,-2.42929861537115,
23.5486204409966));
#20467=CARTESIAN_POINT('Ctrl Pts',(0.44654309475883,1.73474421227166,23.7471365584082));
#20468=CARTESIAN_POINT('Ctrl Pts',(3.74018140704413,4.30976245591016,23.9456526758199));
#20469=CARTESIAN_POINT('Ctrl Pts',(7.69005018696339,2.93870878051704,24.1441687932315));
#20470=CARTESIAN_POINT('Ctrl Pts',(8.67815324699032,-1.12495244308866,24.3426849106432));
#20471=CARTESIAN_POINT('Ctrl Pts',(5.80110407974766,-4.15572474791461,24.5412010280549));
#20472=CARTESIAN_POINT('Ctrl Pts',(1.69076667459873,-3.38595255220879,24.7397171454665));
#20473=CARTESIAN_POINT('Ctrl Pts',(0.116906044416222,0.495033780363739,
24.9382332628782));
#20474=CARTESIAN_POINT('Ctrl Pts',(1.71188963858453,2.76408782845127,25.0705773411526));
#20475=CARTESIAN_POINT('Ctrl Pts',(2.81308617627174,3.31070484176046,25.1367493802898));
#20476=CARTESIAN_POINT('Ctrl Pts',(2.45096789438968,-2.81528236653118,-0.135126215077433));
#20477=CARTESIAN_POINT('Ctrl Pts',(1.5138871719268,-2.14781538060387,-0.0689100650381678));
#20478=CARTESIAN_POINT('Ctrl Pts',(0.375608982507884,0.184245982096433,
0.0634781241383155));
#20479=CARTESIAN_POINT('Ctrl Pts',(2.40361795610193,3.53582435220265,0.262038352452016));
#20480=CARTESIAN_POINT('Ctrl Pts',(6.31301191404873,3.63844533219021,0.460554469863673));
#20481=CARTESIAN_POINT('Ctrl Pts',(8.52123531017291,0.41411968753004,0.659070587275328));
#20482=CARTESIAN_POINT('Ctrl Pts',(7.00753704968407,-3.19206842901602,0.857586704686986));
#20483=CARTESIAN_POINT('Ctrl Pts',(3.15735122024546,-3.87365781783563,1.05610282209864));
#20484=CARTESIAN_POINT('Ctrl Pts',(0.497012637108953,-1.00853559461836,
1.25461893951029));
#20485=CARTESIAN_POINT('Ctrl Pts',(1.46259607175817,2.78055482024318,1.45313505692195));
#20486=CARTESIAN_POINT('Ctrl Pts',(5.16994949606116,4.02307283767128,1.6516511743336));
#20487=CARTESIAN_POINT('Ctrl Pts',(8.22389132840824,1.58143801444312,1.85016729174526));
#20488=CARTESIAN_POINT('Ctrl Pts',(7.82770989036406,-2.30850019028058,2.04868340915692));
#20489=CARTESIAN_POINT('Ctrl Pts',(4.34420487984554,-4.08433044095169,2.24719952656857));
#20490=CARTESIAN_POINT('Ctrl Pts',(0.963512123078899,-2.11982284980964,
2.44571564398023));
#20491=CARTESIAN_POINT('Ctrl Pts',(0.781601462709117,1.78598563226962,2.64423176139188));
#20492=CARTESIAN_POINT('Ctrl Pts',(3.96506545115642,4.05621856135326,2.84274787880354));
#20493=CARTESIAN_POINT('Ctrl Pts',(7.59854716087849,2.61184571475234,3.0412639962152));
#20494=CARTESIAN_POINT('Ctrl Pts',(8.35457376462735,-1.22440681097471,3.23978011362686));
#20495=CARTESIAN_POINT('Ctrl Pts',(5.54079016364776,-3.93937031917242,3.43829623103851));
#20496=CARTESIAN_POINT('Ctrl Pts',(1.7340060207583,-3.04673371102089,3.63681234845017));
#20497=CARTESIAN_POINT('Ctrl Pts',(0.420401755326215,0.636043824414959,
3.83532846586182));
#20498=CARTESIAN_POINT('Ctrl Pts',(2.8029512110655,3.73634444619894,4.03384458327349));
#20499=CARTESIAN_POINT('Ctrl Pts',(6.6997608939274,3.41497193768155,4.23236070068513));
#20500=CARTESIAN_POINT('Ctrl Pts',(8.54220663371807,-0.0337669329441494,
4.4308768180968));
#20501=CARTESIAN_POINT('Ctrl Pts',(6.64301166261426,-3.45158267762228,4.62939293550844));
#20502=CARTESIAN_POINT('Ctrl Pts',(2.74142261194879,-3.70850466797209,4.82790905292011));
#20503=CARTESIAN_POINT('Ctrl Pts',(0.410440516499291,-0.569248623621048,
5.02642517033176));
#20504=CARTESIAN_POINT('Ctrl Pts',(1.78473444019877,3.09131448041513,5.22494128774342));
#20505=CARTESIAN_POINT('Ctrl Pts',(5.60575214909559,3.92091058714242,5.42345740515506));
#20506=CARTESIAN_POINT('Ctrl Pts',(8.37427830909092,1.15981136136555,5.62197352256674));
#20507=CARTESIAN_POINT('Ctrl Pts',(7.55494932568486,-2.66342104697584,5.82048963997839));
#20508=CARTESIAN_POINT('Ctrl Pts',(3.89809109665752,-4.04754312425325,6.01900575739004));
#20509=CARTESIAN_POINT('Ctrl Pts',(0.752584827297987,-1.72500220071308,
6.21752187480171));
#20510=CARTESIAN_POINT('Ctrl Pts',(0.999025325230166,2.17726292518741,6.41603799221334));
#20511=CARTESIAN_POINT('Ctrl Pts',(4.41172707023364,4.08563208015006,6.61455410962502));
#20512=CARTESIAN_POINT('Ctrl Pts',(7.86540272070975,2.25245709306557,6.81307022703666));
#20513=CARTESIAN_POINT('Ctrl Pts',(8.1972418118268,-1.64347525356681,7.01158634444832));
#20514=CARTESIAN_POINT('Ctrl Pts',(5.10335241618994,-4.03434422519923,7.21010246185998));
#20515=CARTESIAN_POINT('Ctrl Pts',(1.4170595903061,-2.73063749675737,7.40861857927163));
#20516=CARTESIAN_POINT('Ctrl Pts',(0.514200183395272,1.07373510898141,7.60713469668328));
#20517=CARTESIAN_POINT('Ctrl Pts',(3.22159566609925,3.89480152652282,7.80565081409495));
#20518=CARTESIAN_POINT('Ctrl Pts',(7.05986475548066,3.14908279305528,8.0041669315066));
#20519=CARTESIAN_POINT('Ctrl Pts',(8.51399363110384,-0.480506060385796,
8.20268304891826));
#20520=CARTESIAN_POINT('Ctrl Pts',(6.25231872913724,-3.67005660392007,8.40119916632992));
#20521=CARTESIAN_POINT('Ctrl Pts',(2.34603890318347,-3.49863912146337,8.59971528374156));
#20522=CARTESIAN_POINT('Ctrl Pts',(0.372450912529775,-0.123234482743352,
8.79823140115322));
#20523=CARTESIAN_POINT('Ctrl Pts',(2.13892909739252,3.36502595110463,8.99674751856487));
#20524=CARTESIAN_POINT('Ctrl Pts',(6.02776633805246,3.77165962851178,9.19526363597655));
#20525=CARTESIAN_POINT('Ctrl Pts',(8.47763946304124,0.72427916270141,9.39377975338818));
#20526=CARTESIAN_POINT('Ctrl Pts',(7.24500126602242,-2.98638238306039,9.59229587079984));
#20527=CARTESIAN_POINT('Ctrl Pts',(3.45867836056103,-3.9621717494319,9.79081198821151));
#20528=CARTESIAN_POINT('Ctrl Pts',(0.586113239980029,-1.30947959617202,
9.98932810562315));
#20529=CARTESIAN_POINT('Ctrl Pts',(1.25794639972494,2.54240906231909,10.1878442230349));
#20530=CARTESIAN_POINT('Ctrl Pts',(4.85892581172318,4.06600786328675,10.3863603404465));
#20531=CARTESIAN_POINT('Ctrl Pts',(8.09134302835829,1.86603400672705,10.5848764578582));
#20532=CARTESIAN_POINT('Ctrl Pts',(7.99501184973105,-2.04281829746266,10.7833925752698));
#20533=CARTESIAN_POINT('Ctrl Pts',(4.658150536815,-4.08089646336047,10.9819086926815));
#20534=CARTESIAN_POINT('Ctrl Pts',(1.13659320614603,-2.38176727499459,11.1804248100931));
#20535=CARTESIAN_POINT('Ctrl Pts',(0.655315074027438,1.49853907779376,11.3789409275048));
#20536=CARTESIAN_POINT('Ctrl Pts',(3.6550614989726,4.00651184837438,11.5774570449165));
#20537=CARTESIAN_POINT('Ctrl Pts',(7.38872176624422,2.84539728015019,11.7759731623281));
#20538=CARTESIAN_POINT('Ctrl Pts',(8.43708082482397,-0.921477992040132,
11.9744892797398));
#20539=CARTESIAN_POINT('Ctrl Pts',(5.84007139076835,-3.84448124749012,12.1730053971514));
#20540=CARTESIAN_POINT('Ctrl Pts',(1.97598530342792,-3.24678170627628,12.3715215145631));
#20541=CARTESIAN_POINT('Ctrl Pts',(0.383479098877827,0.324258761208613,
12.5700376319747));
#20542=CARTESIAN_POINT('Ctrl Pts',(2.52093966656498,3.59834922323431,12.7685537493864));
#20543=CARTESIAN_POINT('Ctrl Pts',(6.43092127741269,3.5771399144821,12.967069866798));
#20544=CARTESIAN_POINT('Ctrl Pts',(8.53273714794332,0.280053916463419,13.1655859842097));
#20545=CARTESIAN_POINT('Ctrl Pts',(6.90158428470204,-3.27350013106212,13.3641021016213));
#20546=CARTESIAN_POINT('Ctrl Pts',(3.0312414520278,-3.82924502713605,13.562618219033));
#20547=CARTESIAN_POINT('Ctrl Pts',(0.466094994356506,-0.878240167322765,
13.7611343364446));
#20548=CARTESIAN_POINT('Ctrl Pts',(1.55525724336407,2.87704033182534,13.9596504538563));
#20549=CARTESIAN_POINT('Ctrl Pts',(5.30129412947213,3.99758202219787,14.1581665712679));
#20550=CARTESIAN_POINT('Ctrl Pts',(8.27365632956023,1.45721413871475,14.3566826886797));
#20551=CARTESIAN_POINT('Ctrl Pts',(7.75031108111198,-2.41764273385123,14.5551988060912));
#20552=CARTESIAN_POINT('Ctrl Pts',(4.21052800757405,-4.07846837919741,14.753714923503));
#20553=CARTESIAN_POINT('Ctrl Pts',(0.895973113878727,-2.00431026356939,
14.9522310409146));
#20554=CARTESIAN_POINT('Ctrl Pts',(0.842052722152676,1.9053570654116,15.1507471583263));
#20555=CARTESIAN_POINT('Ctrl Pts',(4.09814610146403,4.07013463762311,15.3492632757379));
#20556=CARTESIAN_POINT('Ctrl Pts',(7.682384872503,2.50756033086961,15.5477793931496));
#20557=CARTESIAN_POINT('Ctrl Pts',(8.31239134820293,-1.35139002803904,15.7462955105612));
#20558=CARTESIAN_POINT('Ctrl Pts',(5.41121758211169,-3.97276310543362,15.9448116279729));
#20559=CARTESIAN_POINT('Ctrl Pts',(1.63570332303896,-2.95595530083938,16.1433277453845));
#20560=CARTESIAN_POINT('Ctrl Pts',(0.443392711547191,0.767860140031627,
16.3418438627962));
#20561=CARTESIAN_POINT('Ctrl Pts',(2.92618112548781,3.7884838709103,16.5403599802078));
#20562=CARTESIAN_POINT('Ctrl Pts',(6.8103781630174,3.33968613741389,16.7388760976195));
#20563=CARTESIAN_POINT('Ctrl Pts',(8.5389100624284,-0.167532633159739,16.9373922150311));
#20564=CARTESIAN_POINT('Ctrl Pts',(6.52882019040339,-3.5213282050942,17.1359083324428));
#20565=CARTESIAN_POINT('Ctrl Pts',(2.62091061577914,-3.65035838956845,17.3344244498544));
#20566=CARTESIAN_POINT('Ctrl Pts',(0.393970590674286,-0.43645979805503,
17.5329405672661));
#20567=CARTESIAN_POINT('Ctrl Pts',(1.88738942918871,3.17714037417117,17.7314566846778));
#20568=CARTESIAN_POINT('Ctrl Pts',(5.73352256684974,3.8811758273502,17.9299728020894));
#20569=CARTESIAN_POINT('Ctrl Pts',(8.41015443739666,1.03090428563328,18.1284889195011));
#20570=CARTESIAN_POINT('Ctrl Pts',(7.46607648872073,-2.76344979098553,18.3270050369127));
#20571=CARTESIAN_POINT('Ctrl Pts',(3.76585734795025,-4.02708911541293,18.5255211543244));
#20572=CARTESIAN_POINT('Ctrl Pts',(0.698087318576006,-1.60279683129456,
18.724037271736));
#20573=CARTESIAN_POINT('Ctrl Pts',(1.07217183831651,2.28930630247911,18.9225533891477));
#20574=CARTESIAN_POINT('Ctrl Pts',(4.54553141985243,4.08490627169594,19.1210695065593));
#20575=CARTESIAN_POINT('Ctrl Pts',(7.93732942868568,2.13962678039228,19.319585623971));
#20576=CARTESIAN_POINT('Ctrl Pts',(8.14142176722837,-1.76508221626667,19.5181017413827));
#20577=CARTESIAN_POINT('Ctrl Pts',(4.97090455397163,-4.05336249490537,19.7166178587943));
#20578=CARTESIAN_POINT('Ctrl Pts',(1.3292771434127,-2.62965050343175,19.915133976206));
#20579=CARTESIAN_POINT('Ctrl Pts',(0.551472646603815,1.20224539704524,20.1136500936177));
#20580=CARTESIAN_POINT('Ctrl Pts',(3.3497896271543,3.93314783354192,20.3121662110293));
#20581=CARTESIAN_POINT('Ctrl Pts',(7.16158262229433,3.06214829760668,20.510682328441));
#20582=CARTESIAN_POINT('Ctrl Pts',(8.49608411816253,-0.613108395518473,
20.7091984458526));
#20583=CARTESIAN_POINT('Ctrl Pts',(6.13118302381429,-3.72689209317441,20.9077145632643));
#20584=CARTESIAN_POINT('Ctrl Pts',(2.23261078765349,-3.42765888460072,21.1062306806759));
#20585=CARTESIAN_POINT('Ctrl Pts',(0.370605683008962,0.0105590905653954,
21.3047467980876));
#20586=CARTESIAN_POINT('Ctrl Pts',(2.250356607504,3.43910732612115,21.5032629154992));
#20587=CARTESIAN_POINT('Ctrl Pts',(6.15042334082164,3.71818634797007,21.7017790329109));
#20588=CARTESIAN_POINT('Ctrl Pts',(8.49919910975228,0.592221314373082,21.9002951503225));
#20589=CARTESIAN_POINT('Ctrl Pts',(7.14571944818345,-3.07608926032515,22.0988112677342));
#20590=CARTESIAN_POINT('Ctrl Pts',(3.32947585071529,-3.92737479389549,22.2973273851459));
#20591=CARTESIAN_POINT('Ctrl Pts',(0.545310524977601,-1.18204713458114,
22.4958435025575));
#20592=CARTESIAN_POINT('Ctrl Pts',(1.34291119900688,2.64578051982372,22.6943596199692));
#20593=CARTESIAN_POINT('Ctrl Pts',(4.99184635260365,4.05064557959106,22.8928757373808));
#20594=CARTESIAN_POINT('Ctrl Pts',(8.15049824324278,1.74602012818506,23.0913918547925));
#20595=CARTESIAN_POINT('Ctrl Pts',(7.92621886181009,-2.15760353803636,23.2899079722041));
#20596=CARTESIAN_POINT('Ctrl Pts',(4.52442717371885,-4.08528469325705,23.4884240896158));
#20597=CARTESIAN_POINT('Ctrl Pts',(1.06036526828869,-2.27183616857484,23.6869402070274));
#20598=CARTESIAN_POINT('Ctrl Pts',(0.706458758169362,1.62230144113535,23.8854563244391));
#20599=CARTESIAN_POINT('Ctrl Pts',(3.78660979300229,4.03041197296648,24.0839724418507));
#20600=CARTESIAN_POINT('Ctrl Pts',(7.48045570332662,2.74822735016753,24.2824885592624));
#20601=CARTESIAN_POINT('Ctrl Pts',(8.40451183040988,-1.05203519730533,24.481004676674));
#20602=CARTESIAN_POINT('Ctrl Pts',(5.71394743641032,-3.88635869185298,24.6795207940858));
#20603=CARTESIAN_POINT('Ctrl Pts',(1.87003416737941,-3.16648164392546,24.8780369114974));
#20604=CARTESIAN_POINT('Ctrl Pts',(0.398188145107553,0.462946646320358,
25.076553028909));
#20605=CARTESIAN_POINT('Ctrl Pts',(1.88978798161488,2.58492499113116,25.2088971071835));
#20606=CARTESIAN_POINT('Ctrl Pts',(2.91960708544911,3.09611134481228,25.2750691463207));
#20607=CARTESIAN_POINT('Ctrl Pts',(2.58997049159961,-2.62015330925654,0.00319355095334283));
#20608=CARTESIAN_POINT('Ctrl Pts',(1.71783944528228,-1.99894889552244,0.0694097009926075));
#20609=CARTESIAN_POINT('Ctrl Pts',(0.65845605968771,0.171475772890977,0.20179789016909));
#20610=CARTESIAN_POINT('Ctrl Pts',(2.5459024084217,3.29075405988094,0.400358118482792));
#20611=CARTESIAN_POINT('Ctrl Pts',(6.18433372098768,3.38626231280436,0.598874235894448));
#20612=CARTESIAN_POINT('Ctrl Pts',(8.23950371306965,0.385416781850904,0.797390353306103));
#20613=CARTESIAN_POINT('Ctrl Pts',(6.83072086642306,-2.97082408396747,0.995906470717762));
#20614=CARTESIAN_POINT('Ctrl Pts',(3.24739392835603,-3.60517206763711,1.19442258812942));
#20615=CARTESIAN_POINT('Ctrl Pts',(0.771445147794971,-0.938633334672633,
1.39293870554108));
#20616=CARTESIAN_POINT('Ctrl Pts',(1.6701033647243,2.58783275185508,1.59145482295273));
#20617=CARTESIAN_POINT('Ctrl Pts',(5.12049770482736,3.74423103498232,1.78997094036439));
#20618=CARTESIAN_POINT('Ctrl Pts',(7.96276883664299,1.47182751406662,1.98848705777604));
#20619=CARTESIAN_POINT('Ctrl Pts',(7.59404699250464,-2.14849653622342,2.1870031751877));
#20620=CARTESIAN_POINT('Ctrl Pts',(4.35198598660702,-3.80124283382013,2.38551929259936));
#20621=CARTESIAN_POINT('Ctrl Pts',(1.20561125008781,-1.97289654529749,2.58403541001101));
#20622=CARTESIAN_POINT('Ctrl Pts',(1.0363089362513,1.66219780307218,2.78255152742267));
#20623=CARTESIAN_POINT('Ctrl Pts',(3.99912495903867,3.77507940693446,2.98106764483432));
#20624=CARTESIAN_POINT('Ctrl Pts',(7.38076768128599,2.43081698451723,3.17958376224598));
#20625=CARTESIAN_POINT('Ctrl Pts',(8.08439358796167,-1.13954237620741,3.37809987965763));
#20626=CARTESIAN_POINT('Ctrl Pts',(5.4656351638386,-3.66632999264102,3.5766159970693));
#20627=CARTESIAN_POINT('Ctrl Pts',(1.92270171311447,-2.83556261008053,3.77513211448094));
#20628=CARTESIAN_POINT('Ctrl Pts',(0.700144216203009,0.591959212043988,
3.97364823189261));
#20629=CARTESIAN_POINT('Ctrl Pts',(2.91755761499276,3.47737597536012,4.17216434930425));
#20630=CARTESIAN_POINT('Ctrl Pts',(6.54427687678886,3.1782780050441,4.37068046671592));
#20631=CARTESIAN_POINT('Ctrl Pts',(8.2590215005,-0.0314265247951463,4.56919658412757));
#20632=CARTESIAN_POINT('Ctrl Pts',(6.49146097171637,-3.21235123071783,4.76771270153922));
#20633=CARTESIAN_POINT('Ctrl Pts',(2.86029360321679,-3.45146579032245,4.96622881895089));
#20634=CARTESIAN_POINT('Ctrl Pts',(0.690873397337037,-0.529793630188544,
5.16474493636253));
#20635=CARTESIAN_POINT('Ctrl Pts',(1.96991411271267,2.8770534572674,5.36326105377419));
#20636=CARTESIAN_POINT('Ctrl Pts',(5.52609459169944,3.64914971667956,5.56177717118585));
#20637=CARTESIAN_POINT('Ctrl Pts',(8.1027323975949,1.07942407934716,5.7602932885975));
#20638=CARTESIAN_POINT('Ctrl Pts',(7.34019164048911,-2.47881759682101,5.95880940600916));
#20639=CARTESIAN_POINT('Ctrl Pts',(3.93679264073839,-3.76700527003896,6.15732552342081));
#20640=CARTESIAN_POINT('Ctrl Pts',(1.00930346276847,-1.60544117293717,6.35584164083248));
#20641=CARTESIAN_POINT('Ctrl Pts',(1.23866300903221,2.02635541158186,6.55435775824412));
#20642=CARTESIAN_POINT('Ctrl Pts',(4.41482816993367,3.80245425555658,6.75287387565579));
#20643=CARTESIAN_POINT('Ctrl Pts',(7.6291273081915,2.09633782263408,6.95138999306744));
#20644=CARTESIAN_POINT('Ctrl Pts',(7.93796641543966,-1.5295649116789,7.14990611047909));
#20645=CARTESIAN_POINT('Ctrl Pts',(5.05851651200422,-3.75472119528823,7.34842222789076));
#20646=CARTESIAN_POINT('Ctrl Pts',(1.62772304650576,-2.54137523062185,7.5469383453024));
#20647=CARTESIAN_POINT('Ctrl Pts',(0.787441414036509,0.999313828164636,
7.74545446271406));
#20648=CARTESIAN_POINT('Ctrl Pts',(3.30718554976015,3.62485029208286,7.94397058012572));
#20649=CARTESIAN_POINT('Ctrl Pts',(6.8794217047968,2.93081781047529,8.14248669753737));
#20650=CARTESIAN_POINT('Ctrl Pts',(8.23276395950072,-0.447201871899268,
8.34100281494903));
#20651=CARTESIAN_POINT('Ctrl Pts',(6.12784722031342,-3.41568258667014,8.53951893236069));
#20652=CARTESIAN_POINT('Ctrl Pts',(2.49231419722064,-3.25614616174064,8.73803504977233));
#20653=CARTESIAN_POINT('Ctrl Pts',(0.655516877599837,-0.114693020356707,
8.93655116718401));
#20654=CARTESIAN_POINT('Ctrl Pts',(2.29955930716991,3.13179380737736,9.13506728459565));
#20655=CARTESIAN_POINT('Ctrl Pts',(5.9188587019336,3.51024343935022,9.33358340200731));
#20656=CARTESIAN_POINT('Ctrl Pts',(8.19892952254092,0.674078901476532,9.53209951941897));
#20657=CARTESIAN_POINT('Ctrl Pts',(7.05172628302556,-2.77939427202906,9.73061563683061));
#20658=CARTESIAN_POINT('Ctrl Pts',(3.52783588801619,-3.68755104089551,9.92913175424228));
#20659=CARTESIAN_POINT('Ctrl Pts',(0.854370129759403,-1.21871871116838,
10.1276478716539));
#20660=CARTESIAN_POINT('Ctrl Pts',(1.47963809495571,2.36619303175871,10.3261639890656));
#20661=CARTESIAN_POINT('Ctrl Pts',(4.83103127493619,3.78419020596524,10.5246801064772));
#20662=CARTESIAN_POINT('Ctrl Pts',(7.83940754573271,1.73669797247918,10.7231962238889));
#20663=CARTESIAN_POINT('Ctrl Pts',(7.74975314393437,-1.90122922870495,10.9217123413006));
#20664=CARTESIAN_POINT('Ctrl Pts',(4.64417186530054,-3.79804686745578,11.1202284587122));
#20665=CARTESIAN_POINT('Ctrl Pts',(1.36669597038421,-2.21668543150265,11.3187445761239));
#20666=CARTESIAN_POINT('Ctrl Pts',(0.91877553954763,1.39467435679268,11.5172606935355));
#20667=CARTESIAN_POINT('Ctrl Pts',(3.71060758300086,3.72881789865659,11.7157768109472));
#20668=CARTESIAN_POINT('Ctrl Pts',(7.18548542162604,2.64818093856821,11.9142929283589));
#20669=CARTESIAN_POINT('Ctrl Pts',(8.16118202999545,-0.857609751318129,
12.1128090457705));
#20670=CARTESIAN_POINT('Ctrl Pts',(5.74417301388192,-3.57801774441457,12.3113251631822));
#20671=CARTESIAN_POINT('Ctrl Pts',(2.14790925385559,-3.02174514829049,12.5098412805938));
#20672=CARTESIAN_POINT('Ctrl Pts',(0.665780693158256,0.301784174950485,
12.7083573980055));
#20673=CARTESIAN_POINT('Ctrl Pts',(2.65509247460188,3.34894529131551,12.9068735154171));
#20674=CARTESIAN_POINT('Ctrl Pts',(6.29407070946287,3.32920601358802,13.1053896328288));
#20675=CARTESIAN_POINT('Ctrl Pts',(8.25020835096136,0.260643196829997,13.3039057502404));
#20676=CARTESIAN_POINT('Ctrl Pts',(6.7321117566965,-3.04661170162563,13.5024218676521));
#20677=CARTESIAN_POINT('Ctrl Pts',(3.1300249104368,-3.56383755643203,13.7009379850637));
#20678=CARTESIAN_POINT('Ctrl Pts',(0.742670427029733,-0.817368768436538,
13.8994541024754));
#20679=CARTESIAN_POINT('Ctrl Pts',(1.75634213008195,2.67763078969056,14.0979702198871));
#20680=CARTESIAN_POINT('Ctrl Pts',(5.24273875601857,3.7205070045574,14.2964863372987));
#20681=CARTESIAN_POINT('Ctrl Pts',(8.0090845931027,1.35621367619806,14.4950024547104));
#20682=CARTESIAN_POINT('Ctrl Pts',(7.52201274521021,-2.25007433890389,14.693518572122));
#20683=CARTESIAN_POINT('Ctrl Pts',(4.22757434555207,-3.79578707538995,14.8920346895337));
#20684=CARTESIAN_POINT('Ctrl Pts',(1.14275341367199,-1.86539021176013,15.0905508069453));
#20685=CARTESIAN_POINT('Ctrl Pts',(1.09257027946957,1.77329552431533,15.289066924357));
#20686=CARTESIAN_POINT('Ctrl Pts',(4.12298170266298,3.78803095088039,15.4875830417686));
#20687=CARTESIAN_POINT('Ctrl Pts',(7.45879454642923,2.3337596886183,15.6860991591803));
#20688=CARTESIAN_POINT('Ctrl Pts',(8.04513486233581,-1.25772430366396,15.8846152765919));
#20689=CARTESIAN_POINT('Ctrl Pts',(5.34504334245093,-3.69740830310385,16.0831313940036));
#20690=CARTESIAN_POINT('Ctrl Pts',(1.83121243949837,-2.75107611072479,16.2816475114153));
#20691=CARTESIAN_POINT('Ctrl Pts',(0.721541654250978,0.714639252839528,
16.4801636288269));
#20692=CARTESIAN_POINT('Ctrl Pts',(3.03224638366176,3.52590158253341,16.6786797462386));
#20693=CARTESIAN_POINT('Ctrl Pts',(6.64722719080097,3.10821031270302,16.8771958636502));
#20694=CARTESIAN_POINT('Ctrl Pts',(8.25595341671681,-0.155920837071448,
17.0757119810619));
#20695=CARTESIAN_POINT('Ctrl Pts',(6.38518418493321,-3.27726265018464,17.2742280984735));
#20696=CARTESIAN_POINT('Ctrl Pts',(2.74813437211341,-3.39734966840464,17.4727442158852));
#20697=CARTESIAN_POINT('Ctrl Pts',(0.675545012814546,-0.406208484742623,
17.6712603332969));
#20698=CARTESIAN_POINT('Ctrl Pts',(2.06545401745235,2.9569307023417,17.8697764507085));
#20699=CARTESIAN_POINT('Ctrl Pts',(5.64500915845253,3.61216899900811,18.0682925681202));
#20700=CARTESIAN_POINT('Ctrl Pts',(8.13612192804524,0.959451637121888,18.2668086855318));
#20701=CARTESIAN_POINT('Ctrl Pts',(7.25747863782803,-2.57191328333314,18.4653248029435));
#20702=CARTESIAN_POINT('Ctrl Pts',(3.81372409941205,-3.74796894189382,18.6638409203551));
#20703=CARTESIAN_POINT('Ctrl Pts',(0.958583211925542,-1.49170593738941,
18.8623570377668));
#20704=CARTESIAN_POINT('Ctrl Pts',(1.306739689582,2.13063298930591,19.0608731551785));
#20705=CARTESIAN_POINT('Ctrl Pts',(4.53935845279781,3.80177875335989,19.2593892725901));
#20706=CARTESIAN_POINT('Ctrl Pts',(7.69606872911877,1.99132785253305,19.4579053900018));
#20707=CARTESIAN_POINT('Ctrl Pts',(7.88601529454458,-1.64274321646801,19.6564215074134));
#20708=CARTESIAN_POINT('Ctrl Pts',(4.93524869751396,-3.77242129631514,19.8549376248251));
#20709=CARTESIAN_POINT('Ctrl Pts',(1.54602485826833,-2.44738771167893,20.0534537422367));
#20710=CARTESIAN_POINT('Ctrl Pts',(0.822130498506685,1.11891698433359,20.2519698596484));
#20711=CARTESIAN_POINT('Ctrl Pts',(3.42649430375165,3.66053879154859,20.45048597706));
#20712=CARTESIAN_POINT('Ctrl Pts',(6.97408943990954,2.84990880161489,20.6490020944717));
#20713=CARTESIAN_POINT('Ctrl Pts',(8.21609576658401,-0.570613452685432,
20.8475182118833));
#20714=CARTESIAN_POINT('Ctrl Pts',(6.015107509745,-3.46857877108964,21.046034329295));
#20715=CARTESIAN_POINT('Ctrl Pts',(2.38674785836889,-3.19008561139642,21.2445504467067));
#20716=CARTESIAN_POINT('Ctrl Pts',(0.653799542140776,0.00982723311048271,
21.4430665641183));
#20717=CARTESIAN_POINT('Ctrl Pts',(2.40326370386975,3.2007405539671,21.64158268153));
#20718=CARTESIAN_POINT('Ctrl Pts',(6.03301426782987,3.46047642676426,21.8400987989417));
#20719=CARTESIAN_POINT('Ctrl Pts',(8.21899485607472,0.551174068759129,22.0386149163533));
#20720=CARTESIAN_POINT('Ctrl Pts',(6.95932575274402,-2.86288350711349,22.2371310337649));
#20721=CARTESIAN_POINT('Ctrl Pts',(3.40758848840856,-3.65516588504588,22.4356471511766));
#20722=CARTESIAN_POINT('Ctrl Pts',(0.816395477550012,-1.10011867661645,
22.6341632685882));
#20723=CARTESIAN_POINT('Ctrl Pts',(1.55871392857562,2.46239974611297,22.8326793859999));
#20724=CARTESIAN_POINT('Ctrl Pts',(4.95473900642221,3.76989269217354,23.0311955034116));
#20725=CARTESIAN_POINT('Ctrl Pts',(7.89446267408575,1.62500233414576,23.2297116208232));
#20726=CARTESIAN_POINT('Ctrl Pts',(7.68572824288089,-2.00805862937836,23.4282277382349));
#20727=CARTESIAN_POINT('Ctrl Pts',(4.5197169557303,-3.80213094627573,23.6267438556465));
#20728=CARTESIAN_POINT('Ctrl Pts',(1.29575144062437,-2.11437372177854,23.8252599730582));
#20729=CARTESIAN_POINT('Ctrl Pts',(0.966374421579891,1.50985866999905,24.0237760904698));
#20730=CARTESIAN_POINT('Ctrl Pts',(3.83303817896047,3.7510614900228,24.2222922078815));
#20731=CARTESIAN_POINT('Ctrl Pts',(7.27086121968984,2.55774591981802,24.4208083252931));
#20732=CARTESIAN_POINT('Ctrl Pts',(8.13087041382945,-0.979117951521988,
24.6193244427048));
#20733=CARTESIAN_POINT('Ctrl Pts',(5.62679079307294,-3.61699263579137,24.8178405601165));
#20734=CARTESIAN_POINT('Ctrl Pts',(2.04930166016011,-2.94701073564213,25.0163566775281));
#20735=CARTESIAN_POINT('Ctrl Pts',(0.679470245798868,0.430859512276974,
25.2148727949398));
#20736=CARTESIAN_POINT('Ctrl Pts',(2.06768632464525,2.40576215381105,25.3472168732142));
#20737=CARTESIAN_POINT('Ctrl Pts',(3.02612799462649,2.8815178478641,25.4133889123514));
#20738=CARTESIAN_POINT('Ctrl Pts',(6.37917532696298,2.58637165759475,1.87594439571473));
#20739=CARTESIAN_POINT('Ctrl Pts',(6.35746818924401,2.60250872304869,1.87431323785475));
#20740=CARTESIAN_POINT('Ctrl Pts',(6.33555795831466,2.6183724646154,1.87269246732624));
#20741=CARTESIAN_POINT('Ctrl Pts',(6.19727492500446,2.71586407695624,1.86261629455797));
#20742=CARTESIAN_POINT('Ctrl Pts',(6.07580181006572,2.78999834520196,1.85444429514));
#20743=CARTESIAN_POINT('Ctrl Pts',(5.74237257220235,2.96434989857594,1.83317918573207));
#20744=CARTESIAN_POINT('Ctrl Pts',(5.523745245102,3.0498889011599,1.82041424434255));
#20745=CARTESIAN_POINT('Ctrl Pts',(5.23269930128191,3.12859918522094,1.80289072059331));
#20746=CARTESIAN_POINT('Ctrl Pts',(5.167062952266,3.14415666864464,1.79890198363588));
#20747=CARTESIAN_POINT('Ctrl Pts',(5.08538680607657,3.16082801904366,1.79383948934339));
#20748=CARTESIAN_POINT('Ctrl Pts',(5.06975831167358,3.16389752770189,1.79286635151808));
#20749=CARTESIAN_POINT('Ctrl Pts',(5.04516765851111,3.16853820472167,1.79132728319329));
#20750=CARTESIAN_POINT('Ctrl Pts',(5.0362202642569,3.17018752288347,1.79076565250961));
#20751=CARTESIAN_POINT('Ctrl Pts',(5.01960989374187,3.17317672567073,1.78971978245498));
#20752=CARTESIAN_POINT('Ctrl Pts',(5.01194893954713,3.17452677246842,1.78923612092467));
#20753=CARTESIAN_POINT('Ctrl Pts',(4.99426044855479,3.17757792655571,1.78811645356316));
#20754=CARTESIAN_POINT('Ctrl Pts',(4.9842297177955,3.17925930642477,1.78747936020121));
#20755=CARTESIAN_POINT('Ctrl Pts',(4.9528608055175,3.18436491139823,1.78548061603729));
#20756=CARTESIAN_POINT('Ctrl Pts',(4.93149653332297,3.18762191813225,1.7841101395166));
#20757=CARTESIAN_POINT('Ctrl Pts',(4.72526985244489,3.21694220194011,1.77080296572706));
#20758=CARTESIAN_POINT('Ctrl Pts',(4.53852237901646,3.22710773378337,1.75816929017416));
#20759=CARTESIAN_POINT('Ctrl Pts',(4.10975007637841,3.21319690026204,1.7291489467187));
#20760=CARTESIAN_POINT('Ctrl Pts',(3.86914891378651,3.17804088866835,1.71290336056405));
#20761=CARTESIAN_POINT('Ctrl Pts',(3.5992748360651,3.10687629774973,1.69520021938423));
#20762=CARTESIAN_POINT('Ctrl Pts',(3.56397672532074,3.09692103132523,1.69289331884349));
#20763=CARTESIAN_POINT('Ctrl Pts',(3.51146701374181,3.08113911750864,1.6894733305407));
#20764=CARTESIAN_POINT('Ctrl Pts',(3.49412320794559,3.07576618258719,1.68834564908029));
#20765=CARTESIAN_POINT('Ctrl Pts',(3.46423894478094,3.06623081615572,1.68640569433679));
#20766=CARTESIAN_POINT('Ctrl Pts',(3.45167711255051,3.06213735305142,1.68559118674377));
#20767=CARTESIAN_POINT('Ctrl Pts',(3.42566014199035,3.05348199253439,1.68390608985396));
#20768=CARTESIAN_POINT('Ctrl Pts',(3.4122092627877,3.04890813063507,1.68303591541222));
#20769=CARTESIAN_POINT('Ctrl Pts',(3.38062402109995,3.03793428309482,1.68099477896871));
#20770=CARTESIAN_POINT('Ctrl Pts',(3.36251570080964,3.03146059304165,1.67982628100462));
#20771=CARTESIAN_POINT('Ctrl Pts',(3.30280125605346,3.00950803713889,1.67597781096476));
#20772=CARTESIAN_POINT('Ctrl Pts',(3.2614559128536,2.99333123621255,1.67332102454893));
#20773=CARTESIAN_POINT('Ctrl Pts',(3.16372568218563,2.95274540414727,1.66704977644844));
#20774=CARTESIAN_POINT('Ctrl Pts',(3.1076779331469,2.9275679335125,1.66346049577536));
#20775=CARTESIAN_POINT('Ctrl Pts',(2.88871690118901,2.8215833150003,1.6494082159528));
#20776=CARTESIAN_POINT('Ctrl Pts',(2.73204847362243,2.72865485571952,1.63930708277088));
#20777=CARTESIAN_POINT('Ctrl Pts',(2.55338966493566,2.60111995887127,1.62701924739219));
#20778=CARTESIAN_POINT('Ctrl Pts',(2.52311833550173,2.57869950653125,1.62490735852054));
#20779=CARTESIAN_POINT('Ctrl Pts',(2.37642094346987,2.46601278327509,1.61449188041826));
#20780=CARTESIAN_POINT('Ctrl Pts',(2.2658994828539,2.36837774636692,1.606077629023));
#20781=CARTESIAN_POINT('Ctrl Pts',(2.14940807192336,2.25031822012699,1.59603999818292));
#20782=CARTESIAN_POINT('Ctrl Pts',(2.13647444372387,2.23698176940727,1.59490784905773));
#20783=CARTESIAN_POINT('Ctrl Pts',(2.11697321907695,2.21652214215941,1.59317222555267));
#20784=CARTESIAN_POINT('Ctrl Pts',(2.11032100024688,2.20947968349679,1.59257501882737));
#20785=CARTESIAN_POINT('Ctrl Pts',(2.09836047923665,2.19670260377342,1.59149166433327));
#20786=CARTESIAN_POINT('Ctrl Pts',(2.0930411741091,2.19097855606262,1.59100636978853));
#20787=CARTESIAN_POINT('Ctrl Pts',(2.0813054934234,2.17825744587329,1.58992790874209));
#20788=CARTESIAN_POINT('Ctrl Pts',(2.07489927521574,2.17125144160783,1.58933402028445));
#20789=CARTESIAN_POINT('Ctrl Pts',(2.05626385387461,2.15068956984932,1.58759147284775));
#20790=CARTESIAN_POINT('Ctrl Pts',(2.04411900823446,2.13705822286543,1.58643683323208));
#20791=CARTESIAN_POINT('Ctrl Pts',(1.93717851777626,2.01495528921416,1.57610498041153));
#20792=CARTESIAN_POINT('Ctrl Pts',(1.84964933744078,1.9003555296462,1.56649003599813));
#20793=CARTESIAN_POINT('Ctrl Pts',(1.64333323951227,1.58903548256601,1.54129901712155));
#20794=CARTESIAN_POINT('Ctrl Pts',(1.53735010744345,1.3847512085533,1.52568539709475));
#20795=CARTESIAN_POINT('Ctrl Pts',(1.42252413795245,1.09031305146266,1.50512106213752));
#20796=CARTESIAN_POINT('Ctrl Pts',(1.3943430716333,1.00845973638979,1.49958705881355));
#20797=CARTESIAN_POINT('Ctrl Pts',(1.36216740356011,0.901146159759775,1.49256202096957));
#20798=CARTESIAN_POINT('Ctrl Pts',(1.35513586551897,0.876641100171909,1.49097297731463));
#20799=CARTESIAN_POINT('Ctrl Pts',(1.34430274319641,0.837124689555323,1.48843416917684));
#20800=CARTESIAN_POINT('Ctrl Pts',(1.34031739319521,0.822165270353613,1.48747847875109));
#20801=CARTESIAN_POINT('Ctrl Pts',(1.33292886436729,0.793605969097431,1.48566403734921));
#20802=CARTESIAN_POINT('Ctrl Pts',(1.32950634031576,0.780011504483906,1.48480467920146));
#20803=CARTESIAN_POINT('Ctrl Pts',(1.32187804752054,0.748854177816674,1.48284479383397));
#20804=CARTESIAN_POINT('Ctrl Pts',(1.31773095647574,0.731277329663039,1.4817461756327));
#20805=CARTESIAN_POINT('Ctrl Pts',(1.30532273452457,0.676635847758998,1.47835191741383));
#20806=CARTESIAN_POINT('Ctrl Pts',(1.29756859784815,0.639458589344792,1.47607247493859));
#20807=CARTESIAN_POINT('Ctrl Pts',(1.26262802264064,0.455747884216578,1.46494311038925));
#20808=CARTESIAN_POINT('Ctrl Pts',(1.24496967374256,0.307580423469625,1.45639721513811));
#20809=CARTESIAN_POINT('Ctrl Pts',(1.228689965464,-0.0225959984325165,1.43775141445356));
#20810=CARTESIAN_POINT('Ctrl Pts',(1.23508488552788,-0.204323671620051,
1.42775637084742));
#20811=CARTESIAN_POINT('Ctrl Pts',(1.26964919262474,-0.491930673826586,
1.41125360369806));
#20812=CARTESIAN_POINT('Ctrl Pts',(1.28795231687946,-0.598592794204186,
1.40497435296812));
#20813=CARTESIAN_POINT('Ctrl Pts',(1.31516393348759,-0.720130921935759,
1.39743113501213));
#20814=CARTESIAN_POINT('Ctrl Pts',(1.31887059945707,-0.736112978916704,
1.39643135237084));
#20815=CARTESIAN_POINT('Ctrl Pts',(1.32505288367227,-0.761873837776047,
1.39480609843874));
#20816=CARTESIAN_POINT('Ctrl Pts',(1.32745272187494,-0.771670761154133,
1.39418478697599));
#20817=CARTESIAN_POINT('Ctrl Pts',(1.33179830248319,-0.789057233235905,
1.39307615832644));
#20818=CARTESIAN_POINT('Ctrl Pts',(1.33372577905735,-0.796651153117467,
1.39258989111248));
#20819=CARTESIAN_POINT('Ctrl Pts',(1.3379691473637,-0.813117238728657,1.39153099155264));
#20820=CARTESIAN_POINT('Ctrl Pts',(1.34029518146952,-0.821986437301457,
1.39095780468898));
#20821=CARTESIAN_POINT('Ctrl Pts',(1.34696417809225,-0.846980241954366,
1.38933479019491));
#20822=CARTESIAN_POINT('Ctrl Pts',(1.35139459402551,-0.863080919834322,
1.38828014641097));
#20823=CARTESIAN_POINT('Ctrl Pts',(1.3806601377049,-0.966292876861225,1.38146396062797));
#20824=CARTESIAN_POINT('Ctrl Pts',(1.40903139841715,-1.05235117592572,1.37552680524109));
#20825=CARTESIAN_POINT('Ctrl Pts',(1.55285099075795,-1.43375016951215,1.34839112790262));
#20826=CARTESIAN_POINT('Ctrl Pts',(1.70791862549142,-1.71236053840431,1.32651796330595));
#20827=CARTESIAN_POINT('Ctrl Pts',(1.93875599357569,-2.0127194568175,1.30217189147774));
#20828=CARTESIAN_POINT('Ctrl Pts',(1.97772359589434,-2.06051946385817,1.29826144142414));
#20829=CARTESIAN_POINT('Ctrl Pts',(2.03276832942079,-2.12421737454299,1.2929971592978));
#20830=CARTESIAN_POINT('Ctrl Pts',(2.04767430295176,-2.14110544973065,1.2915960762896));
#20831=CARTESIAN_POINT('Ctrl Pts',(2.07170644705166,-2.16776458536358,1.28937529364269));
#20832=CARTESIAN_POINT('Ctrl Pts',(2.0807182656183,-2.17763729534634,1.28855084484696));
#20833=CARTESIAN_POINT('Ctrl Pts',(2.09937550282305,-2.19782317023249,1.28686083992946));
#20834=CARTESIAN_POINT('Ctrl Pts',(2.10902781081721,-2.20812959706504,1.28599560298287));
#20835=CARTESIAN_POINT('Ctrl Pts',(2.13160406142546,-2.23192045627524,1.28399259870112));
#20836=CARTESIAN_POINT('Ctrl Pts',(2.1445781918029,-2.24535672493916,1.28285702623467));
#20837=CARTESIAN_POINT('Ctrl Pts',(2.1865695153516,-2.2880939385146,1.27923022181115));
#20838=CARTESIAN_POINT('Ctrl Pts',(2.21603323590006,-2.31695174039986,1.2767585685141));
#20839=CARTESIAN_POINT('Ctrl Pts',(2.2866523443305,-2.38351143551458,1.27099548261519));
#20840=CARTESIAN_POINT('Ctrl Pts',(2.32824969105022,-2.42072595863082,1.26772391419552));
#20841=CARTESIAN_POINT('Ctrl Pts',(2.48777406272148,-2.55615014524893,1.25558771499452));
#20842=CARTESIAN_POINT('Ctrl Pts',(2.61170280612446,-2.64698047305603,1.24697883892509));
#20843=CARTESIAN_POINT('Ctrl Pts',(2.92130934367302,-2.84155495632107,1.22652503606375));
#20844=CARTESIAN_POINT('Ctrl Pts',(3.11167151330051,-2.93643403866995,1.2147599773957));
#20845=CARTESIAN_POINT('Ctrl Pts',(3.33383261748784,-3.0210028651444,1.20048981068735));
#20846=CARTESIAN_POINT('Ctrl Pts',(3.35782913388204,-3.02981205948318,1.19894138686802));
#20847=CARTESIAN_POINT('Ctrl Pts',(3.39146274851147,-3.04170697527912,1.19675797779796));
#20848=CARTESIAN_POINT('Ctrl Pts',(3.40101413325445,-3.04503442659141,1.1961364589124));
#20849=CARTESIAN_POINT('Ctrl Pts',(3.41753881168727,-3.05070410195038,1.19505839356474));
#20850=CARTESIAN_POINT('Ctrl Pts',(3.42450481962554,-3.05306753662489,1.19460308113107));
#20851=CARTESIAN_POINT('Ctrl Pts',(3.43923812089619,-3.05801008306017,1.19363816397147));
#20852=CARTESIAN_POINT('Ctrl Pts',(3.44700724208598,-3.06058348793223,1.1931282219223));
#20853=CARTESIAN_POINT('Ctrl Pts',(3.46626875112046,-3.0668822562555,1.19186132029033));
#20854=CARTESIAN_POINT('Ctrl Pts',(3.47777234525126,-3.07057261047674,1.19110237139053));
#20855=CARTESIAN_POINT('Ctrl Pts',(3.52089764103687,-3.08414025181291,1.1882492520801));
#20856=CARTESIAN_POINT('Ctrl Pts',(3.55264909981536,-3.09359406787166,1.18613271570161));
#20857=CARTESIAN_POINT('Ctrl Pts',(3.79219819575261,-3.1609159816438,1.17007447922355));
#20858=CARTESIAN_POINT('Ctrl Pts',(4.00517766215825,-3.19827627834922,1.15533189525162));
#20859=CARTESIAN_POINT('Ctrl Pts',(4.43164769923035,-3.22961612740667,1.12650926895391));
#20860=CARTESIAN_POINT('Ctrl Pts',(4.64406716370717,-3.22426313447634,1.1124984498106));
#20861=CARTESIAN_POINT('Ctrl Pts',(4.88162605466237,-3.1947001219446,1.09742658096952));
#20862=CARTESIAN_POINT('Ctrl Pts',(4.90875424646882,-3.19097250473502,1.0957134719679));
#20863=CARTESIAN_POINT('Ctrl Pts',(4.95316394790896,-3.18429253967359,1.09292162964129));
#20864=CARTESIAN_POINT('Ctrl Pts',(4.97047428364735,-3.18154419125974,1.09183654739639));
#20865=CARTESIAN_POINT('Ctrl Pts',(5.00157511752,-3.17634587892235,1.08989243172842));
#20866=CARTESIAN_POINT('Ctrl Pts',(5.01537359201356,-3.1739469894221,1.08903181033593));
#20867=CARTESIAN_POINT('Ctrl Pts',(5.04479344599701,-3.16863449006096,1.08720079935052));
#20868=CARTESIAN_POINT('Ctrl Pts',(5.06040984258929,-3.16569513084344,1.0862312494149));
#20869=CARTESIAN_POINT('Ctrl Pts',(5.10270101251687,-3.15741064192127,1.08361164102233));
#20870=CARTESIAN_POINT('Ctrl Pts',(5.12933124873605,-3.1518429917002,1.08196866779826));
#20871=CARTESIAN_POINT('Ctrl Pts',(5.27356128668659,-3.11977711706809,1.07310139700947));
#20872=CARTESIAN_POINT('Ctrl Pts',(5.38968115929224,-3.0870323695469,1.06608013217971));
#20873=CARTESIAN_POINT('Ctrl Pts',(5.65510267094297,-2.99583426138442,1.05004550725694));
#20874=CARTESIAN_POINT('Ctrl Pts',(5.80241925226489,-2.93260388026925,1.041161498306));
#20875=CARTESIAN_POINT('Ctrl Pts',(6.08861324843494,-2.78363882719303,1.02308286470513));
#20876=CARTESIAN_POINT('Ctrl Pts',(6.22689818369351,-2.6977968469199,1.01390732908834));
#20877=CARTESIAN_POINT('Ctrl Pts',(6.36514710073905,-2.59675606037843,1.00364239908801));
#20878=CARTESIAN_POINT('Ctrl Pts',(6.37217184219401,-2.59157804146046,1.00311764554919));
#20879=CARTESIAN_POINT('Ctrl Pts',(6.37917532113595,-2.58637166192656,1.00259120688551));
#20880=CARTESIAN_POINT('Origin',(4.45646910621825,-5.13094777615093E-16,
-2.31077344927308));
#20881=CARTESIAN_POINT('Ctrl Pts',(7.67921910621823,3.83865910396161E-12,
6.06327685380577));
#20882=CARTESIAN_POINT('Ctrl Pts',(7.67921910621823,-0.00048391001007088,
6.0633051914467));
#20883=CARTESIAN_POINT('Ctrl Pts',(7.67921899722642,-0.000967821022726189,
6.06333352625195));
#20884=CARTESIAN_POINT('Ctrl Pts',(7.67917212283792,-0.105025812727111,
6.06942589124854));
#20885=CARTESIAN_POINT('Ctrl Pts',(7.67413246795198,-0.208542640984706,
6.07535155547207));
#20886=CARTESIAN_POINT('Ctrl Pts',(7.6420606122514,-0.53864869853577,6.0940950333389));
#20887=CARTESIAN_POINT('Ctrl Pts',(7.59597263080692,-0.762652150599657,
6.10654628211578));
#20888=CARTESIAN_POINT('Ctrl Pts',(7.50452302104189,-1.04917758523805,6.12397306485735));
#20889=CARTESIAN_POINT('Ctrl Pts',(7.48007404257778,-1.11768409440402,6.12826318255371));
#20890=CARTESIAN_POINT('Ctrl Pts',(7.44734176898383,-1.20044303755238,6.13366533835845));
#20891=CARTESIAN_POINT('Ctrl Pts',(7.44123764555465,-1.21554083125573,6.13465998003665));
#20892=CARTESIAN_POINT('Ctrl Pts',(7.43151441581216,-1.23907515062649,6.13622569490362));
#20893=CARTESIAN_POINT('Ctrl Pts',(7.42797314456913,-1.24754381414792,6.13679222042822));
#20894=CARTESIAN_POINT('Ctrl Pts',(7.42134030134804,-1.26321725180863,6.13784671089852));
#20895=CARTESIAN_POINT('Ctrl Pts',(7.418258575943,-1.27042597643201,6.13833408409028));
#20896=CARTESIAN_POINT('Ctrl Pts',(7.41115147309215,-1.28688438983048,6.13945223440697));
#20897=CARTESIAN_POINT('Ctrl Pts',(7.40710896466478,-1.2961264371954,6.14008402990406));
#20898=CARTESIAN_POINT('Ctrl Pts',(7.39443896504767,-1.32472632376073,6.14205094914058));
#20899=CARTESIAN_POINT('Ctrl Pts',(7.38566406168201,-1.34401770140436,6.14339452255131));
#20900=CARTESIAN_POINT('Ctrl Pts',(7.36467059356333,-1.38898898006688,6.14656381318704));
#20901=CARTESIAN_POINT('Ctrl Pts',(7.35230125483227,-1.41459617142862,6.14839718205939));
#20902=CARTESIAN_POINT('Ctrl Pts',(7.30719450615279,-1.50490537025683,6.15495711142845));
#20903=CARTESIAN_POINT('Ctrl Pts',(7.27261568508749,-1.56865949614297,6.15976135032848));
#20904=CARTESIAN_POINT('Ctrl Pts',(7.12164691893672,-1.82590134792096,6.17972206872809));
#20905=CARTESIAN_POINT('Ctrl Pts',(6.98721705230608,-2.00808803086824,6.19518778811049));
#20906=CARTESIAN_POINT('Ctrl Pts',(6.75183087139285,-2.26551680985559,6.21822014147556));
#20907=CARTESIAN_POINT('Ctrl Pts',(6.66367696821127,-2.35148714728407,6.22617234436212));
#20908=CARTESIAN_POINT('Ctrl Pts',(6.54964168690211,-2.4506189052801,6.23567053376896));
#20909=CARTESIAN_POINT('Ctrl Pts',(6.52823096756206,-2.46874610708932,6.23742248033569));
#20910=CARTESIAN_POINT('Ctrl Pts',(6.4940749899517,-2.49690663367201,6.24016903431721));
#20911=CARTESIAN_POINT('Ctrl Pts',(6.48148639754896,-2.507126933339,6.24117120223013));
#20912=CARTESIAN_POINT('Ctrl Pts',(6.45793522237783,-2.52595431079032,6.24302762824544));
#20913=CARTESIAN_POINT('Ctrl Pts',(6.44699295654035,-2.53458608164944,6.24388286388316));
#20914=CARTESIAN_POINT('Ctrl Pts',(6.42258759473381,-2.55358264332563,6.24577445636262));
#20915=CARTESIAN_POINT('Ctrl Pts',(6.40909777412277,-2.56391254329682,6.24680941752754));
#20916=CARTESIAN_POINT('Ctrl Pts',(6.36956542925041,-2.59369166525061,6.24981224504217));
#20917=CARTESIAN_POINT('Ctrl Pts',(6.34330912780274,-2.61285453949499,6.25176895903279));
#20918=CARTESIAN_POINT('Ctrl Pts',(6.14135721329509,-2.75561489916029,6.26654725313689));
#20919=CARTESIAN_POINT('Ctrl Pts',(5.95398379213897,-2.86176990562278,6.27866555039204));
#20920=CARTESIAN_POINT('Ctrl Pts',(5.55480133951951,-3.03789896576558,6.30307629519336));
#20921=CARTESIAN_POINT('Ctrl Pts',(5.34353643083463,-3.10616287874828,6.31531225761337));
#20922=CARTESIAN_POINT('Ctrl Pts',(5.10247529037649,-3.15743902642924,6.33011485045602));
#20923=CARTESIAN_POINT('Ctrl Pts',(5.07791181453018,-3.16236526487034,6.33163298382564));
#20924=CARTESIAN_POINT('Ctrl Pts',(5.04344952868219,-3.16885971715975,6.33377973801735));
#20925=CARTESIAN_POINT('Ctrl Pts',(5.03359634140045,-3.17066902587303,6.33439543971008));
#20926=CARTESIAN_POINT('Ctrl Pts',(5.01652521384103,-3.17372153193903,6.33546574139845));
#20927=CARTESIAN_POINT('Ctrl Pts',(5.00931110832481,-3.17498612975827,6.33591914227367));
#20928=CARTESIAN_POINT('Ctrl Pts',(4.99403824453613,-3.17760975813833,6.33688147732505));
#20929=CARTESIAN_POINT('Ctrl Pts',(4.98597854839038,-3.17896273960086,6.33739075875426));
#20930=CARTESIAN_POINT('Ctrl Pts',(4.96593639299222,-3.18224888470069,6.33866063549258));
#20931=CARTESIAN_POINT('Ctrl Pts',(4.95394808649034,-3.18414502396257,6.33942326867859));
#20932=CARTESIAN_POINT('Ctrl Pts',(4.90858324209756,-3.19105774535772,6.34231993218461));
#20933=CARTESIAN_POINT('Ctrl Pts',(4.87514060294697,-3.1956174197338,6.3444773701454));
#20934=CARTESIAN_POINT('Ctrl Pts',(4.61679406892825,-3.22671645238553,6.36128190363622));
#20935=CARTESIAN_POINT('Ctrl Pts',(4.38974140785457,-3.23000631896306,6.37680654875705));
#20936=CARTESIAN_POINT('Ctrl Pts',(3.96306792445177,-3.19115583727224,6.40566043609402));
#20937=CARTESIAN_POINT('Ctrl Pts',(3.76404202147251,-3.15396430240958,6.41898504479793));
#20938=CARTESIAN_POINT('Ctrl Pts',(3.54333496219127,-3.09080251638247,6.43344076151387));
#20939=CARTESIAN_POINT('Ctrl Pts',(3.51698756567261,-3.08289614982321,6.43516189075864));
#20940=CARTESIAN_POINT('Ctrl Pts',(3.47400786217016,-3.06939655237306,6.43796267066151));
#20941=CARTESIAN_POINT('Ctrl Pts',(3.45731471581481,-3.06400323358153,6.43904877947599));
#20942=CARTESIAN_POINT('Ctrl Pts',(3.42740300860117,-3.05406873616739,6.44099211392599));
#20943=CARTESIAN_POINT('Ctrl Pts',(3.41416847913398,-3.04957739548305,6.44185095169711));
#20944=CARTESIAN_POINT('Ctrl Pts',(3.38602443490044,-3.03982166532786,6.44367537458319));
#20945=CARTESIAN_POINT('Ctrl Pts',(3.37112356007344,-3.03453334315993,6.444640142819));
#20946=CARTESIAN_POINT('Ctrl Pts',(3.33092762369611,-3.01993384604648,6.44723985898657));
#20947=CARTESIAN_POINT('Ctrl Pts',(3.30570912542883,-3.0104145224515,6.44886786799746));
#20948=CARTESIAN_POINT('Ctrl Pts',(3.17146179822789,-2.95780614947448,6.45752254277157));
#20949=CARTESIAN_POINT('Ctrl Pts',(3.06471944041703,-2.9091060889055,6.46435756795522));
#20950=CARTESIAN_POINT('Ctrl Pts',(2.72914040728542,-2.73329193187802,6.48602695836141));
#20951=CARTESIAN_POINT('Ctrl Pts',(2.51308613861894,-2.58414291635044,6.50019868504366));
#20952=CARTESIAN_POINT('Ctrl Pts',(2.25718995935007,-2.35706983832039,6.51993688335784));
#20953=CARTESIAN_POINT('Ctrl Pts',(2.19896642337351,-2.30136619188119,6.52467172541004));
#20954=CARTESIAN_POINT('Ctrl Pts',(2.13225542105464,-2.23257293778352,6.53048479666582));
#20955=CARTESIAN_POINT('Ctrl Pts',(2.12169345093999,-2.22152510575018,6.53141735004696));
#20956=CARTESIAN_POINT('Ctrl Pts',(2.10452060179721,-2.20330454949227,6.53295457936054));
#20957=CARTESIAN_POINT('Ctrl Pts',(2.09786286312856,-2.19617606068154,6.53355580269414));
#20958=CARTESIAN_POINT('Ctrl Pts',(2.08592575774298,-2.18327802957213,6.53464353069165));
#20959=CARTESIAN_POINT('Ctrl Pts',(2.08063491888513,-2.17751937604288,6.5351291513768));
#20960=CARTESIAN_POINT('Ctrl Pts',(2.06900036266882,-2.16476321240039,6.53620484790273));
#20961=CARTESIAN_POINT('Ctrl Pts',(2.06266650265164,-2.15775713577978,6.53679561897515));
#20962=CARTESIAN_POINT('Ctrl Pts',(2.0443570680093,-2.13732467387981,6.53851817240934));
#20963=CARTESIAN_POINT('Ctrl Pts',(2.03246323693386,-2.12382597158592,6.53965572054656));
#20964=CARTESIAN_POINT('Ctrl Pts',(1.93565313950459,-2.0120804306145,6.54906375533661));
#20965=CARTESIAN_POINT('Ctrl Pts',(1.85664191543028,-1.90889283098158,6.55769123920622));
#20966=CARTESIAN_POINT('Ctrl Pts',(1.736910980754,-1.7312547884216,6.57210469166792));
#20967=CARTESIAN_POINT('Ctrl Pts',(1.69251077168293,-1.65944979631447,6.57782411451159));
#20968=CARTESIAN_POINT('Ctrl Pts',(1.54304557124267,-1.39505717242105,6.59835573859026));
#20969=CARTESIAN_POINT('Ctrl Pts',(1.45486622860033,-1.19357949543755,6.61298151427723));
#20970=CARTESIAN_POINT('Ctrl Pts',(1.37527813759098,-0.945551733204921,
6.62951403655511));
#20971=CARTESIAN_POINT('Ctrl Pts',(1.36347279275977,-0.906189781824136,
6.63209784173914));
#20972=CARTESIAN_POINT('Ctrl Pts',(1.34783704252929,-0.850185332091116,
6.6357194738507));
#20973=CARTESIAN_POINT('Ctrl Pts',(1.34338149796027,-0.833722956106937,
6.63677744223327));
#20974=CARTESIAN_POINT('Ctrl Pts',(1.33544736261817,-0.803457179499849,
6.63871063620847));
#20975=CARTESIAN_POINT('Ctrl Pts',(1.33192916534085,-0.789664695627758,
6.63958712275707));
#20976=CARTESIAN_POINT('Ctrl Pts',(1.32496729119795,-0.761596726930881,
6.64136184929989));
#20977=CARTESIAN_POINT('Ctrl Pts',(1.32152957394385,-0.747320100192161,
6.64225987914947));
#20978=CARTESIAN_POINT('Ctrl Pts',(1.31324314928973,-0.71184343214003,6.64448012396627));
#20979=CARTESIAN_POINT('Ctrl Pts',(1.30851117399277,-0.690616667015534,
6.64579857679885));
#20980=CARTESIAN_POINT('Ctrl Pts',(1.29130212692048,-0.609565443974385,
6.65079649226544));
#20981=CARTESIAN_POINT('Ctrl Pts',(1.2803121998971,-0.5494361356831,6.6544287047478));
#20982=CARTESIAN_POINT('Ctrl Pts',(1.25666904613559,-0.395429219256831,
6.66357084345649));
#20983=CARTESIAN_POINT('Ctrl Pts',(1.24643143758259,-0.301238787317273,
6.66901024966007));
#20984=CARTESIAN_POINT('Ctrl Pts',(1.22734227865672,-0.00426545225531576,
6.68588826779925));
#20985=CARTESIAN_POINT('Ctrl Pts',(1.23347572235375,0.198964642573343,6.69701909323654));
#20986=CARTESIAN_POINT('Ctrl Pts',(1.27219007398472,0.508263194311666,6.71477367561345));
#20987=CARTESIAN_POINT('Ctrl Pts',(1.29116959723874,0.615498497740809,6.72109074916244));
#20988=CARTESIAN_POINT('Ctrl Pts',(1.31921439696282,0.737577580902475,6.72867676931241));
#20989=CARTESIAN_POINT('Ctrl Pts',(1.32301741193638,0.753570336787383,6.72967849198895));
#20990=CARTESIAN_POINT('Ctrl Pts',(1.32935456798888,0.779342201713178,6.73130659389982));
#20991=CARTESIAN_POINT('Ctrl Pts',(1.33181268463803,0.789139938940349,6.73192879913158));
#20992=CARTESIAN_POINT('Ctrl Pts',(1.33626062447373,0.806522211024997,6.73303869694113));
#20993=CARTESIAN_POINT('Ctrl Pts',(1.33823211598968,0.814111243840464,6.73352533516172));
#20994=CARTESIAN_POINT('Ctrl Pts',(1.34256923735789,0.830559599938853,6.7345846092151));
#20995=CARTESIAN_POINT('Ctrl Pts',(1.34494495003538,0.839415905811248,6.73515779651135));
#20996=CARTESIAN_POINT('Ctrl Pts',(1.35175218751673,0.864366286028786,6.73678039073974));
#20997=CARTESIAN_POINT('Ctrl Pts',(1.35627093558577,0.880435969673518,6.73783460678149));
#20998=CARTESIAN_POINT('Ctrl Pts',(1.38605859410388,0.983294283141381,6.74463806126317));
#20999=CARTESIAN_POINT('Ctrl Pts',(1.41484249897827,1.06901487743942,6.75056208505726));
#21000=CARTESIAN_POINT('Ctrl Pts',(1.55987773123022,1.44741827309273,6.77753644088705));
#21001=CARTESIAN_POINT('Ctrl Pts',(1.7150857816945,1.72341145887595,6.79925596028994));
#21002=CARTESIAN_POINT('Ctrl Pts',(1.94648340785078,2.02239198160467,6.8235721235801));
#21003=CARTESIAN_POINT('Ctrl Pts',(1.98655474625124,2.07114014083156,6.82757537441182));
#21004=CARTESIAN_POINT('Ctrl Pts',(2.04297015749069,2.13580349802398,6.83294236377303));
#21005=CARTESIAN_POINT('Ctrl Pts',(2.05808749469571,2.15276553429368,6.83435579152175));
#21006=CARTESIAN_POINT('Ctrl Pts',(2.08240483731782,2.17947608280492,6.83659095860736));
#21007=CARTESIAN_POINT('Ctrl Pts',(2.09148824224688,2.18932927402222,6.83741756374947));
#21008=CARTESIAN_POINT('Ctrl Pts',(2.11025205306525,2.20943020098751,6.8391083058317));
#21009=CARTESIAN_POINT('Ctrl Pts',(2.11993877638182,2.21967166519366,6.83997214643809));
#21010=CARTESIAN_POINT('Ctrl Pts',(2.14252430470529,2.24323894260994,6.84196579892815));
#21011=CARTESIAN_POINT('Ctrl Pts',(2.15547164098749,2.25651771217994,6.84309347633249));
#21012=CARTESIAN_POINT('Ctrl Pts',(2.19707849418902,2.29845914963459,6.84667009963196));
#21013=CARTESIAN_POINT('Ctrl Pts',(2.22616510067534,2.32669393436031,6.84910021628417));
#21014=CARTESIAN_POINT('Ctrl Pts',(2.37995258298452,2.47044292114875,6.86160707766282));
#21015=CARTESIAN_POINT('Ctrl Pts',(2.5131216818637,2.57651303344542,6.8712818694728));
#21016=CARTESIAN_POINT('Ctrl Pts',(2.80579920626594,2.7739710629407,6.8911046832726));
#21017=CARTESIAN_POINT('Ctrl Pts',(2.96598484811098,2.86322817316442,6.90119741872582));
#21018=CARTESIAN_POINT('Ctrl Pts',(3.2091159361733,2.97274634008944,6.91655768780906));
#21019=CARTESIAN_POINT('Ctrl Pts',(3.28666395546687,3.00410787524317,6.92146593760884));
#21020=CARTESIAN_POINT('Ctrl Pts',(3.37986208188416,3.03764270456729,6.92747303888818));
#21021=CARTESIAN_POINT('Ctrl Pts',(3.39442509162186,3.04276492273715,6.92841478148956));
#21022=CARTESIAN_POINT('Ctrl Pts',(3.41829259973379,3.05096757722417,6.92996410491451));
#21023=CARTESIAN_POINT('Ctrl Pts',(3.42757552968203,3.05411061000787,6.93056814075081));
#21024=CARTESIAN_POINT('Ctrl Pts',(3.44429280328874,3.05968591186089,6.93165876948676));
#21025=CARTESIAN_POINT('Ctrl Pts',(3.45172182527721,3.06213351216891,6.93214445540951));
#21026=CARTESIAN_POINT('Ctrl Pts',(3.46810220147073,3.06746423938798,6.93321763363964));
#21027=CARTESIAN_POINT('Ctrl Pts',(3.47705717809547,3.07033520451832,6.93380580015834));
#21028=CARTESIAN_POINT('Ctrl Pts',(3.50299491118559,3.07852582193736,6.93551338886795));
#21029=CARTESIAN_POINT('Ctrl Pts',(3.52000901854027,3.08374394975419,6.93663842849694));
#21030=CARTESIAN_POINT('Ctrl Pts',(3.65388356231925,3.12359242690812,6.94552457751159));
#21031=CARTESIAN_POINT('Ctrl Pts',(3.77256848842467,3.15170535204232,6.9536009996361));
#21032=CARTESIAN_POINT('Ctrl Pts',(4.18426144440299,3.22487313080894,6.98168831383066));
#21033=CARTESIAN_POINT('Ctrl Pts',(4.48180789192737,3.23625183704567,7.00194454721374));
#21034=CARTESIAN_POINT('Ctrl Pts',(4.82841564804777,3.20163563062986,7.02420773547078));
#21035=CARTESIAN_POINT('Ctrl Pts',(4.87996476967972,3.19522563637173,7.02748949797031));
#21036=CARTESIAN_POINT('Ctrl Pts',(4.95214865905335,3.18447201250545,7.0320459773337));
#21037=CARTESIAN_POINT('Ctrl Pts',(4.97292789936862,3.18116811347642,7.03335309257909));
#21038=CARTESIAN_POINT('Ctrl Pts',(5.00657720365832,3.17547947603045,7.03546278416509));
#21039=CARTESIAN_POINT('Ctrl Pts',(5.01946745099429,3.17321945244702,7.03626928258139));
#21040=CARTESIAN_POINT('Ctrl Pts',(5.04640746463992,3.16832678368415,7.03795145636326));
#21041=CARTESIAN_POINT('Ctrl Pts',(5.06045422799504,3.1656790516403,7.03882663290923));
#21042=CARTESIAN_POINT('Ctrl Pts',(5.09386663125879,3.15915052245924,7.04090402060115));
#21043=CARTESIAN_POINT('Ctrl Pts',(5.11321526932264,3.15518496011883,7.04210350827674));
#21044=CARTESIAN_POINT('Ctrl Pts',(5.17899647375546,3.14107157214969,7.04617059025611));
#21045=CARTESIAN_POINT('Ctrl Pts',(5.22524181443309,3.13007432695933,7.04901111606527));
#21046=CARTESIAN_POINT('Ctrl Pts',(5.48754043585247,3.0615347494652,7.06504521513984));
#21047=CARTESIAN_POINT('Ctrl Pts',(5.69738702954598,2.98265627126743,7.07751761116157));
#21048=CARTESIAN_POINT('Ctrl Pts',(6.06522639528866,2.7987895192076,7.10051571123984));
#21049=CARTESIAN_POINT('Ctrl Pts',(6.22539012272862,2.70041166123858,7.11100835022457));
#21050=CARTESIAN_POINT('Ctrl Pts',(6.39748820079394,2.57279491793265,7.12385546821444));
#21051=CARTESIAN_POINT('Ctrl Pts',(6.41871159187087,2.55664489873432,7.12546964274457));
#21052=CARTESIAN_POINT('Ctrl Pts',(6.44783693839009,2.53390557615123,7.1277303225724));
#21053=CARTESIAN_POINT('Ctrl Pts',(6.45591208963528,2.52753853803787,7.12836203923669));
#21054=CARTESIAN_POINT('Ctrl Pts',(6.46973929987774,2.51652842885067,7.1294525146436));
#21055=CARTESIAN_POINT('Ctrl Pts',(6.47550616878975,2.51190396776234,7.1299099643905));
#21056=CARTESIAN_POINT('Ctrl Pts',(6.48743269058432,2.50227246591128,7.13086164948699));
#21057=CARTESIAN_POINT('Ctrl Pts',(6.49358980242966,2.49726246898597,7.13135610806044));
#21058=CARTESIAN_POINT('Ctrl Pts',(6.50817992737085,2.48530072887005,7.1325351749779));
#21059=CARTESIAN_POINT('Ctrl Pts',(6.51659617652789,2.47832876201568,7.13322121623042));
#21060=CARTESIAN_POINT('Ctrl Pts',(6.53484804685455,2.46305181707763,7.13472159508525));
#21061=CARTESIAN_POINT('Ctrl Pts',(6.54466965867426,2.45473047700132,7.13553703171702));
#21062=CARTESIAN_POINT('Ctrl Pts',(6.57197446462373,2.43131408169053,7.13782600052415));
#21063=CARTESIAN_POINT('Ctrl Pts',(6.58934527016644,2.41608987603887,7.13930767106706));
#21064=CARTESIAN_POINT('Ctrl Pts',(6.6463100814323,2.36507144113298,7.14424740557378));
#21065=CARTESIAN_POINT('Ctrl Pts',(6.68517690344684,2.32848176934814,7.14774929396284));
#21066=CARTESIAN_POINT('Ctrl Pts',(6.83331788943999,2.18191211754013,7.16156337650518));
#21067=CARTESIAN_POINT('Ctrl Pts',(6.93550628735614,2.06507209879258,7.17211448946801));
#21068=CARTESIAN_POINT('Ctrl Pts',(7.1504020014744,1.78031894256516,7.19619460345784));
#21069=CARTESIAN_POINT('Ctrl Pts',(7.25654816552784,1.60822620632392,7.20959062731156));
#21070=CARTESIAN_POINT('Ctrl Pts',(7.36443838644642,1.38981344704689,7.22505398471197));
#21071=CARTESIAN_POINT('Ctrl Pts',(7.38223031454333,1.35195723613556,7.22768387625487));
#21072=CARTESIAN_POINT('Ctrl Pts',(7.40685318288468,1.29680237324319,7.23144520197996));
#21073=CARTESIAN_POINT('Ctrl Pts',(7.41427869972579,1.27977538138872,7.23259686494628));
#21074=CARTESIAN_POINT('Ctrl Pts',(7.42710082773345,1.24966594207764,7.23461699180284));
#21075=CARTESIAN_POINT('Ctrl Pts',(7.43255920487138,1.23661049911037,7.23548753724335));
#21076=CARTESIAN_POINT('Ctrl Pts',(7.44367386923792,1.20952637217369,7.23728259964956));
#21077=CARTESIAN_POINT('Ctrl Pts',(7.44931774371867,1.19549294704685,7.23820668011825));
#21078=CARTESIAN_POINT('Ctrl Pts',(7.46359340724234,1.15926192538388,7.24057730334684));
#21079=CARTESIAN_POINT('Ctrl Pts',(7.47207840752938,1.13700719516733,7.2420189073332));
#21080=CARTESIAN_POINT('Ctrl Pts',(7.50755730295076,1.04076013059023,7.24819357147067));
#21081=CARTESIAN_POINT('Ctrl Pts',(7.53208173391118,0.965882643633223,7.25284475361226));
#21082=CARTESIAN_POINT('Ctrl Pts',(7.5919332169537,0.757629425777134,7.26544293426783));
#21083=CARTESIAN_POINT('Ctrl Pts',(7.62148147420242,0.622766670066883,7.27322356150208));
#21084=CARTESIAN_POINT('Ctrl Pts',(7.66687941955569,0.325430162093823,7.2900710493035));
#21085=CARTESIAN_POINT('Ctrl Pts',(7.67921910621661,0.162824882296941,7.29909016486001));
#21086=CARTESIAN_POINT('Ctrl Pts',(7.67921910621823,3.21015783399936E-11,
7.30846150265207));
#21087=CARTESIAN_POINT('Origin',(4.45646910621825,-5.13094777615093E-16,
-2.31077344927308));
#21088=CARTESIAN_POINT('Ctrl Pts',(6.37917568135534,-2.58637139413976,3.74329856950612));
#21089=CARTESIAN_POINT('Ctrl Pts',(6.34981776169284,-2.60819604983126,3.74545795803728));
#21090=CARTESIAN_POINT('Ctrl Pts',(6.32008641473289,-2.62952220215757,3.74764227516074));
#21091=CARTESIAN_POINT('Ctrl Pts',(6.27627241956155,-2.65983305279075,3.75086776268092));
#21092=CARTESIAN_POINT('Ctrl Pts',(6.26247734541822,-2.66921902081475,3.75188424917421));
#21093=CARTESIAN_POINT('Ctrl Pts',(6.24024382473343,-2.68409512710286,3.75352506513817));
#21094=CARTESIAN_POINT('Ctrl Pts',(6.2318512533263,-2.68965371807077,3.75414500494344));
#21095=CARTESIAN_POINT('Ctrl Pts',(6.21686488041954,-2.69947883145809,3.75525329482638));
#21096=CARTESIAN_POINT('Ctrl Pts',(6.21028135030926,-2.70376068730008,3.75574061418644));
#21097=CARTESIAN_POINT('Ctrl Pts',(6.19605368380114,-2.7129403748258,3.75679479687359));
#21098=CARTESIAN_POINT('Ctrl Pts',(6.18840461162385,-2.71782990274919,3.75736216293192));
#21099=CARTESIAN_POINT('Ctrl Pts',(6.16698862995532,-2.7313925521135,3.75895217233337));
#21100=CARTESIAN_POINT('Ctrl Pts',(6.15317676597574,-2.73999368727886,3.75997933010706));
#21101=CARTESIAN_POINT('Ctrl Pts',(6.06956539130074,-2.79118684463646,3.76620477497964));
#21102=CARTESIAN_POINT('Ctrl Pts',(5.99823637780219,-2.83121085230435,3.77154622617879));
#21103=CARTESIAN_POINT('Ctrl Pts',(5.7814661209703,-2.94222300142046,3.78770402297351));
#21104=CARTESIAN_POINT('Ctrl Pts',(5.63211739923204,-3.00501951589682,3.79872786137717));
#21105=CARTESIAN_POINT('Ctrl Pts',(5.27890143948994,-3.12315587311417,3.82384093072569));
#21106=CARTESIAN_POINT('Ctrl Pts',(5.07301360408779,-3.17023649998643,3.83776623513276));
#21107=CARTESIAN_POINT('Ctrl Pts',(4.8367836126848,-3.20034835269865,3.85276057963487));
#21108=CARTESIAN_POINT('Ctrl Pts',(4.809552911355,-3.20346696620147,3.85447537845611));
#21109=CARTESIAN_POINT('Ctrl Pts',(4.76486261607714,-3.20800836676478,3.85726799192259));
#21110=CARTESIAN_POINT('Ctrl Pts',(4.74742577447629,-3.20963681352515,3.85835220141562));
#21111=CARTESIAN_POINT('Ctrl Pts',(4.71605383436079,-3.21230891589858,3.86029345916461));
#21112=CARTESIAN_POINT('Ctrl Pts',(4.70212368809387,-3.21340421335462,3.86115210538209));
#21113=CARTESIAN_POINT('Ctrl Pts',(4.672397011315,-3.21554712476631,3.86297751253728));
#21114=CARTESIAN_POINT('Ctrl Pts',(4.65659895248147,-3.21656901533518,3.86394344645148));
#21115=CARTESIAN_POINT('Ctrl Pts',(4.61379440963783,-3.21902122856369,3.86654972858248));
#21116=CARTESIAN_POINT('Ctrl Pts',(4.58677603899122,-3.22022811179088,3.86818307653523));
#21117=CARTESIAN_POINT('Ctrl Pts',(4.44114121931691,-3.22489750916803,3.87692844797836));
#21118=CARTESIAN_POINT('Ctrl Pts',(4.32241035730945,-3.22214705596425,3.88384379947539));
#21119=CARTESIAN_POINT('Ctrl Pts',(4.04933038358868,-3.20069590628345,3.89950347711698));
#21120=CARTESIAN_POINT('Ctrl Pts',(3.89564590314937,-3.17737245428039,3.90812982625756));
#21121=CARTESIAN_POINT('Ctrl Pts',(3.57940300272826,-3.10571072657916,3.92628648859027));
#21122=CARTESIAN_POINT('Ctrl Pts',(3.41777903146608,-3.05545299974991,3.93580372816945));
#21123=CARTESIAN_POINT('Ctrl Pts',(3.23585077852002,-2.98277285361419,3.94754794881669));
#21124=CARTESIAN_POINT('Ctrl Pts',(3.21096611919768,-2.9724678635729,3.94917784262253));
#21125=CARTESIAN_POINT('Ctrl Pts',(3.17672933363865,-2.95778467653029,3.95145680682462));
#21126=CARTESIAN_POINT('Ctrl Pts',(3.1672639395666,-2.95367129345696,3.9520907675041));
#21127=CARTESIAN_POINT('Ctrl Pts',(3.15104430451888,-2.94652989757682,3.95318408480818));
#21128=CARTESIAN_POINT('Ctrl Pts',(3.14428036887951,-2.94352391959094,3.95364211688344));
#21129=CARTESIAN_POINT('Ctrl Pts',(3.13014465865495,-2.93718342715595,3.95460385618622));
#21130=CARTESIAN_POINT('Ctrl Pts',(3.12277503659694,-2.93384443155106,3.95510784792173));
#21131=CARTESIAN_POINT('Ctrl Pts',(3.10474858220154,-2.92559513064642,3.95634686079197));
#21132=CARTESIAN_POINT('Ctrl Pts',(3.09410590327748,-2.92065433366923,3.95708371473344));
#21133=CARTESIAN_POINT('Ctrl Pts',(3.05550885142972,-2.90247903176341,3.95977487505274));
#21134=CARTESIAN_POINT('Ctrl Pts',(3.02771938106358,-2.88890086780487,3.96174861661637));
#21135=CARTESIAN_POINT('Ctrl Pts',(2.95839315810366,-2.85378259030085,3.96675603041624));
#21136=CARTESIAN_POINT('Ctrl Pts',(2.91712289139339,-2.83173434590594,3.96981356369938));
#21137=CARTESIAN_POINT('Ctrl Pts',(2.58473013705096,-2.64474312009241,3.9949868584153));
#21138=CARTESIAN_POINT('Ctrl Pts',(2.3204092414957,-2.43626750367108,4.01819928517467));
#21139=CARTESIAN_POINT('Ctrl Pts',(2.04852514414407,-2.14293717908672,4.04395289853798));
#21140=CARTESIAN_POINT('Ctrl Pts',(2.00563630643055,-2.09375104874505,4.04809600219894));
#21141=CARTESIAN_POINT('Ctrl Pts',(1.9496742259047,-2.02549420697816,4.05361790596751));
#21142=CARTESIAN_POINT('Ctrl Pts',(1.93527162700832,-2.0075384602635,4.05505015026933));
#21143=CARTESIAN_POINT('Ctrl Pts',(1.91183183465776,-1.9776658730033,4.05740010762631));
#21144=CARTESIAN_POINT('Ctrl Pts',(1.90268320552073,-1.9658379217199,4.05832223824882));
#21145=CARTESIAN_POINT('Ctrl Pts',(1.88499002633847,-1.94263104364197,4.06011551552755));
#21146=CARTESIAN_POINT('Ctrl Pts',(1.87643787707972,-1.93125837134497,4.06098694855694));
#21147=CARTESIAN_POINT('Ctrl Pts',(1.85641545098851,-1.90426211275478,4.06303843772651));
#21148=CARTESIAN_POINT('Ctrl Pts',(1.84501015790563,-1.88859084790915,4.06421595315793));
#21149=CARTESIAN_POINT('Ctrl Pts',(1.80741981421603,-1.8359487502541,4.06812801253917));
#21150=CARTESIAN_POINT('Ctrl Pts',(1.78187232017805,-1.79852781535277,4.0708382650619));
#21151=CARTESIAN_POINT('Ctrl Pts',(1.72265089645832,-1.70772859580557,4.07725871707347));
#21152=CARTESIAN_POINT('Ctrl Pts',(1.68973867083592,-1.65387495270192,4.08094202096787));
#21153=CARTESIAN_POINT('Ctrl Pts',(1.49090226071539,-1.30595609949559,4.10406427265169));
#21154=CARTESIAN_POINT('Ctrl Pts',(1.37050983471422,-0.988380628069924,
4.12195529580339));
#21155=CARTESIAN_POINT('Ctrl Pts',(1.29400965244306,-0.621570516594846,
4.14420823992934));
#21156=CARTESIAN_POINT('Ctrl Pts',(1.28705016136918,-0.585049559637317,
4.14644298120553));
#21157=CARTESIAN_POINT('Ctrl Pts',(1.27850885236505,-0.535589097740135,
4.14950520689873));
#21158=CARTESIAN_POINT('Ctrl Pts',(1.27637120165279,-0.522746937552845,
4.15030353293756));
#21159=CARTESIAN_POINT('Ctrl Pts',(1.27311994748278,-0.502456376911369,
4.15157048580155));
#21160=CARTESIAN_POINT('Ctrl Pts',(1.27195451545177,-0.495016257898872,
4.15203623686493));
#21161=CARTESIAN_POINT('Ctrl Pts',(1.26960594735517,-0.479671402352096,
4.15299939449796));
#21162=CARTESIAN_POINT('Ctrl Pts',(1.26842613643813,-0.471766324443939,
4.15349699514388));
#21163=CARTESIAN_POINT('Ctrl Pts',(1.26566261849829,-0.452766090444523,
4.15469629780726));
#21164=CARTESIAN_POINT('Ctrl Pts',(1.26410736828276,-0.441666956134685,
4.15539956997679));
#21165=CARTESIAN_POINT('Ctrl Pts',(1.25893158098884,-0.403273398896135,
4.15784105658939));
#21166=CARTESIAN_POINT('Ctrl Pts',(1.25560306922828,-0.375941690990998,
4.1595943943965));
#21167=CARTESIAN_POINT('Ctrl Pts',(1.24829523057348,-0.308772817516369,
4.16393529758366));
#21168=CARTESIAN_POINT('Ctrl Pts',(1.2447073437145,-0.268898410902722,4.16653975920778));
#21169=CARTESIAN_POINT('Ctrl Pts',(1.23301500006768,-0.104744289972911,
4.1773478629858));
#21170=CARTESIAN_POINT('Ctrl Pts',(1.23137548864601,0.0198822758279329,
4.18575170872378));
#21171=CARTESIAN_POINT('Ctrl Pts',(1.24849105400465,0.401797934962905,4.2116107241368));
#21172=CARTESIAN_POINT('Ctrl Pts',(1.29088872305006,0.65704943899393,4.22894975426185));
#21173=CARTESIAN_POINT('Ctrl Pts',(1.37327146098075,0.938765450359666,4.24755331344584));
#21174=CARTESIAN_POINT('Ctrl Pts',(1.38384411194963,0.972812468348576,4.24979457995541));
#21175=CARTESIAN_POINT('Ctrl Pts',(1.40057205092747,1.02368513667787,4.25313381711095));
#21176=CARTESIAN_POINT('Ctrl Pts',(1.40630597499971,1.04064545609906,4.25424545897899));
#21177=CARTESIAN_POINT('Ctrl Pts',(1.41649451849129,1.06997422983963,4.25616519936816));
#21178=CARTESIAN_POINT('Ctrl Pts',(1.4208839889695,1.08236470315842,4.25697542637545));
#21179=CARTESIAN_POINT('Ctrl Pts',(1.43018871229421,1.10812793290962,4.25865857486128));
#21180=CARTESIAN_POINT('Ctrl Pts',(1.43511708969751,1.12149567136304,4.25953103913061));
#21181=CARTESIAN_POINT('Ctrl Pts',(1.44699531154754,1.15306752166063,4.26158978569447));
#21182=CARTESIAN_POINT('Ctrl Pts',(1.45402197571662,1.17124228264011,4.26277347616694));
#21183=CARTESIAN_POINT('Ctrl Pts',(1.4781601175877,1.23203158785901,4.26672863672215));
#21184=CARTESIAN_POINT('Ctrl Pts',(1.4960179203447,1.2743450706152,4.26947505950246));
#21185=CARTESIAN_POINT('Ctrl Pts',(1.54100919453519,1.37489524231377,4.27599670165879));
#21186=CARTESIAN_POINT('Ctrl Pts',(1.56899179505691,1.43273128526529,4.27974383347161));
#21187=CARTESIAN_POINT('Ctrl Pts',(1.68614662446461,1.65747737194452,4.29435702941941));
#21188=CARTESIAN_POINT('Ctrl Pts',(1.78821310664888,1.81723184052764,4.30483681489048));
#21189=CARTESIAN_POINT('Ctrl Pts',(1.95458853839343,2.03314026340757,4.32011603201655));
#21190=CARTESIAN_POINT('Ctrl Pts',(2.00800795817604,2.09716537979181,4.32481153799596));
#21191=CARTESIAN_POINT('Ctrl Pts',(2.12497231191156,2.22678357875538,4.33483072751014));
#21192=CARTESIAN_POINT('Ctrl Pts',(2.18894135851257,2.29188942760255,4.34016729457898));
#21193=CARTESIAN_POINT('Ctrl Pts',(2.26713397731344,2.36499037359676,4.34665564810149));
#21194=CARTESIAN_POINT('Ctrl Pts',(2.27876803591371,2.37570743132216,4.34762018773588));
#21195=CARTESIAN_POINT('Ctrl Pts',(2.29782246684684,2.39300241732182,4.34919948698004));
#21196=CARTESIAN_POINT('Ctrl Pts',(2.30519529004754,2.39963264787468,4.34981046784696));
#21197=CARTESIAN_POINT('Ctrl Pts',(2.31844298864866,2.41143591186017,4.35090835951223));
#21198=CARTESIAN_POINT('Ctrl Pts',(2.32430624967556,2.41662168891636,4.35139430679078));
#21199=CARTESIAN_POINT('Ctrl Pts',(2.33718366443557,2.42792780618445,4.35246171272344));
#21200=CARTESIAN_POINT('Ctrl Pts',(2.34420536408459,2.43403904947004,4.35304379614867));
#21201=CARTESIAN_POINT('Ctrl Pts',(2.36438624339256,2.45145012378544,4.35471665573849));
#21202=CARTESIAN_POINT('Ctrl Pts',(2.37761007141598,2.4626740540899,4.35581271206401));
#21203=CARTESIAN_POINT('Ctrl Pts',(2.47296777821088,2.54229506459685,4.36371162673015));
#21204=CARTESIAN_POINT('Ctrl Pts',(2.55836112002222,2.60666895006234,4.37075801376289));
#21205=CARTESIAN_POINT('Ctrl Pts',(2.83305520814657,2.79308451442682,4.39297258558839));
#21206=CARTESIAN_POINT('Ctrl Pts',(3.03207974890739,2.89964181234241,4.40839355098079));
#21207=CARTESIAN_POINT('Ctrl Pts',(3.35531660206728,3.03132453995996,4.43144666662687));
#21208=CARTESIAN_POINT('Ctrl Pts',(3.47265726603864,3.07141433160756,4.43945657855958));
#21209=CARTESIAN_POINT('Ctrl Pts',(3.61909755986484,3.11218829764507,4.44901240631823));
#21210=CARTESIAN_POINT('Ctrl Pts',(3.64626477154127,3.11937111018519,4.45076733456801));
#21211=CARTESIAN_POINT('Ctrl Pts',(3.68926226790782,3.1301396913184,4.45351751064787));
#21212=CARTESIAN_POINT('Ctrl Pts',(3.70503114552755,3.13396263962135,4.45452035199704));
#21213=CARTESIAN_POINT('Ctrl Pts',(3.73439664985469,3.1408475202904,4.45637742154078));
#21214=CARTESIAN_POINT('Ctrl Pts',(3.74798550034312,3.14394064317625,4.45723263252117));
#21215=CARTESIAN_POINT('Ctrl Pts',(3.77817207408652,3.15060612036469,4.45912342639666));
#21216=CARTESIAN_POINT('Ctrl Pts',(3.79477889718563,3.15413567779364,4.46015761974628));
#21217=CARTESIAN_POINT('Ctrl Pts',(3.84319676355824,3.16402701615015,4.46315592129958));
#21218=CARTESIAN_POINT('Ctrl Pts',(3.87507749553923,3.17004003690818,4.46510892966774));
#21219=CARTESIAN_POINT('Ctrl Pts',(4.11684838740508,3.21187027401117,4.47977122939964));
#21220=CARTESIAN_POINT('Ctrl Pts',(4.32974136686386,3.22729122010331,4.49179076533305));
#21221=CARTESIAN_POINT('Ctrl Pts',(4.76628115782701,3.21561702101713,4.5162261782402));
#21222=CARTESIAN_POINT('Ctrl Pts',(4.98867702377822,3.18636199397078,4.52857811974589));
#21223=CARTESIAN_POINT('Ctrl Pts',(5.23039511307756,3.12854187097451,4.54350880611434));
#21224=CARTESIAN_POINT('Ctrl Pts',(5.25450679679479,3.12247841648598,4.54501563242105));
#21225=CARTESIAN_POINT('Ctrl Pts',(5.28820028659546,3.11358965140443,4.54714890814396));
#21226=CARTESIAN_POINT('Ctrl Pts',(5.29784346338925,3.11099766292469,4.54776265004838));
#21227=CARTESIAN_POINT('Ctrl Pts',(5.31453069110011,3.10642904378486,4.5488304974479));
#21228=CARTESIAN_POINT('Ctrl Pts',(5.32158040991493,3.10447314648003,4.54928341714026));
#21229=CARTESIAN_POINT('Ctrl Pts',(5.33650045337289,3.10027891376274,4.55024590240835));
#21230=CARTESIAN_POINT('Ctrl Pts',(5.34436899384271,3.09803458669996,4.55075582228102));
#21231=CARTESIAN_POINT('Ctrl Pts',(5.36393354250173,3.09237357561683,4.55202934293306));
#21232=CARTESIAN_POINT('Ctrl Pts',(5.37561878692755,3.08892050522273,4.55279500592538));
#21233=CARTESIAN_POINT('Ctrl Pts',(5.41992743804611,3.07555331380205,4.55571668153471));
#21234=CARTESIAN_POINT('Ctrl Pts',(5.45241109207888,3.06518832818375,4.55789661161878));
#21235=CARTESIAN_POINT('Ctrl Pts',(5.53537963606106,3.03725642689589,4.56355175364656));
#21236=CARTESIAN_POINT('Ctrl Pts',(5.58560185195019,3.01894570199932,4.56705877981558));
#21237=CARTESIAN_POINT('Ctrl Pts',(5.83774851215238,2.91984273290741,4.58501856159581));
#21238=CARTESIAN_POINT('Ctrl Pts',(6.03158176459205,2.82000689038689,4.59994010379897));
#21239=CARTESIAN_POINT('Ctrl Pts',(6.34631745079664,2.61525352573873,4.62499961077273));
#21240=CARTESIAN_POINT('Ctrl Pts',(6.47224825476557,2.51946920452413,4.63530723888649));
#21241=CARTESIAN_POINT('Ctrl Pts',(6.61087638948587,2.39695114043158,4.64695182020448));
#21242=CARTESIAN_POINT('Ctrl Pts',(6.63086830738769,2.37883032116423,4.64863946606084));
#21243=CARTESIAN_POINT('Ctrl Pts',(6.66336265076748,2.34862525947712,4.65139702453477));
#21244=CARTESIAN_POINT('Ctrl Pts',(6.67599873016896,2.33668739753253,4.65247306345761));
#21245=CARTESIAN_POINT('Ctrl Pts',(6.6986088087269,2.31497776437926,4.65440543176101));
#21246=CARTESIAN_POINT('Ctrl Pts',(6.70861699119395,2.30524237534058,4.655263298122));
#21247=CARTESIAN_POINT('Ctrl Pts',(6.72790905935415,2.28623059358038,4.65692202656086));
#21248=CARTESIAN_POINT('Ctrl Pts',(6.73720015398694,2.27696194158973,4.65772320146893));
#21249=CARTESIAN_POINT('Ctrl Pts',(6.76220300293278,2.25171289762537,4.65988576667305));
#21250=CARTESIAN_POINT('Ctrl Pts',(6.77780529485408,2.23562477037519,4.66124235479986));
#21251=CARTESIAN_POINT('Ctrl Pts',(6.84409876582088,2.16582467693333,4.66703925873701));
#21252=CARTESIAN_POINT('Ctrl Pts',(6.89310548850275,2.11053933878044,4.67140774922145));
#21253=CARTESIAN_POINT('Ctrl Pts',(7.0200473036631,1.9570121681029,4.68301698341837));
#21254=CARTESIAN_POINT('Ctrl Pts',(7.09422246918846,1.85582609554176,4.69012332222034));
#21255=CARTESIAN_POINT('Ctrl Pts',(7.17200284155761,1.73560132735333,4.69816286885749));
#21256=CARTESIAN_POINT('Ctrl Pts',(7.18156139451602,1.72055434209397,4.69916231235919));
#21257=CARTESIAN_POINT('Ctrl Pts',(7.19099309084831,1.70543136478218,4.70016067061871));
#21258=CARTESIAN_POINT('Origin',(4.45646910621825,-5.13094777615093E-16,
-2.31077344927308));
#21259=CARTESIAN_POINT('Ctrl Pts',(6.37918196868372,-2.58636672013265,2.49808050559515));
#21260=CARTESIAN_POINT('Ctrl Pts',(6.28518486951706,-2.65624444868342,2.50481557244532));
#21261=CARTESIAN_POINT('Ctrl Pts',(6.18739743632227,-2.72098388076692,2.51140426454075));
#21262=CARTESIAN_POINT('Ctrl Pts',(5.89937864052687,-2.88981760055554,2.53009003280362));
#21263=CARTESIAN_POINT('Ctrl Pts',(5.70197263437052,-2.98022328862117,2.54204479930428));
#21264=CARTESIAN_POINT('Ctrl Pts',(5.46564045093849,-3.06084797756682,2.55693518690676));
#21265=CARTESIAN_POINT('Ctrl Pts',(5.4340945393033,-3.07106910732803,2.55893472520474));
#21266=CARTESIAN_POINT('Ctrl Pts',(5.39087364308137,-3.08433964641135,2.56169762132471));
#21267=CARTESIAN_POINT('Ctrl Pts',(5.37932977043503,-3.08781331635947,2.56243781562696));
#21268=CARTESIAN_POINT('Ctrl Pts',(5.3599441385493,-3.09352823525713,2.56368501597441));
#21269=CARTESIAN_POINT('Ctrl Pts',(5.35211273340421,-3.09580467196993,2.56419000257694));
#21270=CARTESIAN_POINT('Ctrl Pts',(5.33721807588775,-3.1000730107221,2.56515275866065));
#21271=CARTESIAN_POINT('Ctrl Pts',(5.33015650855711,-3.10207055687392,2.56561018281042));
#21272=CARTESIAN_POINT('Ctrl Pts',(5.31338352422811,-3.10675341247277,2.56669890190203));
#21273=CARTESIAN_POINT('Ctrl Pts',(5.30366628195886,-3.10941731274112,2.56733140317273));
#21274=CARTESIAN_POINT('Ctrl Pts',(5.2694152088243,-3.11863448547352,2.5695666371848));
#21275=CARTESIAN_POINT('Ctrl Pts',(5.24481728974322,-3.12494311441454,2.57118237184543));
#21276=CARTESIAN_POINT('Ctrl Pts',(5.0101758211773,-3.18217501660275,2.586677651492));
#21277=CARTESIAN_POINT('Ctrl Pts',(4.79560105169467,-3.21213399893489,2.60143593171232));
#21278=CARTESIAN_POINT('Ctrl Pts',(4.42874664045629,-3.22616768330515,2.62622546111055));
#21279=CARTESIAN_POINT('Ctrl Pts',(4.27759830218279,-3.22132586397863,2.63632107142302));
#21280=CARTESIAN_POINT('Ctrl Pts',(4.07233574230635,-3.20025245081135,2.64971826259662));
#21281=CARTESIAN_POINT('Ctrl Pts',(4.01749002079987,-3.19319152827772,2.65326866444437));
#21282=CARTESIAN_POINT('Ctrl Pts',(3.92239140019319,-3.17845163905746,2.65937374019091));
#21283=CARTESIAN_POINT('Ctrl Pts',(3.88205417113569,-3.17141002522392,2.66194719425168));
#21284=CARTESIAN_POINT('Ctrl Pts',(3.8235823979692,-3.16005042311833,2.66565569211455));
#21285=CARTESIAN_POINT('Ctrl Pts',(3.80533508374427,-3.15634104149528,2.66680989101781));
#21286=CARTESIAN_POINT('Ctrl Pts',(3.77332093682859,-3.14954364276837,2.66882968781259));
#21287=CARTESIAN_POINT('Ctrl Pts',(3.75954046034546,-3.14652300987291,2.66969740912508));
#21288=CARTESIAN_POINT('Ctrl Pts',(3.73273209211697,-3.14046194843547,2.67138231401274));
#21289=CARTESIAN_POINT('Ctrl Pts',(3.71970244092451,-3.13743070115226,2.67219977155121));
#21290=CARTESIAN_POINT('Ctrl Pts',(3.68471521075411,-3.12906121692898,2.67439111296566));
#21291=CARTESIAN_POINT('Ctrl Pts',(3.66279402101405,-3.12357296592664,2.67576016230111));
#21292=CARTESIAN_POINT('Ctrl Pts',(3.58074919234202,-3.1021125007785,2.68087108200045));
#21293=CARTESIAN_POINT('Ctrl Pts',(3.52103220021034,-3.08463059183433,2.68456435968236));
#21294=CARTESIAN_POINT('Ctrl Pts',(3.45424201160977,-3.06295975853678,2.68867919591175));
#21295=CARTESIAN_POINT('Ctrl Pts',(3.44663761583096,-3.06046107540552,2.68914746152703));
#21296=CARTESIAN_POINT('Ctrl Pts',(3.12513042069685,-2.95349017741802,2.70893700938461));
#21297=CARTESIAN_POINT('Ctrl Pts',(2.8292185517356,-2.80135398063382,2.72657394649185));
#21298=CARTESIAN_POINT('Ctrl Pts',(2.52393355506871,-2.5794570656971,2.74849368113489));
#21299=CARTESIAN_POINT('Ctrl Pts',(2.48681181532542,-2.55122365500893,2.75123502302096));
#21300=CARTESIAN_POINT('Ctrl Pts',(2.42617007866204,-2.50298929888503,2.75586531428964));
#21301=CARTESIAN_POINT('Ctrl Pts',(2.40230062469231,-2.48343738836674,2.7577286269456));
#21302=CARTESIAN_POINT('Ctrl Pts',(2.3697554610113,-2.45598883286712,2.76033189838433));
#21303=CARTESIAN_POINT('Ctrl Pts',(2.36083581310995,-2.44838233844631,2.76105201701385));
#21304=CARTESIAN_POINT('Ctrl Pts',(2.34583218041234,-2.43544549422176,2.76227498505889));
#21305=CARTESIAN_POINT('Ctrl Pts',(2.33972629396624,-2.43014050065552,2.76277598770714));
#21306=CARTESIAN_POINT('Ctrl Pts',(2.32806951112227,-2.41993544303534,2.76373894129266));
#21307=CARTESIAN_POINT('Ctrl Pts',(2.32251543657167,-2.41503915455816,2.76420059569364));
#21308=CARTESIAN_POINT('Ctrl Pts',(2.30925339980471,-2.40326631337749,2.76530964834268));
#21309=CARTESIAN_POINT('Ctrl Pts',(2.301561586026,-2.39637180660293,2.76595835667477));
#21310=CARTESIAN_POINT('Ctrl Pts',(2.27388432162737,-2.37132246648406,2.76831201436388));
#21311=CARTESIAN_POINT('Ctrl Pts',(2.25409470102397,-2.352954196432,2.77003179610513));
#21312=CARTESIAN_POINT('Ctrl Pts',(2.10913893262197,-2.21497876568062,2.78288992630603));
#21313=CARTESIAN_POINT('Ctrl Pts',(1.99357236233124,-2.08571771221435,2.79459093805212));
#21314=CARTESIAN_POINT('Ctrl Pts',(1.77964809002725,-1.80373364151393,2.81853648892629));
#21315=CARTESIAN_POINT('Ctrl Pts',(1.68265191754336,-1.65068982538436,2.83073398126935));
#21316=CARTESIAN_POINT('Ctrl Pts',(1.57068087793179,-1.43599959830357,2.84652031534988));
#21317=CARTESIAN_POINT('Ctrl Pts',(1.54391146500114,-1.38089728593823,2.85046657104193));
#21318=CARTESIAN_POINT('Ctrl Pts',(1.50051835996936,-1.28469220993171,2.85717645664701));
#21319=CARTESIAN_POINT('Ctrl Pts',(1.48314282106256,-1.24394935739802,2.85996428431486));
#21320=CARTESIAN_POINT('Ctrl Pts',(1.45944244009449,-1.18503911163739,2.86392058197347));
#21321=CARTESIAN_POINT('Ctrl Pts',(1.45243235860227,-1.16715456480946,2.86511198028158));
#21322=CARTESIAN_POINT('Ctrl Pts',(1.4405188916409,-1.1359416812938,2.86717476595096));
#21323=CARTESIAN_POINT('Ctrl Pts',(1.43554298274396,-1.12264178030261,2.86804856143227));
#21324=CARTESIAN_POINT('Ctrl Pts',(1.42548784973079,-1.09521483653803,2.86984007626873));
#21325=CARTESIAN_POINT('Ctrl Pts',(1.42041909753476,-1.08108430387859,2.87075742951432));
#21326=CARTESIAN_POINT('Ctrl Pts',(1.40773843960834,-1.04494084332239,2.87308978931931));
#21327=CARTESIAN_POINT('Ctrl Pts',(1.40026601470624,-1.02287963642323,2.8745001659332));
#21328=CARTESIAN_POINT('Ctrl Pts',(1.37212289717023,-0.936728658827347,
2.87995846036124));
#21329=CARTESIAN_POINT('Ctrl Pts',(1.35322291445947,-0.872075765366114,
2.88394860285795));
#21330=CARTESIAN_POINT('Ctrl Pts',(1.25319919964049,-0.485293519959753,
2.90729526881307));
#21331=CARTESIAN_POINT('Ctrl Pts',(1.22026002972698,-0.152839572016994,
2.92499853874331));
#21332=CARTESIAN_POINT('Ctrl Pts',(1.24126974780216,0.225367357612319,2.94699749744975));
#21333=CARTESIAN_POINT('Ctrl Pts',(1.24487190547074,0.271919749776895,2.94974184704032));
#21334=CARTESIAN_POINT('Ctrl Pts',(1.25253447154715,0.349104611388237,2.95437674566911));
#21335=CARTESIAN_POINT('Ctrl Pts',(1.25602655436483,0.379787421653811,2.9562415926886));
#21336=CARTESIAN_POINT('Ctrl Pts',(1.26145220339481,0.422045098901182,2.95884666759168));
#21337=CARTESIAN_POINT('Ctrl Pts',(1.26300901467856,0.433667739988653,2.95956701934933));
#21338=CARTESIAN_POINT('Ctrl Pts',(1.26574688723206,0.45329319608573,2.96079026815489));
#21339=CARTESIAN_POINT('Ctrl Pts',(1.26689473232787,0.46130067419336,2.96129131646005));
#21340=CARTESIAN_POINT('Ctrl Pts',(1.26915080822516,0.476628199260626,2.96225426473321));
#21341=CARTESIAN_POINT('Ctrl Pts',(1.27025413235005,0.483948872025284,2.96271586758078));
#21342=CARTESIAN_POINT('Ctrl Pts',(1.27295679562112,0.501471402258538,2.9638246723081));
#21343=CARTESIAN_POINT('Ctrl Pts',(1.27457995202293,0.511669427076917,2.96447318298709));
#21344=CARTESIAN_POINT('Ctrl Pts',(1.28062047076585,0.548480422393644,2.96682516733172));
#21345=CARTESIAN_POINT('Ctrl Pts',(1.28532280188968,0.575044637444286,2.96854344572162));
#21346=CARTESIAN_POINT('Ctrl Pts',(1.32135561407563,0.764695896638454,2.98094646137619));
#21347=CARTESIAN_POINT('Ctrl Pts',(1.36491486366795,0.92519096521642,2.99214979649443));
#21348=CARTESIAN_POINT('Ctrl Pts',(1.4734228316176,1.22975116498648,3.01401992145856));
#21349=CARTESIAN_POINT('Ctrl Pts',(1.536984695453,1.37385251149684,3.02465417590375));
#21350=CARTESIAN_POINT('Ctrl Pts',(1.6668715864945,1.61818507147743,3.04288998801567));
#21351=CARTESIAN_POINT('Ctrl Pts',(1.72874586729189,1.7204386016444,3.05059479169305));
#21352=CARTESIAN_POINT('Ctrl Pts',(1.81145160979574,1.84139454919563,3.0597956226882));
#21353=CARTESIAN_POINT('Ctrl Pts',(1.82702398548475,1.86356375561464,3.06148602139075));
#21354=CARTESIAN_POINT('Ctrl Pts',(1.85214241964481,1.89838115334209,3.06414795433224));
#21355=CARTESIAN_POINT('Ctrl Pts',(1.86150512405357,1.91115944895919,3.06512645882332));
#21356=CARTESIAN_POINT('Ctrl Pts',(1.87930227642939,1.9350772325466,3.0669611168412));
#21357=CARTESIAN_POINT('Ctrl Pts',(1.88771565622375,1.94623186885487,3.06781805980918));
#21358=CARTESIAN_POINT('Ctrl Pts',(1.90682805857651,1.97123165260524,3.06974179535838));
#21359=CARTESIAN_POINT('Ctrl Pts',(1.91756788227919,1.98504516168025,3.07080695213981));
#21360=CARTESIAN_POINT('Ctrl Pts',(1.94538628085664,2.02022992844962,3.07352624448694));
#21361=CARTESIAN_POINT('Ctrl Pts',(1.96262564563155,2.04147269956306,3.07517395835823));
#21362=CARTESIAN_POINT('Ctrl Pts',(2.11072293195473,2.21928585009176,3.08902464733973));
#21363=CARTESIAN_POINT('Ctrl Pts',(2.25591330654054,2.36332902778761,3.10059247973866));
#21364=CARTESIAN_POINT('Ctrl Pts',(2.58768383946716,2.63520721631527,3.12461965782392));
#21365=CARTESIAN_POINT('Ctrl Pts',(2.77601333675428,2.75911543555872,3.13699129080868));
#21366=CARTESIAN_POINT('Ctrl Pts',(3.00556458882084,2.87786837283464,3.15239621387373));
#21367=CARTESIAN_POINT('Ctrl Pts',(3.03569649450793,2.89286281596386,3.15442502550917));
#21368=CARTESIAN_POINT('Ctrl Pts',(3.07699414819286,2.91261281342183,3.15722210540213));
#21369=CARTESIAN_POINT('Ctrl Pts',(3.08796121636261,2.91778181248422,3.15796646208979));
#21370=CARTESIAN_POINT('Ctrl Pts',(3.10636662391309,2.92633005578013,3.15921870661804));
#21371=CARTESIAN_POINT('Ctrl Pts',(3.11378924493475,2.92974317911138,3.15972453864958));
#21372=CARTESIAN_POINT('Ctrl Pts',(3.12789273947022,2.93616349634336,3.16068735636654));
#21373=CARTESIAN_POINT('Ctrl Pts',(3.13457104003222,2.93917620084513,3.16114398704493));
#21374=CARTESIAN_POINT('Ctrl Pts',(3.15041365336089,2.94625817960258,3.16222882229064));
#21375=CARTESIAN_POINT('Ctrl Pts',(3.15958673718835,2.9503074791374,3.16285821347111));
#21376=CARTESIAN_POINT('Ctrl Pts',(3.19179359653387,2.96434541650362,3.16507202929224));
#21377=CARTESIAN_POINT('Ctrl Pts',(3.21492439685828,2.97410735143469,3.16666914156387));
#21378=CARTESIAN_POINT('Ctrl Pts',(3.44253734122585,3.06704935497796,3.18243839807141));
#21379=CARTESIAN_POINT('Ctrl Pts',(3.65492585154512,3.12927533109989,3.19752811313324));
#21380=CARTESIAN_POINT('Ctrl Pts',(4.08526167123623,3.20863764561537,3.22706297232233));
#21381=CARTESIAN_POINT('Ctrl Pts',(4.30199468346828,3.22634769695101,3.24143203436631));
#21382=CARTESIAN_POINT('Ctrl Pts',(4.55051967751224,3.22153262063662,3.25709756475171));
#21383=CARTESIAN_POINT('Ctrl Pts',(4.58213255193061,3.22045443202462,3.25907642553904));
#21384=CARTESIAN_POINT('Ctrl Pts',(4.63051476704922,3.21809077363217,3.26208472293813));
#21385=CARTESIAN_POINT('Ctrl Pts',(4.64729774586694,3.21713918984079,3.26312451608655));
#21386=CARTESIAN_POINT('Ctrl Pts',(4.67784243585196,3.21516746145702,3.26501034560159));
#21387=CARTESIAN_POINT('Ctrl Pts',(4.69160641772356,3.21419016400823,3.26585770087099));
#21388=CARTESIAN_POINT('Ctrl Pts',(4.7216327846948,3.21186426423241,3.26770108859904));
#21389=CARTESIAN_POINT('Ctrl Pts',(4.73789212118772,3.21048048275839,3.26869599595685));
#21390=CARTESIAN_POINT('Ctrl Pts',(4.78252594564014,3.20634015158037,3.27141852242898));
#21391=CARTESIAN_POINT('Ctrl Pts',(4.8108758805816,3.20333047738715,3.2731381941255));
#21392=CARTESIAN_POINT('Ctrl Pts',(4.96990108317588,3.18431104664116,3.28273615631727));
#21393=CARTESIAN_POINT('Ctrl Pts',(5.09954693954922,3.16068125056175,3.29037017949853));
#21394=CARTESIAN_POINT('Ctrl Pts',(5.43989282343945,3.07683132161021,3.31030831079949));
#21395=CARTESIAN_POINT('Ctrl Pts',(5.64649245559286,3.00297368077317,3.32227930301988));
#21396=CARTESIAN_POINT('Ctrl Pts',(5.93858482303338,2.86363947522782,3.34075167973917));
#21397=CARTESIAN_POINT('Ctrl Pts',(6.03089675623035,2.81394225257676,3.34684896211601));
#21398=CARTESIAN_POINT('Ctrl Pts',(6.13540541484197,2.75092507306508,3.35424897618752));
#21399=CARTESIAN_POINT('Ctrl Pts',(6.15012424308198,2.74188769522744,3.35530313743748));
#21400=CARTESIAN_POINT('Ctrl Pts',(6.17264957455036,2.7278065414261,3.35693601543223));
#21401=CARTESIAN_POINT('Ctrl Pts',(6.18050834635878,2.72284641886572,3.35750941471188));
#21402=CARTESIAN_POINT('Ctrl Pts',(6.19494787879044,2.71364522602656,3.35857003413021));
#21403=CARTESIAN_POINT('Ctrl Pts',(6.20153473924759,2.7094141041535,3.35905660289348));
#21404=CARTESIAN_POINT('Ctrl Pts',(6.21644572519887,2.69975898413953,3.36016430369359));
#21405=CARTESIAN_POINT('Ctrl Pts',(6.22476017946508,2.69432049799191,3.36078637852781));
#21406=CARTESIAN_POINT('Ctrl Pts',(6.24630104692054,2.68008795771658,3.36240926138875));
#21407=CARTESIAN_POINT('Ctrl Pts',(6.25948765263792,2.67123453380736,3.36341381286248));
#21408=CARTESIAN_POINT('Ctrl Pts',(6.30864628809099,2.63769983166925,3.36719878950639));
#21409=CARTESIAN_POINT('Ctrl Pts',(6.34417595802215,2.6123901579048,3.37001549160216));
#21410=CARTESIAN_POINT('Ctrl Pts',(6.37917546296132,2.5863715564937,3.37286375486987));
#21411=CARTESIAN_POINT('Origin',(4.45646910621825,-5.13094777615093E-16,
-2.31077344927308));
#21412=CARTESIAN_POINT('Ctrl Pts',(6.37917539807422,-2.58637160473072,1.24811343365893));
#21413=CARTESIAN_POINT('Ctrl Pts',(6.28432437072099,-2.65688377194887,1.25590601120793));
#21414=CARTESIAN_POINT('Ctrl Pts',(6.1856529462747,-2.72213483260349,1.26353878577593));
#21415=CARTESIAN_POINT('Ctrl Pts',(6.05922589129334,-2.79608400843386,1.27274709778538));
#21416=CARTESIAN_POINT('Ctrl Pts',(6.03466209627653,-2.81002171913176,1.27451103026261));
#21417=CARTESIAN_POINT('Ctrl Pts',(5.99567005221813,-2.8314735465297,1.27727240294704));
#21418=CARTESIAN_POINT('Ctrl Pts',(5.98136315220221,-2.83920414216325,1.27827753174099));
#21419=CARTESIAN_POINT('Ctrl Pts',(5.95468376549879,-2.85336025318346,1.28013717763507));
#21420=CARTESIAN_POINT('Ctrl Pts',(5.94232697522004,-2.85981438252857,1.2809926923703));
#21421=CARTESIAN_POINT('Ctrl Pts',(5.91485444263773,-2.87393755215874,1.28288212726527));
#21422=CARTESIAN_POINT('Ctrl Pts',(5.8997192276691,-2.88156796678734,1.28391467402853));
#21423=CARTESIAN_POINT('Ctrl Pts',(5.8555827449706,-2.90338437910215,1.28690199436515));
#21424=CARTESIAN_POINT('Ctrl Pts',(5.82642712111742,-2.91725469886676,1.28884580596293));
#21425=CARTESIAN_POINT('Ctrl Pts',(5.60776806123106,-3.01727702066677,1.30321652298663));
#21426=CARTESIAN_POINT('Ctrl Pts',(5.41051693879766,-3.08532944758594,1.31498741028267));
#21427=CARTESIAN_POINT('Ctrl Pts',(4.98481503975404,-3.18742399352355,1.33949496928203));
#21428=CARTESIAN_POINT('Ctrl Pts',(4.75652322532088,-3.21694859947992,1.35214588414229));
#21429=CARTESIAN_POINT('Ctrl Pts',(4.5023938504328,-3.22251730446222,1.36742821714461));
#21430=CARTESIAN_POINT('Ctrl Pts',(4.47771127978986,-3.22277451051547,1.36892536824358));
#21431=CARTESIAN_POINT('Ctrl Pts',(4.44336140790039,-3.22273784447202,1.37102976860697));
#21432=CARTESIAN_POINT('Ctrl Pts',(4.43369400327641,-3.22268402345997,1.37162433012077));
#21433=CARTESIAN_POINT('Ctrl Pts',(4.41606430057242,-3.2225065441803,1.37271301854345));
#21434=CARTESIAN_POINT('Ctrl Pts',(4.40810185569787,-3.22239686929489,1.37320637464648));
#21435=CARTESIAN_POINT('Ctrl Pts',(4.39165632370578,-3.22210938039964,1.37422889590243));
#21436=CARTESIAN_POINT('Ctrl Pts',(4.38317345330773,-3.22192757512915,1.37475826711537));
#21437=CARTESIAN_POINT('Ctrl Pts',(4.36112298766194,-3.22136786222245,1.37613918599357));
#21438=CARTESIAN_POINT('Ctrl Pts',(4.34755704958475,-3.22093774151957,1.37699354788008));
#21439=CARTESIAN_POINT('Ctrl Pts',(4.28835265631089,-3.21868616273685,1.3807418800653));
#21440=CARTESIAN_POINT('Ctrl Pts',(4.24275549244713,-3.2159803717525,1.38367987015236));
#21441=CARTESIAN_POINT('Ctrl Pts',(4.11634734579705,-3.20577915928023,1.3919393466081));
#21442=CARTESIAN_POINT('Ctrl Pts',(4.03574100624826,-3.19619915040328,1.39733604843425));
#21443=CARTESIAN_POINT('Ctrl Pts',(3.68842590158269,-3.14155525492517,1.42093825935699));
#21444=CARTESIAN_POINT('Ctrl Pts',(3.42756459874292,-3.06604909057105,1.43944520159311));
#21445=CARTESIAN_POINT('Ctrl Pts',(3.1114303943461,-2.92957947643918,1.46171457712721));
#21446=CARTESIAN_POINT('Ctrl Pts',(3.04468845325288,-2.89800653130501,1.46641550554881));
#21447=CARTESIAN_POINT('Ctrl Pts',(2.95767602809721,-2.8531241066922,1.47254683047114));
#21448=CARTESIAN_POINT('Ctrl Pts',(2.93639104685182,-2.84184105876041,1.47404696787047));
#21449=CARTESIAN_POINT('Ctrl Pts',(2.9018980398178,-2.82305808483701,1.4764789722661));
#21450=CARTESIAN_POINT('Ctrl Pts',(2.88861329237939,-2.81570174387441,1.47741588535205));
#21451=CARTESIAN_POINT('Ctrl Pts',(2.86307016917397,-2.80132057840447,1.47921798870632));
#21452=CARTESIAN_POINT('Ctrl Pts',(2.85080504454862,-2.79430851672815,1.48008360895036));
#21453=CARTESIAN_POINT('Ctrl Pts',(2.82236678084909,-2.77780108432146,1.48209157391351));
#21454=CARTESIAN_POINT('Ctrl Pts',(2.80622952311672,-2.76824468124391,1.48323168395863));
#21455=CARTESIAN_POINT('Ctrl Pts',(2.75449431872098,-2.73699418156885,1.4868898721696));
#21456=CARTESIAN_POINT('Ctrl Pts',(2.71923270367704,-2.7147495738661,1.48938786126209));
#21457=CARTESIAN_POINT('Ctrl Pts',(2.63714099610603,-2.66070773288696,1.49522257662628));
#21458=CARTESIAN_POINT('Ctrl Pts',(2.5906967986849,-2.6283482705324,1.49853871474661));
#21459=CARTESIAN_POINT('Ctrl Pts',(2.4186052335584,-2.50158386836181,1.51092696304993));
#21460=CARTESIAN_POINT('Ctrl Pts',(2.29906332063943,-2.39925321046001,1.51973031771063));
#21461=CARTESIAN_POINT('Ctrl Pts',(2.04042594866894,-2.14283048916025,1.54009510912807));
#21462=CARTESIAN_POINT('Ctrl Pts',(1.9078016113455,-1.98324427361955,1.5515932836182));
#21463=CARTESIAN_POINT('Ctrl Pts',(1.77688408952507,-1.79070084398704,1.56556645303265));
#21464=CARTESIAN_POINT('Ctrl Pts',(1.76261183642913,-1.76915750819852,1.56713150115008));
#21465=CARTESIAN_POINT('Ctrl Pts',(1.74309700717423,-1.73891703159205,1.56933404914046));
#21466=CARTESIAN_POINT('Ctrl Pts',(1.73763371297858,-1.73036258879075,1.56995773193926));
#21467=CARTESIAN_POINT('Ctrl Pts',(1.72828032993332,-1.71556337469762,1.57103803908136));
#21468=CARTESIAN_POINT('Ctrl Pts',(1.72437100834903,-1.70933076749649,1.57149340956568));
#21469=CARTESIAN_POINT('Ctrl Pts',(1.71618499225832,-1.69618002829124,1.57245520842259));
#21470=CARTESIAN_POINT('Ctrl Pts',(1.71191310956421,-1.68925903581498,1.57296195566111));
#21471=CARTESIAN_POINT('Ctrl Pts',(1.70142952859197,-1.67212956678769,1.57421741888454));
#21472=CARTESIAN_POINT('Ctrl Pts',(1.6952483656057,-1.66190263658152,1.57496807754542));
#21473=CARTESIAN_POINT('Ctrl Pts',(1.67250840076782,-1.62380156383968,1.57776808880217));
#21474=CARTESIAN_POINT('Ctrl Pts',(1.65631425900738,-1.5957134366868,1.5798389368044));
#21475=CARTESIAN_POINT('Ctrl Pts',(1.54086116826912,-1.38829379280759,1.59515339350298));
#21476=CARTESIAN_POINT('Ctrl Pts',(1.45849505369408,-1.20011230603677,1.60913454978702));
#21477=CARTESIAN_POINT('Ctrl Pts',(1.32983823276182,-0.808292809777138,
1.63698809362539));
#21478=CARTESIAN_POINT('Ctrl Pts',(1.28429097750638,-0.605367708302494,
1.65078410453559));
#21479=CARTESIAN_POINT('Ctrl Pts',(1.25338928457226,-0.357971930268893,
1.66660968803264));
#21480=CARTESIAN_POINT('Ctrl Pts',(1.24901623065826,-0.316402530620074,
1.66923765898355));
#21481=CARTESIAN_POINT('Ctrl Pts',(1.24386977488883,-0.256257453817599,
1.67299666990883));
#21482=CARTESIAN_POINT('Ctrl Pts',(1.2424466104044,-0.237743066846545,1.6741479090382));
#21483=CARTESIAN_POINT('Ctrl Pts',(1.24022116562331,-0.205102179782672,
1.6761674520122));
#21484=CARTESIAN_POINT('Ctrl Pts',(1.23935175919098,-0.190980902539523,
1.67703783514015));
#21485=CARTESIAN_POINT('Ctrl Pts',(1.23774534006146,-0.161751815801462,
1.67883271301947));
#21486=CARTESIAN_POINT('Ctrl Pts',(1.23702163822925,-0.146643601406856,
1.67975677029862));
#21487=CARTESIAN_POINT('Ctrl Pts',(1.23543211109036,-0.107729625951668,
1.68212764455932));
#21488=CARTESIAN_POINT('Ctrl Pts',(1.23472380317287,-0.0839180861933661,
1.68356951875863));
#21489=CARTESIAN_POINT('Ctrl Pts',(1.23280957768231,0.0187101694074913,
1.68974821475011));
#21490=CARTESIAN_POINT('Ctrl Pts',(1.23423139400789,0.0975522380866514,
1.69440300411715));
#21491=CARTESIAN_POINT('Ctrl Pts',(1.24609610761348,0.314153016811112,1.70701475805742));
#21492=CARTESIAN_POINT('Ctrl Pts',(1.26250392090779,0.451417090806418,1.71480483617002));
#21493=CARTESIAN_POINT('Ctrl Pts',(1.32749907840671,0.802153790944397,1.73478394794283));
#21494=CARTESIAN_POINT('Ctrl Pts',(1.38909113958491,1.01245919142645,1.74682213063857));
#21495=CARTESIAN_POINT('Ctrl Pts',(1.48550686650785,1.2493541908941,1.76201093224694));
#21496=CARTESIAN_POINT('Ctrl Pts',(1.50013121623719,1.28357646241496,1.76424789018086));
#21497=CARTESIAN_POINT('Ctrl Pts',(1.52066834507762,1.32942132463193,1.76731265456939));
#21498=CARTESIAN_POINT('Ctrl Pts',(1.52606444487834,1.34127390004303,1.76811123459308));
#21499=CARTESIAN_POINT('Ctrl Pts',(1.53469410466658,1.35992835107652,1.76937845264571));
#21500=CARTESIAN_POINT('Ctrl Pts',(1.53787999283507,1.36675230538042,1.76984421182392));
#21501=CARTESIAN_POINT('Ctrl Pts',(1.54449601274022,1.38079474873368,1.770807327498));
#21502=CARTESIAN_POINT('Ctrl Pts',(1.54792908803591,1.38801166868292,1.77130487766316));
#21503=CARTESIAN_POINT('Ctrl Pts',(1.55623926321043,1.40531489049167,1.77250387175784));
#21504=CARTESIAN_POINT('Ctrl Pts',(1.56114216227308,1.41538862600662,1.77320688391706));
#21505=CARTESIAN_POINT('Ctrl Pts',(1.5782640472204,1.45010684370797,1.77564644487831));
#21506=CARTESIAN_POINT('Ctrl Pts',(1.59074558636522,1.47461954760107,1.77739808538057));
#21507=CARTESIAN_POINT('Ctrl Pts',(1.62213579785259,1.53436335348133,1.78173393781648));
#21508=CARTESIAN_POINT('Ctrl Pts',(1.64138897824218,1.56940746230951,1.7843349973596));
#21509=CARTESIAN_POINT('Ctrl Pts',(1.72314204425424,1.71186558948067,1.79512159394847));
#21510=CARTESIAN_POINT('Ctrl Pts',(1.79117483671061,1.81597453069043,1.80350660991975));
#21511=CARTESIAN_POINT('Ctrl Pts',(2.01853885950442,2.12350641620846,1.82937568827534));
#21512=CARTESIAN_POINT('Ctrl Pts',(2.19645937059511,2.31196625724159,1.84674473255027));
#21513=CARTESIAN_POINT('Ctrl Pts',(2.42237089471476,2.49996606705262,1.8653725266059));
#21514=CARTESIAN_POINT('Ctrl Pts',(2.45012183508567,2.52229194606669,1.86761161614946));
#21515=CARTESIAN_POINT('Ctrl Pts',(2.49236499678626,2.55513851678946,1.87094821459012));
#21516=CARTESIAN_POINT('Ctrl Pts',(2.50658339846922,2.56600536634488,1.87205936320115));
#21517=CARTESIAN_POINT('Ctrl Pts',(2.53140058791155,2.58464726991907,1.8739785236849));
#21518=CARTESIAN_POINT('Ctrl Pts',(2.54195767965379,2.59247686890071,1.87478866039092));
#21519=CARTESIAN_POINT('Ctrl Pts',(2.56405965146715,2.60866001418015,1.87647187775748));
#21520=CARTESIAN_POINT('Ctrl Pts',(2.57561265110091,2.61700202895191,1.87734449960534));
#21521=CARTESIAN_POINT('Ctrl Pts',(2.60310246705791,2.63657538604247,1.87940407685979));
#21522=CARTESIAN_POINT('Ctrl Pts',(2.61908673514986,2.64773935910417,1.88058843540739));
#21523=CARTESIAN_POINT('Ctrl Pts',(2.67310743913949,2.6847445250957,1.88454800274269));
#21524=CARTESIAN_POINT('Ctrl Pts',(2.71159643474556,2.70991728285408,1.88729808959648));
#21525=CARTESIAN_POINT('Ctrl Pts',(2.80520640138743,2.76831891875407,1.89382997636857));
#21526=CARTESIAN_POINT('Ctrl Pts',(2.86081035045357,2.80073776514723,1.89758356995579));
#21527=CARTESIAN_POINT('Ctrl Pts',(3.08415071533901,2.92214013477198,1.91223931768102));
#21528=CARTESIAN_POINT('Ctrl Pts',(3.25863645153879,2.99789282083081,1.92275256765801));
#21529=CARTESIAN_POINT('Ctrl Pts',(3.51886224504409,3.08449900862795,1.93812820688402));
#21530=CARTESIAN_POINT('Ctrl Pts',(3.59995567257934,3.10799362183085,1.94288397493816));
#21531=CARTESIAN_POINT('Ctrl Pts',(3.76870892624601,3.14977873825397,1.95286919072498));
#21532=CARTESIAN_POINT('Ctrl Pts',(3.85639348047208,3.1676531372025,1.95810566431655));
#21533=CARTESIAN_POINT('Ctrl Pts',(3.96024328092333,3.18435635069918,1.96448215351545));
#21534=CARTESIAN_POINT('Ctrl Pts',(3.97580531962413,3.18674249657521,1.9654422595561));
#21535=CARTESIAN_POINT('Ctrl Pts',(4.00117414241517,3.19044228074222,1.96701576185162));
#21536=CARTESIAN_POINT('Ctrl Pts',(4.01097079832151,3.19182497991703,1.96762542596179));
#21537=CARTESIAN_POINT('Ctrl Pts',(4.02852864087191,3.19422068466063,1.96872195905145));
#21538=CARTESIAN_POINT('Ctrl Pts',(4.03628732985413,3.19525055304027,1.96920787546485));
#21539=CARTESIAN_POINT('Ctrl Pts',(4.05330045459496,3.19744579311992,1.97027642563613));
#21540=CARTESIAN_POINT('Ctrl Pts',(4.06255609662174,3.19859923987284,1.97085969354372));
#21541=CARTESIAN_POINT('Ctrl Pts',(4.08912396716185,3.20179308973439,1.9725392590116));
#21542=CARTESIAN_POINT('Ctrl Pts',(4.1064476083125,3.20373319116,1.97364090088938));
#21543=CARTESIAN_POINT('Ctrl Pts',(4.2326786308378,3.21683396852926,1.9817111221626));
#21544=CARTESIAN_POINT('Ctrl Pts',(4.34206581741018,3.22257812747055,1.98893501374306));
#21545=CARTESIAN_POINT('Ctrl Pts',(4.69087246143503,3.22311373764159,2.01229276444122));
#21546=CARTESIAN_POINT('Ctrl Pts',(4.92955310009338,3.19681388845523,2.02869410108571));
#21547=CARTESIAN_POINT('Ctrl Pts',(5.26923103824124,3.12047486257552,2.05156072694335));
#21548=CARTESIAN_POINT('Ctrl Pts',(5.37407343638804,3.0912702945058,2.05856257610921));
#21549=CARTESIAN_POINT('Ctrl Pts',(5.50295735169327,3.04823138210278,2.06709721422406));
#21550=CARTESIAN_POINT('Ctrl Pts',(5.5285573998072,3.0393221233745,2.0687889785881));
#21551=CARTESIAN_POINT('Ctrl Pts',(5.56908507983875,3.02464199885521,2.07146235020954));
#21552=CARTESIAN_POINT('Ctrl Pts',(5.58408693988634,3.01908124467358,2.07245086438306));
#21553=CARTESIAN_POINT('Ctrl Pts',(5.61209378344675,3.00846204204178,2.07429451435462));
#21554=CARTESIAN_POINT('Ctrl Pts',(5.62510847361357,3.00343042065004,2.07515052011989));
#21555=CARTESIAN_POINT('Ctrl Pts',(5.65383655843253,2.99210882193038,2.07703859973636));
#21556=CARTESIAN_POINT('Ctrl Pts',(5.66953397654492,2.98577923753363,2.07806931719305));
#21557=CARTESIAN_POINT('Ctrl Pts',(5.71528035578434,2.96691285013587,2.08107082056864));
#21558=CARTESIAN_POINT('Ctrl Pts',(5.74519061721309,2.95404377183853,2.08303037529159));
#21559=CARTESIAN_POINT('Ctrl Pts',(5.81296490668127,2.92365810985191,2.08746740799169));
#21560=CARTESIAN_POINT('Ctrl Pts',(5.85069447942567,2.90585502620798,2.08993515888191));
#21561=CARTESIAN_POINT('Ctrl Pts',(5.97498579920238,2.84422860181653,2.09807036397128));
#21562=CARTESIAN_POINT('Ctrl Pts',(6.05991623655735,2.79722874427635,2.10363704431509));
#21563=CARTESIAN_POINT('Ctrl Pts',(6.22383374807,2.69659516588618,2.1145353227027));
#21564=CARTESIAN_POINT('Ctrl Pts',(6.30276803677694,2.64317303334387,2.11986096441958));
#21565=CARTESIAN_POINT('Ctrl Pts',(6.37918119522423,2.5863672951246,2.12518466390817));
#21566=CARTESIAN_POINT('Ctrl Pts',(5.88688308661327,2.88166464694226,-0.413294290592403));
#21567=CARTESIAN_POINT('Ctrl Pts',(6.84537358445575,2.40588471549031,-0.347122251455184));
#21568=CARTESIAN_POINT('Ctrl Pts',(8.23365752427788,0.430873938343679,-0.214778173180747));
#21569=CARTESIAN_POINT('Ctrl Pts',(6.86376121760315,-2.94715670275194,-0.0162620557690901));
#21570=CARTESIAN_POINT('Ctrl Pts',(3.28608690294124,-3.61718018023642,0.182254061642566));
#21571=CARTESIAN_POINT('Ctrl Pts',(0.781880406995935,-0.979166244321737,
0.380770179054222));
#21572=CARTESIAN_POINT('Ctrl Pts',(1.64193314359211,2.55787552455616,0.579286296465875));
#21573=CARTESIAN_POINT('Ctrl Pts',(5.07993189931123,3.75125370222575,0.777802413877532));
#21574=CARTESIAN_POINT('Ctrl Pts',(7.94674205925474,1.50993542852403,0.976318531289188));
#21575=CARTESIAN_POINT('Ctrl Pts',(7.61734820438694,-2.11448150974993,1.17483464870084));
#21576=CARTESIAN_POINT('Ctrl Pts',(4.39321803491158,-3.80232526959411,1.3733507661125));
#21577=CARTESIAN_POINT('Ctrl Pts',(1.22704502026327,-2.0081611280352,1.57186688352415));
#21578=CARTESIAN_POINT('Ctrl Pts',(1.01829993859556,1.62508529687376,1.77038300093581));
#21579=CARTESIAN_POINT('Ctrl Pts',(3.95817375267475,3.77008527062174,1.96889911834747));
#21580=CARTESIAN_POINT('Ctrl Pts',(7.35437229592725,2.462525507432,2.16741523575912));
#21581=CARTESIAN_POINT('Ctrl Pts',(8.09672865983581,-1.10017486129741,2.36593135317078));
#21582=CARTESIAN_POINT('Ctrl Pts',(5.50540329893836,-3.65535258567839,2.56444747058243));
#21583=CARTESIAN_POINT('Ctrl Pts',(1.95348461951634,-2.8630297341532,2.76296358799409));
#21584=CARTESIAN_POINT('Ctrl Pts',(0.693751175975549,0.551202220257554,
2.96147970540574));
#21585=CARTESIAN_POINT('Ctrl Pts',(2.87984341841113,3.46065318004877,3.1599958228174));
#21586=CARTESIAN_POINT('Ctrl Pts',(6.50977938134639,3.20090403962421,3.35851194022905));
#21587=CARTESIAN_POINT('Ctrl Pts',(8.25933290131072,0.00982773524565914,
3.55702805764071));
#21588=CARTESIAN_POINT('Ctrl Pts',(6.52629607038668,-3.19024855326339,3.75554417505237));
#21589=CARTESIAN_POINT('Ctrl Pts',(2.89775109124319,-3.46875593755042,3.95406029246402));
#21590=CARTESIAN_POINT('Ctrl Pts',(0.69665041333009,-0.570642598253718,
4.15257640987568));
#21591=CARTESIAN_POINT('Ctrl Pts',(1.93872017863753,2.85005436799852,4.35109252728733));
#21592=CARTESIAN_POINT('Ctrl Pts',(5.48649651727959,3.66072576290342,4.54960864469899));
#21593=CARTESIAN_POINT('Ctrl Pts',(8.09099334705098,1.11897413587954,4.74812476211065));
#21594=CARTESIAN_POINT('Ctrl Pts',(7.36706201253862,-2.44751271825679,4.9466408795223));
#21595=CARTESIAN_POINT('Ctrl Pts',(3.97766506003213,-3.7726139823619,5.14515699693396));
#21596=CARTESIAN_POINT('Ctrl Pts',(1.02674774506536,-1.64282712377203,5.34367311434561));
#21597=CARTESIAN_POINT('Ctrl Pts',(1.21670401249677,1.99142956468722,5.54218923175727));
#21598=CARTESIAN_POINT('Ctrl Pts',(4.37357552585394,3.80197293891488,5.74070534916892));
#21599=CARTESIAN_POINT('Ctrl Pts',(7.60635940332531,2.13074181682499,5.93922146658058));
#21600=CARTESIAN_POINT('Ctrl Pts',(7.95453366396254,-1.49178213007847,6.13773758399224));
#21601=CARTESIAN_POINT('Ctrl Pts',(5.09924694286633,-3.74816037897555,6.33625370140389));
#21602=CARTESIAN_POINT('Ctrl Pts',(1.65531650589596,-2.57204465036969,6.53476981881556));
#21603=CARTESIAN_POINT('Ctrl Pts',(0.776628336729841,0.959500643563771,
6.7332859362272));
#21604=CARTESIAN_POINT('Ctrl Pts',(3.26786834626679,3.6123534997611,6.93180205363886));
#21605=CARTESIAN_POINT('Ctrl Pts',(6.84760632218384,2.95708173512582,7.1303181710505));
#21606=CARTESIAN_POINT('Ctrl Pts',(8.23758631997216,-0.406229232878139,
7.32883428846218));
#21607=CARTESIAN_POINT('Ctrl Pts',(6.16489109788061,-3.39752319671194,7.52735040587382));
#21608=CARTESIAN_POINT('Ctrl Pts',(2.52765551345678,-3.27743004474078,7.72586652328549));
#21609=CARTESIAN_POINT('Ctrl Pts',(0.656790727359,-0.155928801126063,7.92438264069713));
#21610=CARTESIAN_POINT('Ctrl Pts',(2.26559912307384,3.10836907247963,8.1228987581088));
#21611=CARTESIAN_POINT('Ctrl Pts',(5.88076457458627,3.52608167695778,8.32141487552045));
#21612=CARTESIAN_POINT('Ctrl Pts',(8.19158732913988,0.714675754863574,8.5199309929321));
#21613=CARTESIAN_POINT('Ctrl Pts',(7.08185986462416,-2.75121662896035,8.71844711034376));
#21614=CARTESIAN_POINT('Ctrl Pts',(3.56784948378791,-3.69759715767183,8.91696322775543));
#21615=CARTESIAN_POINT('Ctrl Pts',(0.867620049835816,-1.2577885451434,9.11547934516706));
#21616=CARTESIAN_POINT('Ctrl Pts',(1.45399031457103,2.33387889135228,9.31399546257875));
#21617=CARTESIAN_POINT('Ctrl Pts',(4.78997354349419,3.78822443423146,9.51251157999037));
#21618=CARTESIAN_POINT('Ctrl Pts',(7.8205397526871,1.77338609991104,9.71102769740205));
#21619=CARTESIAN_POINT('Ctrl Pts',(7.77035405525285,-1.8654854913274,9.90954381481369));
#21620=CARTESIAN_POINT('Ctrl Pts',(4.68537555826851,-3.79598095490491,10.1080599322253));
#21621=CARTESIAN_POINT('Ctrl Pts',(1.39076888675897,-2.25018926719472,10.306576049637));
#21622=CARTESIAN_POINT('Ctrl Pts',(0.903672160428571,1.35628294827392,10.5050921670486));
#21623=CARTESIAN_POINT('Ctrl Pts',(3.67015929568852,3.72069703895061,10.7036082844603));
#21624=CARTESIAN_POINT('Ctrl Pts',(7.156733998233,2.67776755651859,10.902124401872));
#21625=CARTESIAN_POINT('Ctrl Pts',(8.17045747715504,-0.817410517633158,
11.1006405192836));
#21626=CARTESIAN_POINT('Ctrl Pts',(5.78298105352307,-3.56401958853324,11.2991566366953));
#21627=CARTESIAN_POINT('Ctrl Pts',(2.18071022148213,-3.04676731509573,11.4976727541069));
#21628=CARTESIAN_POINT('Ctrl Pts',(0.662536086558379,0.260656509846819,
11.6961888715186));
#21629=CARTESIAN_POINT('Ctrl Pts',(2.61877364278075,3.32937606128419,11.8947049889302));
#21630=CARTESIAN_POINT('Ctrl Pts',(6.25793774774488,3.34911634724554,12.0932211063419));
#21631=CARTESIAN_POINT('Ctrl Pts',(8.24735113836601,0.301799589347462,12.2917372237535));
#21632=CARTESIAN_POINT('Ctrl Pts',(6.76514687416864,-3.02189949163811,12.4902533411652));
#21633=CARTESIAN_POINT('Ctrl Pts',(3.16869942579002,-3.57820050080496,12.6887694585768));
#21634=CARTESIAN_POINT('Ctrl Pts',(0.751566954770839,-0.857653555925328,
12.8872855759885));
#21635=CARTESIAN_POINT('Ctrl Pts',(1.72731339933552,2.64831620117018,13.0858016934002));
#21636=CARTESIAN_POINT('Ctrl Pts',(5.20236872621718,3.72900835754984,13.2843178108118));
#21637=CARTESIAN_POINT('Ctrl Pts',(7.99434336961907,1.39474559334568,13.4828339282235));
#21638=CARTESIAN_POINT('Ctrl Pts',(7.54640006010282,-2.21679865437008,13.6813500456351));
#21639=CARTESIAN_POINT('Ctrl Pts',(4.26875675973819,-3.79824086239538,13.8798661630468));
#21640=CARTESIAN_POINT('Ctrl Pts',(1.16301685561255,-1.9013263388412,14.0783822804584));
#21641=CARTESIAN_POINT('Ctrl Pts',(1.07335787448695,1.73678667876183,14.2768983978701));
#21642=CARTESIAN_POINT('Ctrl Pts',(4.08188780578152,3.78438349314049,14.4754145152818));
#21643=CARTESIAN_POINT('Ctrl Pts',(7.43345216672421,2.36631389110821,14.6739306326934));
#21644=CARTESIAN_POINT('Ctrl Pts',(8.05875206907788,-1.21878096033793,14.8724467501051));
#21645=CARTESIAN_POINT('Ctrl Pts',(5.38514975673243,-3.68773939197872,15.0709628675167));
#21646=CARTESIAN_POINT('Ctrl Pts',(1.86107937002522,-2.77953623668677,15.2694789849284));
#21647=CARTESIAN_POINT('Ctrl Pts',(0.713817534175901,0.674113331777405,
15.46799510234));
#21648=CARTESIAN_POINT('Ctrl Pts',(2.9940048152212,3.5104227339951,15.6665112197517));
#21649=CARTESIAN_POINT('Ctrl Pts',(6.61348907494099,3.13195377174095,15.8650273371633));
#21650=CARTESIAN_POINT('Ctrl Pts',(8.257615478175,-0.114698878595687,16.063543454575));
#21651=CARTESIAN_POINT('Ctrl Pts',(6.42072433944188,-3.25631247771842,16.2620595719866));
#21652=CARTESIAN_POINT('Ctrl Pts',(2.78500562221897,-3.41585705137789,16.4605756893983));
#21653=CARTESIAN_POINT('Ctrl Pts',(0.67998136903583,-0.447224713876356,
16.65909180681));
#21654=CARTESIAN_POINT('Ctrl Pts',(2.03339274915041,2.93096750947701,16.8576079242216));
#21655=CARTESIAN_POINT('Ctrl Pts',(5.60581136526813,3.62503544056518,17.0561240416333));
#21656=CARTESIAN_POINT('Ctrl Pts',(8.12568420335589,0.999364870669326,17.2546401590449));
#21657=CARTESIAN_POINT('Ctrl Pts',(7.28535965135699,-2.54150503784963,17.4531562764566));
#21658=CARTESIAN_POINT('Ctrl Pts',(3.85439094932391,-3.75491297725849,17.6516723938682));
#21659=CARTESIAN_POINT('Ctrl Pts',(0.974793970633971,-1.52964303811135,
17.8501885112799));
#21660=CARTESIAN_POINT('Ctrl Pts',(1.2836488526281,2.09644489844015,18.0487046286916));
#21661=CARTESIAN_POINT('Ctrl Pts',(4.49811216942012,3.80264847561477,18.2472207461032));
#21662=CARTESIAN_POINT('Ctrl Pts',(7.67443956106538,2.02645891285741,18.4457368635149));
#21663=CARTESIAN_POINT('Ctrl Pts',(7.90381082245328,-1.60552317494378,18.6442529809265));
#21664=CARTESIAN_POINT('Ctrl Pts',(4.9761721155001,-3.76719767944954,18.8427690983382));
#21665=CARTESIAN_POINT('Ctrl Pts',(1.57259927845708,-2.47894420875808,19.0412852157498));
#21666=CARTESIAN_POINT('Ctrl Pts',(0.810019572635768,1.07947921368855,19.2398013331615));
#21667=CARTESIAN_POINT('Ctrl Pts',(3.38678898688482,3.6493361063157,19.4383174505731));
#21668=CARTESIAN_POINT('Ctrl Pts',(6.94315110686829,2.87720041011993,19.6368335679848));
#21669=CARTESIAN_POINT('Ctrl Pts',(8.22225715251285,-0.529820690755693,
19.8353496853965));
#21670=CARTESIAN_POINT('Ctrl Pts',(6.05272613795891,-3.45164208273989,20.0338658028081));
#21671=CARTESIAN_POINT('Ctrl Pts',(2.42137329831411,-3.212515309774,20.2323819202198));
#21672=CARTESIAN_POINT('Ctrl Pts',(0.65372248686789,-0.0314281299545405,
20.4308980376314));
#21673=CARTESIAN_POINT('Ctrl Pts',(2.36855469553213,3.178440343651,20.6294141550431));
#21674=CARTESIAN_POINT('Ctrl Pts',(5.99545920128352,3.47755359131801,20.8279302724548));
#21675=CARTESIAN_POINT('Ctrl Pts',(8.21298586010566,0.591989447683331,21.0264463898664));
#21676=CARTESIAN_POINT('Ctrl Pts',(6.99036591797756,-2.83570744333498,21.2249625072781));
#21677=CARTESIAN_POINT('Ctrl Pts',(3.44725150283742,-3.6665172604341,21.4234786246897));
#21678=CARTESIAN_POINT('Ctrl Pts',(0.828359319011244,-1.13960058009792,
21.6219947421014));
#21679=CARTESIAN_POINT('Ctrl Pts',(1.53202116508044,2.43094114262164,21.820510859513));
#21680=CARTESIAN_POINT('Ctrl Pts',(4.91383661347899,3.77527223251319,22.0190269769247));
#21681=CARTESIAN_POINT('Ctrl Pts',(7.87680396956558,1.66228269728872,22.2175430943363));
#21682=CARTESIAN_POINT('Ctrl Pts',(7.7074930081086,-1.97299730385434,22.416059211748));
#21683=CARTESIAN_POINT('Ctrl Pts',(4.56095756308617,-3.80143701374933,22.6145753291597));
#21684=CARTESIAN_POINT('Ctrl Pts',(1.31873095853907,-2.14860623751896,22.8130914465713));
#21685=CARTESIAN_POINT('Ctrl Pts',(0.949990286798536,1.47190262315773,23.011607563983));
#21686=CARTESIAN_POINT('Ctrl Pts',(3.7924065803434,3.74442240079083,23.2101236813946));
#21687=CARTESIAN_POINT('Ctrl Pts',(7.24297719250067,2.58796472414074,23.4086397988063));
#21688=CARTESIAN_POINT('Ctrl Pts',(8.14168123233833,-0.938680920498277,
23.6071559162179));
#21689=CARTESIAN_POINT('Ctrl Pts',(5.66560616055497,-3.60535681683013,23.8056720336296));
#21690=CARTESIAN_POINT('Ctrl Pts',(2.08209581503262,-2.97097481614092,24.0041881510412));
#21691=CARTESIAN_POINT('Ctrl Pts',(0.673241827254791,0.385434817028999,
24.2027042684529));
#21692=CARTESIAN_POINT('Ctrl Pts',(2.72851506381635,3.38643791990783,24.4012203858645));
#21693=CARTESIAN_POINT('Ctrl Pts',(6.36713580394013,3.29091791303403,24.5997365032762));
#21694=CARTESIAN_POINT('Ctrl Pts',(8.25465969525897,0.17151120336101,24.7982954766299));
#21695=CARTESIAN_POINT('Ctrl Pts',(7.19525837483205,-1.99900958588141,24.9306824108463));
#21696=CARTESIAN_POINT('Ctrl Pts',(6.32311239899223,-2.62025147071356,24.9968973059255));
#21697=CARTESIAN_POINT('Ctrl Pts',(5.99341579333084,3.0962819108244,-0.27495920519366));
#21698=CARTESIAN_POINT('Ctrl Pts',(7.02329163031133,2.58506739568259,-0.208787166056442));
#21699=CARTESIAN_POINT('Ctrl Pts',(8.51497056474962,0.462964065771816,-0.0764430877820045));
#21700=CARTESIAN_POINT('Ctrl Pts',(7.04304871618797,-3.16665160770128,0.122073029629653));
#21701=CARTESIAN_POINT('Ctrl Pts',(3.19892054011338,-3.88657631350085,0.320589147041309));
#21702=CARTESIAN_POINT('Ctrl Pts',(0.508208668906595,-1.05209144762919,
0.519105264452963));
#21703=CARTESIAN_POINT('Ctrl Pts',(1.43231541168923,2.74837799923302,0.717621381864618));
#21704=CARTESIAN_POINT('Ctrl Pts',(5.12636543519397,4.03063520713254,0.916137499276276));
#21705=CARTESIAN_POINT('Ctrl Pts',(8.20668654383497,1.62239064105283,1.11465361668793));
#21706=CARTESIAN_POINT('Ctrl Pts',(7.85276047702285,-2.27196140132349,1.31316973409959));
#21707=CARTESIAN_POINT('Ctrl Pts',(4.38850729527858,-4.08551042322263,1.51168585151124));
#21708=CARTESIAN_POINT('Ctrl Pts',(0.986527733847538,-2.15772261402933,
1.7102019689229));
#21709=CARTESIAN_POINT('Ctrl Pts',(0.7622359790706,1.74611650720567,1.90871808633455));
#21710=CARTESIAN_POINT('Ctrl Pts',(3.92106229159746,4.0508692911502,2.10723420374621));
#21711=CARTESIAN_POINT('Ctrl Pts',(7.57019895508782,2.64592661456843,2.30575032115786));
#21712=CARTESIAN_POINT('Ctrl Pts',(8.36784367179503,-1.18211240346562,2.50426643856952));
#21713=CARTESIAN_POINT('Ctrl Pts',(5.58352459826198,-3.92759167890361,2.70278255598118));
#21714=CARTESIAN_POINT('Ctrl Pts',(1.7670702556363,-3.07625912870098,2.90129867339283));
#21715=CARTESIAN_POINT('Ctrl Pts',(0.413515851644582,0.592254017343965,
3.09981479080449));
#21716=CARTESIAN_POINT('Ctrl Pts',(2.76242132641212,3.7183916776686,3.29833090821614));
#21717=CARTESIAN_POINT('Ctrl Pts',(6.66270343294158,3.43929724324088,3.4968470256278));
#21718=CARTESIAN_POINT('Ctrl Pts',(8.54255816261418,0.0105596738669375,
3.69536314303945));
#21719=CARTESIAN_POINT('Ctrl Pts',(6.6804502327146,-3.42784816997514,3.89387926045112));
#21720=CARTESIAN_POINT('Ctrl Pts',(2.78166270604797,-3.72709790290783,4.09239537786277));
#21721=CARTESIAN_POINT('Ctrl Pts',(0.416631015022661,-0.613142253174304,
4.29091149527442));
#21722=CARTESIAN_POINT('Ctrl Pts',(1.75120620592284,3.06231739833558,4.48942761268608));
#21723=CARTESIAN_POINT('Ctrl Pts',(5.56320969933569,3.93336503336498,4.68794373009773));
#21724=CARTESIAN_POINT('Ctrl Pts',(8.36168121106336,1.20231178852842,4.88645984750939));
#21725=CARTESIAN_POINT('Ctrl Pts',(7.58383376163584,-2.62979572036334,5.08497596492104));
#21726=CARTESIAN_POINT('Ctrl Pts',(3.94200524984668,-4.05358633333867,5.2834920823327));
#21727=CARTESIAN_POINT('Ctrl Pts',(0.771312951433223,-1.76517968922739,
5.48200819974436));
#21728=CARTESIAN_POINT('Ctrl Pts',(0.97541656054666,2.13974493679014,5.68052431715601));
#21729=CARTESIAN_POINT('Ctrl Pts',(4.36740187430494,4.08513185206935,5.87904043456767));
#21730=CARTESIAN_POINT('Ctrl Pts',(7.84095326483218,2.28943272461384,6.07755655197932));
#21731=CARTESIAN_POINT('Ctrl Pts',(8.21505844260491,-1.60288534238506,6.27607266939098));
#21732=CARTESIAN_POINT('Ctrl Pts',(5.14711900207072,-4.02731150295548,6.47458878680263));
#21733=CARTESIAN_POINT('Ctrl Pts',(1.44669552446588,-2.76360239669899,6.6731049042143));
#21734=CARTESIAN_POINT('Ctrl Pts',(0.502565441067234,1.03096121515846,6.87162102162594));
#21735=CARTESIAN_POINT('Ctrl Pts',(3.17934512299035,3.88139015713774,7.07013713903761));
#21736=CARTESIAN_POINT('Ctrl Pts',(7.0256906552799,3.17731582507866,7.26865325644925));
#21737=CARTESIAN_POINT('Ctrl Pts',(8.51919196471455,-0.436483900631263,
7.46716937386092));
#21738=CARTESIAN_POINT('Ctrl Pts',(6.2921289615216,-3.65055997294754,7.66568549127257));
#21739=CARTESIAN_POINT('Ctrl Pts',(2.38400358079477,-3.52152266305215,7.86420160868423));
#21740=CARTESIAN_POINT('Ctrl Pts',(0.373802705776339,-0.16754188479758,
8.06271772609589));
#21741=CARTESIAN_POINT('Ctrl Pts',(2.10243005973299,3.33987056457006,8.26123384350753));
#21742=CARTESIAN_POINT('Ctrl Pts',(5.98684159389007,3.78869308197905,8.4597499609192));
#21743=CARTESIAN_POINT('Ctrl Pts',(8.4697671146088,0.767902543495819,8.65826607833084));
#21744=CARTESIAN_POINT('Ctrl Pts',(7.27739066026635,-2.95611853726567,8.85678219574251));
#21745=CARTESIAN_POINT('Ctrl Pts',(3.50166790634439,-3.97298249293629,9.05529831315416));
#21746=CARTESIAN_POINT('Ctrl Pts',(0.600333929022254,-1.35146465571633,
9.25381443056581));
#21747=CARTESIAN_POINT('Ctrl Pts',(1.23037519550738,2.50769880562501,9.45233054797748));
#21748=CARTESIAN_POINT('Ctrl Pts',(4.81481189860833,4.07035940226423,9.65084666538912));
#21749=CARTESIAN_POINT('Ctrl Pts',(8.07108508884113,1.90546228475562,9.84936278280079));
#21750=CARTESIAN_POINT('Ctrl Pts',(8.01716171947454,-2.00442094739626,10.0478789002124));
#21751=CARTESIAN_POINT('Ctrl Pts',(4.70242378644322,-4.07869360405195,10.2463950176241));
#21752=CARTESIAN_POINT('Ctrl Pts',(1.16244523581599,-2.41777624309588,10.4449111350357));
#21753=CARTESIAN_POINT('Ctrl Pts',(0.639071086725107,1.45729461030662,10.6434272524474));
#21754=CARTESIAN_POINT('Ctrl Pts',(3.61159742927608,3.99780278027315,10.841943369859));
#21755=CARTESIAN_POINT('Ctrl Pts',(7.35784118240728,2.87719921033794,11.0404594872707));
#21756=CARTESIAN_POINT('Ctrl Pts',(8.44706357811351,-0.878288666292467,
11.2389756046823));
#21757=CARTESIAN_POINT('Ctrl Pts',(5.88177546561389,-3.82945648915419,11.437491722094));
#21758=CARTESIAN_POINT('Ctrl Pts',(2.01121890138154,-3.27368090323489,11.6360078395057));
#21759=CARTESIAN_POINT('Ctrl Pts',(0.379975961147697,0.280069381853164,
11.8345239569173));
#21760=CARTESIAN_POINT('Ctrl Pts',(2.4819079000476,3.57733745452462,12.033040074329));
#21761=CARTESIAN_POINT('Ctrl Pts',(6.39210543142176,3.59854793451629,12.2315561917406));
#21762=CARTESIAN_POINT('Ctrl Pts',(8.52968403588164,0.324276667717884,12.4300723091523));
#21763=CARTESIAN_POINT('Ctrl Pts',(6.93708988851933,-3.24696100298028,12.6285884265639));
#21764=CARTESIAN_POINT('Ctrl Pts',(3.07279041513639,-3.84469355089646,12.8271045439756));
#21765=CARTESIAN_POINT('Ctrl Pts',(0.475637566686629,-0.921528878727684,
13.0256206613872));
#21766=CARTESIAN_POINT('Ctrl Pts',(1.52405451869475,2.84555441124189,13.2241367787989));
#21767=CARTESIAN_POINT('Ctrl Pts',(5.25792096951678,4.00673309958052,13.4226528962106));
#21768=CARTESIAN_POINT('Ctrl Pts',(8.257833049161,1.4986218314684,13.6211690136222));
#21769=CARTESIAN_POINT('Ctrl Pts',(7.77652833946771,-2.38189880309254,13.8196851310339));
#21770=CARTESIAN_POINT('Ctrl Pts',(4.25477653818775,-4.08112182230083,14.0182012484455));
#21771=CARTESIAN_POINT('Ctrl Pts',(0.917730954110628,-2.04293110781465,
14.2167173658572));
#21772=CARTESIAN_POINT('Ctrl Pts',(0.821394455796449,1.86613705453794,14.4152334832688));
#21773=CARTESIAN_POINT('Ctrl Pts',(4.05399017588675,4.06623240003544,14.6137496006805));
#21774=CARTESIAN_POINT('Ctrl Pts',(7.65516844441363,2.54254946152231,14.8122657180922));
#21775=CARTESIAN_POINT('Ctrl Pts',(8.32703870473431,-1.30955190943392,15.0107818355038));
#21776=CARTESIAN_POINT('Ctrl Pts',(5.45431495277465,-3.96239055204922,15.2092979529155));
#21777=CARTESIAN_POINT('Ctrl Pts',(1.66778295557931,-2.98654729975826,15.4078140703271));
#21778=CARTESIAN_POINT('Ctrl Pts',(0.435076688703739,0.724319159497842,
15.6063301877388));
#21779=CARTESIAN_POINT('Ctrl Pts',(2.88508510279309,3.77186791049719,15.8048463051504));
#21780=CARTESIAN_POINT('Ctrl Pts',(6.77413709632598,3.36521177759866,16.0033624225621));
#21781=CARTESIAN_POINT('Ctrl Pts',(8.54071283123811,-0.123241288109086,
16.2018785399737));
#21782=CARTESIAN_POINT('Ctrl Pts',(6.56701585333057,-3.49883232646441,16.4003946573854));
#21783=CARTESIAN_POINT('Ctrl Pts',(2.66052031127365,-3.67025927509159,16.598910774797));
#21784=CARTESIAN_POINT('Ctrl Pts',(0.398720513058523,-0.480532595324168,
16.7974268922087));
#21785=CARTESIAN_POINT('Ctrl Pts',(1.85292968989636,3.14925669454191,16.9959430096203));
#21786=CARTESIAN_POINT('Ctrl Pts',(5.69141073963082,3.89501660876095,17.194459127032));
#21787=CARTESIAN_POINT('Ctrl Pts',(8.39895573256671,1.07379440374864,17.3929752444437));
#21788=CARTESIAN_POINT('Ctrl Pts',(7.49604646714037,-2.73078829048094,17.5914913618553));
#21789=CARTESIAN_POINT('Ctrl Pts',(3.80955007347359,-4.03456701338995,17.790007479267));
#21790=CARTESIAN_POINT('Ctrl Pts',(0.715489824289806,-1.64356601103751,
17.9885235966786));
#21791=CARTESIAN_POINT('Ctrl Pts',(1.04734724052415,2.25258148028018,18.1870397140903));
#21792=CARTESIAN_POINT('Ctrl Pts',(4.50121361298798,4.08585770060491,18.3855558315019));
#21793=CARTESIAN_POINT('Ctrl Pts',(7.91410381728119,2.1773831599618,18.5840719489136));
#21794=CARTESIAN_POINT('Ctrl Pts',(8.16055792437237,-1.72509746033864,18.7825880663253));
#21795=CARTESIAN_POINT('Ctrl Pts',(5.0148779510323,-4.04776664132528,18.9811041837369));
#21796=CARTESIAN_POINT('Ctrl Pts',(1.35781777968586,-2.66356812881232,19.1796203011486));
#21797=CARTESIAN_POINT('Ctrl Pts',(0.538443550556935,1.1598754095142,19.3781364185603));
#21798=CARTESIAN_POINT('Ctrl Pts',(3.30712259659747,3.92112711119714,19.5766525359719));
#21799=CARTESIAN_POINT('Ctrl Pts',(7.12835131317638,3.09148519177063,19.7751686533836));
#21800=CARTESIAN_POINT('Ctrl Pts',(8.50272112937199,-0.569280059186615,
19.9736847707952));
#21801=CARTESIAN_POINT('Ctrl Pts',(6.17161031033075,-3.70870946234774,20.1722008882069));
#21802=CARTESIAN_POINT('Ctrl Pts',(2.26980580259814,-3.45177328404759,20.3707170056185));
#21803=CARTESIAN_POINT('Ctrl Pts',(0.370505952442893,-0.0337687976193256,
20.5692331230302));
#21804=CARTESIAN_POINT('Ctrl Pts',(2.21305343742525,3.41516052227788,20.7677492404418));
#21805=CARTESIAN_POINT('Ctrl Pts',(6.11007831343283,3.73655077808788,20.9662653578534));
#21806=CARTESIAN_POINT('Ctrl Pts',(8.49275934044528,0.636078948397367,21.1647814752652));
#21807=CARTESIAN_POINT('Ctrl Pts',(7.17908253400595,-3.04690196012391,21.3632975926768));
#21808=CARTESIAN_POINT('Ctrl Pts',(3.37208816940477,-3.93958786330456,21.5618137100885));
#21809=CARTESIAN_POINT('Ctrl Pts',(0.558149183206385,-1.22447442503984,
21.7603298275001));
#21810=CARTESIAN_POINT('Ctrl Pts',(1.31421753683424,2.61198994621562,21.9588459449118));
#21811=CARTESIAN_POINT('Ctrl Pts',(4.94789989808116,4.05644256154919,22.1573620623234));
#21812=CARTESIAN_POINT('Ctrl Pts',(8.13153968654471,1.78608425229248,22.3558781797351));
#21813=CARTESIAN_POINT('Ctrl Pts',(7.94961898046267,-2.11993989949929,22.5543942971467));
#21814=CARTESIAN_POINT('Ctrl Pts',(4.56873953270021,-4.0845560128934,22.7529104145584));
#21815=CARTESIAN_POINT('Ctrl Pts',(1.08504215066615,-2.30862763082918,22.95142653197));
#21816=CARTESIAN_POINT('Ctrl Pts',(0.688838840573486,1.58152527269752,23.1499426493817));
#21817=CARTESIAN_POINT('Ctrl Pts',(3.74294930484078,4.02329513198439,23.3484587667933));
#21818=CARTESIAN_POINT('Ctrl Pts',(7.45050749686758,2.78070814718547,23.546974884205));
#21819=CARTESIAN_POINT('Ctrl Pts',(8.41614416964521,-1.00859090500303,23.7454910016166));
#21820=CARTESIAN_POINT('Ctrl Pts',(5.75565886205016,-3.87387238340306,23.9440071190283));
#21821=CARTESIAN_POINT('Ctrl Pts',(1.90526000600476,-3.19224361880315,24.14252323644));
#21822=CARTESIAN_POINT('Ctrl Pts',(0.391479031532891,0.414140782493564,
24.3410393538516));
#21823=CARTESIAN_POINT('Ctrl Pts',(2.59982251484541,3.6386490998064,24.5395554712633));
#21824=CARTESIAN_POINT('Ctrl Pts',(6.50943621328541,3.53601506509354,24.7380715886749));
#21825=CARTESIAN_POINT('Ctrl Pts',(8.53753691096405,0.184284815040506,24.9366305620286));
#21826=CARTESIAN_POINT('Ctrl Pts',(7.39923473266516,-2.14788949397592,25.069017496245));
#21827=CARTESIAN_POINT('Ctrl Pts',(6.46213408444902,-2.81539950847165,25.1352323913243));
#21828=CARTESIAN_POINT('Ctrl Pts',(6.0999485000484,3.31089917470656,-0.136624119794918));
#21829=CARTESIAN_POINT('Ctrl Pts',(7.2012096761669,2.76425007587486,-0.0704520806576993));
#21830=CARTESIAN_POINT('Ctrl Pts',(8.79628360522135,0.495054193199949,0.061891997616738));
#21831=CARTESIAN_POINT('Ctrl Pts',(7.22233621477278,-3.38614651265062,0.260408115028396));
#21832=CARTESIAN_POINT('Ctrl Pts',(3.11175417728552,-4.15597244676529,0.458924232440051));
#21833=CARTESIAN_POINT('Ctrl Pts',(0.234536930817258,-1.12501665093665,
0.657440349851707));
#21834=CARTESIAN_POINT('Ctrl Pts',(1.22269767978634,2.93888047390986,0.855956467263361));
#21835=CARTESIAN_POINT('Ctrl Pts',(5.17279897107673,4.31001671203934,1.05447258467502));
#21836=CARTESIAN_POINT('Ctrl Pts',(8.46663102841521,1.73484585358162,1.25298870208667));
#21837=CARTESIAN_POINT('Ctrl Pts',(8.08817274965877,-2.42944129289705,1.45150481949833));
#21838=CARTESIAN_POINT('Ctrl Pts',(4.38379655564558,-4.36869557685114,1.65002093690999));
#21839=CARTESIAN_POINT('Ctrl Pts',(0.746010447431816,-2.30728410002347,
1.84853705432164));
#21840=CARTESIAN_POINT('Ctrl Pts',(0.506172019545635,1.86714771753756,2.04705317173329));
#21841=CARTESIAN_POINT('Ctrl Pts',(3.88395083052018,4.33165331167866,2.24556928914495));
#21842=CARTESIAN_POINT('Ctrl Pts',(7.78602561424836,2.82932772170484,2.4440854065566));
#21843=CARTESIAN_POINT('Ctrl Pts',(8.63895868375428,-1.26404994563383,2.64260152396827));
#21844=CARTESIAN_POINT('Ctrl Pts',(5.66164589758561,-4.19983077212884,2.84111764137992));
#21845=CARTESIAN_POINT('Ctrl Pts',(1.58065589175627,-3.28948852324876,3.03963375879158));
#21846=CARTESIAN_POINT('Ctrl Pts',(0.133280527313607,0.633305814430374,
3.23814987620323));
#21847=CARTESIAN_POINT('Ctrl Pts',(2.6449992344131,3.97613017528841,3.43666599361489));
#21848=CARTESIAN_POINT('Ctrl Pts',(6.81562748453676,3.67769044685756,3.63518211102655));
#21849=CARTESIAN_POINT('Ctrl Pts',(8.82578342391765,0.0112916124882134,
3.8336982284382));
#21850=CARTESIAN_POINT('Ctrl Pts',(6.83460439504253,-3.66544778668689,4.03221434584986));
#21851=CARTESIAN_POINT('Ctrl Pts',(2.66557432085276,-3.98543986826524,4.23073046326151));
#21852=CARTESIAN_POINT('Ctrl Pts',(0.13661161671523,-0.655641908094887,
4.42924658067317));
#21853=CARTESIAN_POINT('Ctrl Pts',(1.56369223320815,3.27458042867263,4.62776269808482));
#21854=CARTESIAN_POINT('Ctrl Pts',(5.63992288139177,4.20600430382654,4.82627881549648));
#21855=CARTESIAN_POINT('Ctrl Pts',(8.63236907507575,1.28564944117731,5.02479493290813));
#21856=CARTESIAN_POINT('Ctrl Pts',(7.80060551073305,-2.81207872246989,5.22331105031979));
#21857=CARTESIAN_POINT('Ctrl Pts',(3.90634543966123,-4.33455868431544,5.42182716773146));
#21858=CARTESIAN_POINT('Ctrl Pts',(0.515878157801087,-1.88753225468275,
5.62034328514309));
#21859=CARTESIAN_POINT('Ctrl Pts',(0.734129108596551,2.28806030889307,5.81885940255477));
#21860=CARTESIAN_POINT('Ctrl Pts',(4.36122822275595,4.36829076522382,6.0173755199664));
#21861=CARTESIAN_POINT('Ctrl Pts',(8.07554712633902,2.44812363240269,6.21589163737808));
#21862=CARTESIAN_POINT('Ctrl Pts',(8.47558322124728,-1.71398855469165,6.41440775478972));
#21863=CARTESIAN_POINT('Ctrl Pts',(5.19499106127511,-4.3064626269354,6.61292387220138));
#21864=CARTESIAN_POINT('Ctrl Pts',(1.2380745430358,-2.9551601430283,6.81143998961304));
#21865=CARTESIAN_POINT('Ctrl Pts',(0.228502545404632,1.10242178675316,7.00995610702469));
#21866=CARTESIAN_POINT('Ctrl Pts',(3.09082189971391,4.15042681451437,7.20847222443635));
#21867=CARTESIAN_POINT('Ctrl Pts',(7.20377498837598,3.39754991503151,7.406988341848));
#21868=CARTESIAN_POINT('Ctrl Pts',(8.80079760945692,-0.466738568384383,
7.60550445925966));
#21869=CARTESIAN_POINT('Ctrl Pts',(6.41936682516261,-3.90359674918315,7.80402057667131));
#21870=CARTESIAN_POINT('Ctrl Pts',(2.24035164813274,-3.7656152813635,8.00253669408298));
#21871=CARTESIAN_POINT('Ctrl Pts',(0.0908146841936848,-0.179154968469096,
8.20105281149462));
#21872=CARTESIAN_POINT('Ctrl Pts',(1.93926099639212,3.57137205666049,8.39956892890629));
#21873=CARTESIAN_POINT('Ctrl Pts',(6.09291861319388,4.05130448700034,8.59808504631793));
#21874=CARTESIAN_POINT('Ctrl Pts',(8.7479469000777,0.821129332128062,8.7966011637296));
#21875=CARTESIAN_POINT('Ctrl Pts',(7.47292145590854,-3.16102044557099,8.99511728114126));
#21876=CARTESIAN_POINT('Ctrl Pts',(3.43548632890085,-4.24836782820074,9.19363339855291));
#21877=CARTESIAN_POINT('Ctrl Pts',(0.333047808208697,-1.44514076628925,
9.39214951596456));
#21878=CARTESIAN_POINT('Ctrl Pts',(1.00676007644372,2.68151871989772,9.59066563337622));
#21879=CARTESIAN_POINT('Ctrl Pts',(4.83965025372247,4.352494370297,9.78918175078787));
#21880=CARTESIAN_POINT('Ctrl Pts',(8.32163042499515,2.03753846960017,9.98769786819953));
#21881=CARTESIAN_POINT('Ctrl Pts',(8.26396938369623,-2.14335640346512,10.1862139856111));
#21882=CARTESIAN_POINT('Ctrl Pts',(4.71947201461794,-4.36140625319899,10.3847301030228));
#21883=CARTESIAN_POINT('Ctrl Pts',(0.934121584873003,-2.58536321899705,
10.5832462204345));
#21884=CARTESIAN_POINT('Ctrl Pts',(0.37447001302165,1.5583062723393,10.7817623378461));
#21885=CARTESIAN_POINT('Ctrl Pts',(3.55303556286365,4.27490852159572,10.9802784552578));
#21886=CARTESIAN_POINT('Ctrl Pts',(7.55894836658157,3.07663086415728,11.1787945726694));
#21887=CARTESIAN_POINT('Ctrl Pts',(8.72366967907197,-0.939166814951776,
11.3773106900811));
#21888=CARTESIAN_POINT('Ctrl Pts',(5.98056987770475,-4.09489338977514,11.5758268074927));
#21889=CARTESIAN_POINT('Ctrl Pts',(1.84172758128094,-3.50059449137405,11.7743429249044));
#21890=CARTESIAN_POINT('Ctrl Pts',(0.0974158357370281,0.299482253859507,
11.9728590423161));
#21891=CARTESIAN_POINT('Ctrl Pts',(2.34504215731444,3.82529884776504,12.1713751597277));
#21892=CARTESIAN_POINT('Ctrl Pts',(6.52627311509865,3.84797952178704,12.3698912771394));
#21893=CARTESIAN_POINT('Ctrl Pts',(8.81201693339725,0.346753746088307,12.568407394551));
#21894=CARTESIAN_POINT('Ctrl Pts',(7.10903290287004,-3.47202251432246,12.7669235119627));
#21895=CARTESIAN_POINT('Ctrl Pts',(2.97688140448274,-4.11118660098796,12.9654396293744));
#21896=CARTESIAN_POINT('Ctrl Pts',(0.199708178602426,-0.985404201530036,
13.163955746786));
#21897=CARTESIAN_POINT('Ctrl Pts',(1.32079563805398,3.0427926213136,13.3624718641977));
#21898=CARTESIAN_POINT('Ctrl Pts',(5.3134732128164,4.28445784161121,13.5609879816093));
#21899=CARTESIAN_POINT('Ctrl Pts',(8.52132272870291,1.60249806959112,13.759504099021));
#21900=CARTESIAN_POINT('Ctrl Pts',(8.00665661883263,-2.546998951815,13.9580202164326));
#21901=CARTESIAN_POINT('Ctrl Pts',(4.24079631663729,-4.36400278220629,14.1565363338443));
#21902=CARTESIAN_POINT('Ctrl Pts',(0.672445052608722,-2.18453587678811,
14.3550524512559));
#21903=CARTESIAN_POINT('Ctrl Pts',(0.569431037105937,1.99548743031406,14.5535685686676));
#21904=CARTESIAN_POINT('Ctrl Pts',(4.02609254599198,4.3480813069304,14.7520846860792));
#21905=CARTESIAN_POINT('Ctrl Pts',(7.87688472210303,2.7187850319364,14.9506008034909));
#21906=CARTESIAN_POINT('Ctrl Pts',(8.59532534039074,-1.40032285852991,15.1491169209026));
#21907=CARTESIAN_POINT('Ctrl Pts',(5.52348014881688,-4.2370417121197,15.3476330383142));
#21908=CARTESIAN_POINT('Ctrl Pts',(1.47448654113341,-3.19355836282975,15.5461491557259));
#21909=CARTESIAN_POINT('Ctrl Pts',(0.156335843231577,0.774524987218279,
15.7446652731375));
#21910=CARTESIAN_POINT('Ctrl Pts',(2.77616539036498,4.03331308699926,15.9431813905492));
#21911=CARTESIAN_POINT('Ctrl Pts',(6.93478511771097,3.59846978345639,16.1416975079608));
#21912=CARTESIAN_POINT('Ctrl Pts',(8.82381018430121,-0.131783697622486,
16.3402136253725));
#21913=CARTESIAN_POINT('Ctrl Pts',(6.71330736721926,-3.74135217521042,16.5387297427841));
#21914=CARTESIAN_POINT('Ctrl Pts',(2.53603500032833,-3.92466149880528,16.7372458601958));
#21915=CARTESIAN_POINT('Ctrl Pts',(0.117459657081213,-0.513840476771981,
16.9357619776075));
#21916=CARTESIAN_POINT('Ctrl Pts',(1.6724666306423,3.3675458796068,17.1342780950191));
#21917=CARTESIAN_POINT('Ctrl Pts',(5.77701011399349,4.16499777695671,17.3327942124308));
#21918=CARTESIAN_POINT('Ctrl Pts',(8.67222726177754,1.14822393682795,17.5313103298424));
#21919=CARTESIAN_POINT('Ctrl Pts',(7.70673328292373,-2.92007154311226,17.7298264472541));
#21920=CARTESIAN_POINT('Ctrl Pts',(3.76470919762329,-4.31422104952143,17.9283425646657));
#21921=CARTESIAN_POINT('Ctrl Pts',(0.456185677945633,-1.75748898396369,
18.1268586820774));
#21922=CARTESIAN_POINT('Ctrl Pts',(0.811045628420214,2.40871806212022,18.3253747994891));
#21923=CARTESIAN_POINT('Ctrl Pts',(4.50431505655582,4.36906692559506,18.5238909169007));
#21924=CARTESIAN_POINT('Ctrl Pts',(8.153768073497,2.32830740706619,18.7224070343124));
#21925=CARTESIAN_POINT('Ctrl Pts',(8.41730502629147,-1.84467174573349,18.920923151724));
#21926=CARTESIAN_POINT('Ctrl Pts',(5.05358378656449,-4.328335603201,19.1194392691357));
#21927=CARTESIAN_POINT('Ctrl Pts',(1.14303628091464,-2.84819204886657,19.3179553865473));
#21928=CARTESIAN_POINT('Ctrl Pts',(0.266867528478102,1.24027160533984,19.516471503959));
#21929=CARTESIAN_POINT('Ctrl Pts',(3.22745620631011,4.19291811607857,19.7149876213706));
#21930=CARTESIAN_POINT('Ctrl Pts',(7.31355151948446,3.30576997342133,19.9135037387823));
#21931=CARTESIAN_POINT('Ctrl Pts',(8.78318510623113,-0.60873942761753,20.112019856194));
#21932=CARTESIAN_POINT('Ctrl Pts',(6.29049448270258,-3.96577684195559,20.3105359736056));
#21933=CARTESIAN_POINT('Ctrl Pts',(2.11823830688215,-3.69103125832118,20.5090520910173));
#21934=CARTESIAN_POINT('Ctrl Pts',(0.0872894180178925,-0.0361094652841183,
20.7075682084289));
#21935=CARTESIAN_POINT('Ctrl Pts',(2.05755217931839,3.65188070090475,20.9060843258406));
#21936=CARTESIAN_POINT('Ctrl Pts',(6.2246974255821,3.99554796485774,21.1046004432522));
#21937=CARTESIAN_POINT('Ctrl Pts',(8.77253282078492,0.680168449111409,21.3031165606639));
#21938=CARTESIAN_POINT('Ctrl Pts',(7.36779915003431,-3.25809647691284,21.5016326780756));
#21939=CARTESIAN_POINT('Ctrl Pts',(3.29692483597213,-4.21265846617502,21.7001487954872));
#21940=CARTESIAN_POINT('Ctrl Pts',(0.287939047401517,-1.30934826998177,
21.8986649128989));
#21941=CARTESIAN_POINT('Ctrl Pts',(1.09641390858805,2.79303874980958,22.0971810303105));
#21942=CARTESIAN_POINT('Ctrl Pts',(4.98196318268333,4.33761289058522,22.2956971477222));
#21943=CARTESIAN_POINT('Ctrl Pts',(8.38627540352384,1.90988580729624,22.4942132651338));
#21944=CARTESIAN_POINT('Ctrl Pts',(8.19174495281671,-2.26688249514424,22.6927293825455));
#21945=CARTESIAN_POINT('Ctrl Pts',(4.57652150231426,-4.36767501203749,22.8912454999571));
#21946=CARTESIAN_POINT('Ctrl Pts',(0.851353342793238,-2.46864902413938,
23.0897616173688));
#21947=CARTESIAN_POINT('Ctrl Pts',(0.42768739434844,1.69114792223732,23.2882777347804));
#21948=CARTESIAN_POINT('Ctrl Pts',(3.69349202933814,4.30216786317793,23.4867938521921));
#21949=CARTESIAN_POINT('Ctrl Pts',(7.65803780123451,2.9734515702302,23.6853099696038));
#21950=CARTESIAN_POINT('Ctrl Pts',(8.6906071069521,-1.07850088950778,23.8838260870154));
#21951=CARTESIAN_POINT('Ctrl Pts',(5.84571156354535,-4.14238794997599,24.0823422044271));
#21952=CARTESIAN_POINT('Ctrl Pts',(1.7284241969769,-3.41351242146536,24.2808583218387));
#21953=CARTESIAN_POINT('Ctrl Pts',(0.109716235810993,0.442846747958131,
24.4793744392504));
#21954=CARTESIAN_POINT('Ctrl Pts',(2.47112996587446,3.89086027970496,24.677890556662));
#21955=CARTESIAN_POINT('Ctrl Pts',(6.6517366226307,3.78111221715306,24.8764066740737));
#21956=CARTESIAN_POINT('Ctrl Pts',(8.82041412666913,0.197058426719993,25.0749656474274));
#21957=CARTESIAN_POINT('Ctrl Pts',(7.60321109049825,-2.29676940207044,25.2073525816438));
#21958=CARTESIAN_POINT('Ctrl Pts',(6.60115576990582,-3.01054754622974,25.273567476723));
#21959=CARTESIAN_POINT('Ctrl Pts',(6.20648120676596,3.5255164385887,0.00171096560382468));
#21960=CARTESIAN_POINT('Ctrl Pts',(7.37912772202248,2.94343275606714,0.0678830047410433));
#21961=CARTESIAN_POINT('Ctrl Pts',(9.07759664569311,0.527144320628084,0.200227083015481));
#21962=CARTESIAN_POINT('Ctrl Pts',(7.40162371335757,-3.60564141759996,0.398743200427137));
#21963=CARTESIAN_POINT('Ctrl Pts',(3.02458781445768,-4.42536858002973,0.597259317838794));
#21964=CARTESIAN_POINT('Ctrl Pts',(-0.0391348072720899,-1.19794185424409,
0.795775435250448));
#21965=CARTESIAN_POINT('Ctrl Pts',(1.01307994788347,3.12938294858669,0.994291552662105));
#21966=CARTESIAN_POINT('Ctrl Pts',(5.21923250695947,4.58939821694615,1.19280767007376));
#21967=CARTESIAN_POINT('Ctrl Pts',(8.72657551299543,1.84730106611042,1.39132378748542));
#21968=CARTESIAN_POINT('Ctrl Pts',(8.32358502229467,-2.58692118447061,1.58983990489707));
#21969=CARTESIAN_POINT('Ctrl Pts',(4.37908581601258,-4.65188073047965,1.78835602230873));
#21970=CARTESIAN_POINT('Ctrl Pts',(0.505493161016087,-2.45684558601761,
1.98687213972038));
#21971=CARTESIAN_POINT('Ctrl Pts',(0.250108060020668,1.98817892786946,2.18538825713204));
#21972=CARTESIAN_POINT('Ctrl Pts',(3.8468393694429,4.61243733220712,2.38390437454369));
#21973=CARTESIAN_POINT('Ctrl Pts',(8.0018522734089,3.01272882884126,2.58242049195535));
#21974=CARTESIAN_POINT('Ctrl Pts',(8.91007369571349,-1.34598748780205,2.78093660936701));
#21975=CARTESIAN_POINT('Ctrl Pts',(5.73976719690925,-4.47206986535408,2.97945272677866));
#21976=CARTESIAN_POINT('Ctrl Pts',(1.39424152787623,-3.50271791779653,3.17796884419032));
#21977=CARTESIAN_POINT('Ctrl Pts',(-0.146954797017362,0.674357611516781,
3.37648496160198));
#21978=CARTESIAN_POINT('Ctrl Pts',(2.5275771424141,4.23386867290823,3.57500107901363));
#21979=CARTESIAN_POINT('Ctrl Pts',(6.96855153613195,3.91608365047424,3.77351719642529));
#21980=CARTESIAN_POINT('Ctrl Pts',(9.10900868522111,0.0120235511094912,
3.97203331383693));
#21981=CARTESIAN_POINT('Ctrl Pts',(6.98875855737045,-3.90304740339865,4.17054943124861));
#21982=CARTESIAN_POINT('Ctrl Pts',(2.54948593565754,-4.24378183362265,4.36906554866025));
#21983=CARTESIAN_POINT('Ctrl Pts',(-0.143407781592193,-0.698141563015474,
4.56758166607191));
#21984=CARTESIAN_POINT('Ctrl Pts',(1.37617826049345,3.48684345900968,4.76609778348356));
#21985=CARTESIAN_POINT('Ctrl Pts',(5.71663606344787,4.47864357428809,4.96461390089523));
#21986=CARTESIAN_POINT('Ctrl Pts',(8.90305693908813,1.36898709382619,5.16313001830687));
#21987=CARTESIAN_POINT('Ctrl Pts',(8.01737725983028,-2.99436172457643,5.36164613571854));
#21988=CARTESIAN_POINT('Ctrl Pts',(3.87068562947579,-4.61553103529222,5.56016225313019));
#21989=CARTESIAN_POINT('Ctrl Pts',(0.260443364168955,-2.00988482013811,
5.75867837054185));
#21990=CARTESIAN_POINT('Ctrl Pts',(0.492841656646439,2.436375680996,5.95719448795349));
#21991=CARTESIAN_POINT('Ctrl Pts',(4.35505457120696,4.6514496783783,6.15571060536516));
#21992=CARTESIAN_POINT('Ctrl Pts',(8.31014098784587,2.60681454019155,6.35422672277681));
#21993=CARTESIAN_POINT('Ctrl Pts',(8.73610799988966,-1.82509176699825,6.55274284018847));
#21994=CARTESIAN_POINT('Ctrl Pts',(5.24286312047947,-4.58561375091533,6.75125895760012));
#21995=CARTESIAN_POINT('Ctrl Pts',(1.02945356160573,-3.14671788935761,6.94977507501179));
#21996=CARTESIAN_POINT('Ctrl Pts',(-0.0455603502579819,1.17388235834786,
7.14829119242343));
#21997=CARTESIAN_POINT('Ctrl Pts',(3.00229867643747,4.41946347189101,7.34680730983509));
#21998=CARTESIAN_POINT('Ctrl Pts',(7.38185932147204,3.61778400498435,7.54532342724674));
#21999=CARTESIAN_POINT('Ctrl Pts',(9.08240325419932,-0.496993236137507,
7.7438395446584));
#22000=CARTESIAN_POINT('Ctrl Pts',(6.5466046888036,-4.15663352541875,7.94235566207006));
#22001=CARTESIAN_POINT('Ctrl Pts',(2.09669971547073,-4.00970789967487,8.1408717794817));
#22002=CARTESIAN_POINT('Ctrl Pts',(-0.192173337388976,-0.19076805214061,
8.33938789689338));
#22003=CARTESIAN_POINT('Ctrl Pts',(1.77609193305126,3.80287354875093,8.53790401430502));
#22004=CARTESIAN_POINT('Ctrl Pts',(6.1989956324977,4.3139158920216,8.73642013171668));
#22005=CARTESIAN_POINT('Ctrl Pts',(9.0261266855466,0.874356120760312,8.93493624912834));
#22006=CARTESIAN_POINT('Ctrl Pts',(7.66845225155073,-3.36592235387631,9.13345236653999));
#22007=CARTESIAN_POINT('Ctrl Pts',(3.36930475145732,-4.52375316346519,9.33196848395166));
#22008=CARTESIAN_POINT('Ctrl Pts',(0.0657616873951493,-1.53881687686219,
9.53048460136329));
#22009=CARTESIAN_POINT('Ctrl Pts',(0.783144957380055,2.85533863417045,9.72900071877498));
#22010=CARTESIAN_POINT('Ctrl Pts',(4.86448860883662,4.63462933832978,9.92751683618659));
#22011=CARTESIAN_POINT('Ctrl Pts',(8.57217576114917,2.16961465444475,10.1260329535983));
#22012=CARTESIAN_POINT('Ctrl Pts',(8.51077704791793,-2.28229185953398,10.3245490710099));
#22013=CARTESIAN_POINT('Ctrl Pts',(4.73652024279266,-4.644118902346,10.5230651884216));
#22014=CARTESIAN_POINT('Ctrl Pts',(0.705797933930029,-2.75295019489822,
10.7215813058332));
#22015=CARTESIAN_POINT('Ctrl Pts',(0.109868939318185,1.65931793437198,10.9200974232449));
#22016=CARTESIAN_POINT('Ctrl Pts',(3.49447369645122,4.55201426291826,11.1186135406565));
#22017=CARTESIAN_POINT('Ctrl Pts',(7.76005555075585,3.27606251797663,11.3171296580682));
#22018=CARTESIAN_POINT('Ctrl Pts',(9.00027578003045,-1.00004496361109,11.5156457754798));
#22019=CARTESIAN_POINT('Ctrl Pts',(6.07936428979557,-4.36033029039609,11.7141618928915));
#22020=CARTESIAN_POINT('Ctrl Pts',(1.67223626118035,-3.72750807951321,11.9126780103032));
#22021=CARTESIAN_POINT('Ctrl Pts',(-0.185144289673645,0.31889512586586,
12.1111941277148));
#22022=CARTESIAN_POINT('Ctrl Pts',(2.20817641458127,4.07326024100545,12.3097102451265));
#22023=CARTESIAN_POINT('Ctrl Pts',(6.66044079877556,4.09741110905781,12.5082263625381));
#22024=CARTESIAN_POINT('Ctrl Pts',(9.09434983091284,0.369230824458725,12.7067424799498));
#22025=CARTESIAN_POINT('Ctrl Pts',(7.28097591722075,-3.69708402566464,12.9052585973614));
#22026=CARTESIAN_POINT('Ctrl Pts',(2.8809723938291,-4.37767965107946,13.1037747147731));
#22027=CARTESIAN_POINT('Ctrl Pts',(-0.0762212094817758,-1.04927952433239,
13.3022908321848));
#22028=CARTESIAN_POINT('Ctrl Pts',(1.11753675741321,3.24003083138531,13.5008069495964));
#22029=CARTESIAN_POINT('Ctrl Pts',(5.369025456116,4.5621825836419,13.6993230670081));
#22030=CARTESIAN_POINT('Ctrl Pts',(8.78481240824481,1.70637430771384,13.8978391844197));
#22031=CARTESIAN_POINT('Ctrl Pts',(8.23678489819753,-2.71209910053747,14.0963553018314));
#22032=CARTESIAN_POINT('Ctrl Pts',(4.22681609508684,-4.64688374211174,14.294871419243));
#22033=CARTESIAN_POINT('Ctrl Pts',(0.427159151106815,-2.32614064576156,
14.4933875366547));
#22034=CARTESIAN_POINT('Ctrl Pts',(0.317467618415429,2.12483780609018,14.6919036540663));
#22035=CARTESIAN_POINT('Ctrl Pts',(3.99819491609722,4.62993021382537,14.890419771478));
#22036=CARTESIAN_POINT('Ctrl Pts',(8.09860099979244,2.8950206023505,15.0889358888896));
#22037=CARTESIAN_POINT('Ctrl Pts',(8.86361197604717,-1.49109380762589,15.2874520063013));
#22038=CARTESIAN_POINT('Ctrl Pts',(5.59264534485911,-4.5116928721902,15.485968123713));
#22039=CARTESIAN_POINT('Ctrl Pts',(1.2811901266875,-3.40056942590122,15.6844842411246));
#22040=CARTESIAN_POINT('Ctrl Pts',(-0.122405002240585,0.824730814938715,
15.8830003585363));
#22041=CARTESIAN_POINT('Ctrl Pts',(2.66724567793686,4.29475826350135,16.0815164759479));
#22042=CARTESIAN_POINT('Ctrl Pts',(7.09543313909595,3.83172778931411,16.2800325933596));
#22043=CARTESIAN_POINT('Ctrl Pts',(9.10690753736432,-0.140326107135887,
16.4785487107712));
#22044=CARTESIAN_POINT('Ctrl Pts',(6.85959888110794,-3.98387202395643,16.6770648281829));
#22045=CARTESIAN_POINT('Ctrl Pts',(2.41154968938301,-4.179063722519,16.8755809455945));
#22046=CARTESIAN_POINT('Ctrl Pts',(-0.163801198896094,-0.547148358219792,
17.0740970630062));
#22047=CARTESIAN_POINT('Ctrl Pts',(1.49200357138825,3.5858350646717,17.2726131804178));
#22048=CARTESIAN_POINT('Ctrl Pts',(5.86260948835618,4.43497894515246,17.4711292978295));
#22049=CARTESIAN_POINT('Ctrl Pts',(8.94549879098837,1.22265346990726,17.6696454152412));
#22050=CARTESIAN_POINT('Ctrl Pts',(7.91742009870712,-3.10935479574357,17.8681615326528));
#22051=CARTESIAN_POINT('Ctrl Pts',(3.71986832177296,-4.59387508565289,18.0666776500645));
#22052=CARTESIAN_POINT('Ctrl Pts',(0.196881531601468,-1.87141195688986,
18.2651937674761));
#22053=CARTESIAN_POINT('Ctrl Pts',(0.574744016316265,2.56485464396025,18.4637098848878));
#22054=CARTESIAN_POINT('Ctrl Pts',(4.50741650012369,4.6522761505852,18.6622260022994));
#22055=CARTESIAN_POINT('Ctrl Pts',(8.3934323297128,2.47923165417059,18.8607421197111));
#22056=CARTESIAN_POINT('Ctrl Pts',(8.67405212821057,-1.96424603112833,19.0592582371228));
#22057=CARTESIAN_POINT('Ctrl Pts',(5.09228962209667,-4.60890456507674,19.2577743545344));
#22058=CARTESIAN_POINT('Ctrl Pts',(0.928254782143413,-3.0328159689208,19.4562904719461));
#22059=CARTESIAN_POINT('Ctrl Pts',(-0.00470849360073685,1.32066780116548,
19.6548065893577));
#22060=CARTESIAN_POINT('Ctrl Pts',(3.14778981602278,4.46470912096001,19.8533227067694));
#22061=CARTESIAN_POINT('Ctrl Pts',(7.49875172579254,3.52005475507203,20.051838824181));
#22062=CARTESIAN_POINT('Ctrl Pts',(9.06364908309027,-0.648198796048447,
20.2503549415927));
#22063=CARTESIAN_POINT('Ctrl Pts',(6.4093786550744,-4.22284422156345,20.4488710590044));
#22064=CARTESIAN_POINT('Ctrl Pts',(1.96667081116617,-3.93028923259476,20.647387176416));
#22065=CARTESIAN_POINT('Ctrl Pts',(-0.195927116407106,-0.0384501329489085,
20.8459032938277));
#22066=CARTESIAN_POINT('Ctrl Pts',(1.90205092121151,3.88860087953163,21.0444194112393));
#22067=CARTESIAN_POINT('Ctrl Pts',(6.3393165377314,4.25454515162759,21.242935528651));
#22068=CARTESIAN_POINT('Ctrl Pts',(9.05230630112455,0.724257949825445,21.4414516460626));
#22069=CARTESIAN_POINT('Ctrl Pts',(7.55651576606266,-3.46929099370176,21.6399677634743));
#22070=CARTESIAN_POINT('Ctrl Pts',(3.22176150253947,-4.48572906904549,21.838483880886));
#22071=CARTESIAN_POINT('Ctrl Pts',(0.0177289115966501,-1.39422211492368,
22.0369999982976));
#22072=CARTESIAN_POINT('Ctrl Pts',(0.878610280341868,2.97408755340353,22.2355161157093));
#22073=CARTESIAN_POINT('Ctrl Pts',(5.01602646728549,4.61878321962123,22.4340322331209));
#22074=CARTESIAN_POINT('Ctrl Pts',(8.64101112050298,2.03368736229999,22.6325483505326));
#22075=CARTESIAN_POINT('Ctrl Pts',(8.43387092517075,-2.41382509078919,22.8310644679442));
#22076=CARTESIAN_POINT('Ctrl Pts',(4.58430347192829,-4.65079401118156,23.0295805853559));
#22077=CARTESIAN_POINT('Ctrl Pts',(0.617664534920323,-2.6286704174496,23.2280967027675));
#22078=CARTESIAN_POINT('Ctrl Pts',(0.166535948123391,1.80077057177711,23.4266128201792));
#22079=CARTESIAN_POINT('Ctrl Pts',(3.64403475383551,4.58104059437149,23.6251289375908));
#22080=CARTESIAN_POINT('Ctrl Pts',(7.86556810560143,3.16619499327494,23.8236450550025));
#22081=CARTESIAN_POINT('Ctrl Pts',(8.96507004425898,-1.14841087401253,24.0221611724142));
#22082=CARTESIAN_POINT('Ctrl Pts',(5.93576426504054,-4.41090351654891,24.2206772898258));
#22083=CARTESIAN_POINT('Ctrl Pts',(1.55158838794904,-3.63478122412758,24.4191934072375));
#22084=CARTESIAN_POINT('Ctrl Pts',(-0.172046559910909,0.471552713422697,
24.6177095246491));
#22085=CARTESIAN_POINT('Ctrl Pts',(2.34243741690352,4.14307145960353,24.8162256420608));
#22086=CARTESIAN_POINT('Ctrl Pts',(6.79403703197597,4.02620936921257,25.0147417594724));
#22087=CARTESIAN_POINT('Ctrl Pts',(9.10329134237422,0.209832038399488,25.2133007328261));
#22088=CARTESIAN_POINT('Ctrl Pts',(7.80718744833136,-2.44564931016495,25.3456876670425));
#22089=CARTESIAN_POINT('Ctrl Pts',(6.7401774553626,-3.20569558398784,25.4119025621217));
#22090=CARTESIAN_POINT('Ctrl Pts',(6.20927333103823,3.52819356681411,25.));
#22091=CARTESIAN_POINT('Ctrl Pts',(6.28261154412738,3.4838260879241,25.0000000000001));
#22092=CARTESIAN_POINT('Ctrl Pts',(6.35424941973236,3.43697508500066,25.0000000000001));
#22093=CARTESIAN_POINT('Ctrl Pts',(6.42404893624125,3.38764089866559,25.0000000000001));
#22094=CARTESIAN_POINT('Ctrl Pts',(6.52206241532727,3.3183651288261,25.));
#22095=CARTESIAN_POINT('Ctrl Pts',(6.61645276431289,3.24419440233525,25.));
#22096=CARTESIAN_POINT('Ctrl Pts',(6.70706507635195,3.16554216285713,25.));
#22097=CARTESIAN_POINT('Ctrl Pts',(6.80025007628785,3.08465680891572,25.));
#22098=CARTESIAN_POINT('Ctrl Pts',(6.88944003016716,2.99903106588321,25.));
#22099=CARTESIAN_POINT('Ctrl Pts',(6.97442221394972,2.90907978105801,25.));
#22100=CARTESIAN_POINT('Ctrl Pts',(7.05940439773228,2.81912849623282,25.));
#22101=CARTESIAN_POINT('Ctrl Pts',(7.14017919450627,2.72485071100732,25.));
#22102=CARTESIAN_POINT('Ctrl Pts',(7.21648332556474,2.62664039331786,25.));
#22103=CARTESIAN_POINT('Ctrl Pts',(7.2390189568644,2.59763499769156,25.));
#22104=CARTESIAN_POINT('Ctrl Pts',(7.26116427578476,2.56828649887293,25.));
#22105=CARTESIAN_POINT('Ctrl Pts',(7.28291158066946,2.53860488576137,25.));
#22106=CARTESIAN_POINT('Ctrl Pts',(7.29537914461769,2.52158864344917,25.));
#22107=CARTESIAN_POINT('Ctrl Pts',(7.30771776574352,2.50446012174108,25.));
#22108=CARTESIAN_POINT('Ctrl Pts',(7.31991133794954,2.48724223290588,25.));
#22109=CARTESIAN_POINT('Ctrl Pts',(7.3892179063549,2.38937814761646,25.));
#22110=CARTESIAN_POINT('Ctrl Pts',(7.45393979874638,2.28849903006182,25.));
#22111=CARTESIAN_POINT('Ctrl Pts',(7.51391284145599,2.18499970732938,25.));
#22112=CARTESIAN_POINT('Ctrl Pts',(7.57376716649844,2.08170526328231,25.));
#22113=CARTESIAN_POINT('Ctrl Pts',(7.6288917223817,1.97580008382021,25.));
#22114=CARTESIAN_POINT('Ctrl Pts',(7.67907542985071,1.86765710889506,25.));
#22115=CARTESIAN_POINT('Ctrl Pts',(7.72818555256263,1.76182764676762,25.));
#22116=CARTESIAN_POINT('Ctrl Pts',(7.77256407814287,1.65385429361903,25.));
#22117=CARTESIAN_POINT('Ctrl Pts',(7.81196451615951,1.5440804949319,25.));
#22118=CARTESIAN_POINT('Ctrl Pts',(7.84315387284692,1.45718363960404,25.));
#22119=CARTESIAN_POINT('Ctrl Pts',(7.87122292435585,1.36915832449176,25.));
#22120=CARTESIAN_POINT('Ctrl Pts',(7.89602624090641,1.28017705305137,25.));
#22121=CARTESIAN_POINT('Ctrl Pts',(7.90166022982024,1.25996526017227,25.));
#22122=CARTESIAN_POINT('Ctrl Pts',(7.90712563430273,1.2397041612825,25.));
#22123=CARTESIAN_POINT('Ctrl Pts',(7.91242059476302,1.21939581318014,25.));
#22124=CARTESIAN_POINT('Ctrl Pts',(7.91644877919605,1.2039460714304,25.));
#22125=CARTESIAN_POINT('Ctrl Pts',(7.92037774257214,1.18847099664305,25.));
#22126=CARTESIAN_POINT('Ctrl Pts',(7.92420415205769,1.1729825292745,25.));
#22127=CARTESIAN_POINT('Ctrl Pts',(7.95174043373912,1.06152169323888,25.));
#22128=CARTESIAN_POINT('Ctrl Pts',(7.97401184054752,0.949208236392413,25.));
#22129=CARTESIAN_POINT('Ctrl Pts',(7.99082766139777,0.836380380640087,25.));
#22130=CARTESIAN_POINT('Ctrl Pts',(8.00740128583895,0.725177572023492,25.));
#22131=CARTESIAN_POINT('Ctrl Pts',(8.01867545985289,0.613474332036543,25.));
#22132=CARTESIAN_POINT('Ctrl Pts',(8.02441717531606,0.501595548678134,25.));
#22133=CARTESIAN_POINT('Ctrl Pts',(8.03015889077922,0.389716765319841,25.));
#22134=CARTESIAN_POINT('Ctrl Pts',(8.03036837961706,0.277661727596636,25.));
#22135=CARTESIAN_POINT('Ctrl Pts',(8.02475908266942,0.165767231301056,25.));
#22136=CARTESIAN_POINT('Ctrl Pts',(8.02123118697422,0.0953926165353414,
25.));
#22137=CARTESIAN_POINT('Ctrl Pts',(8.01540028668034,0.0250817784959784,
25.));
#22138=CARTESIAN_POINT('Ctrl Pts',(8.00730734899356,-0.0450760163560306,
25.));
#22139=CARTESIAN_POINT('Ctrl Pts',(8.00445998309532,-0.0697598728602317,
25.));
#22140=CARTESIAN_POINT('Ctrl Pts',(8.0013325513392,-0.0944247476893036,
25.));
#22141=CARTESIAN_POINT('Ctrl Pts',(7.99792666298958,-0.119066624073926,
25.));
#22142=CARTESIAN_POINT('Ctrl Pts',(7.99555860106597,-0.136199742721088,
25.));
#22143=CARTESIAN_POINT('Ctrl Pts',(7.99305592559248,-0.15332174198476,25.));
#22144=CARTESIAN_POINT('Ctrl Pts',(7.99041915317417,-0.170431250299178,
25.));
#22145=CARTESIAN_POINT('Ctrl Pts',(7.98799100859738,-0.186187012736873,
25.));
#22146=CARTESIAN_POINT('Ctrl Pts',(7.9854507348484,-0.201921874689769,25.));
#22147=CARTESIAN_POINT('Ctrl Pts',(7.98279921776876,-0.217634511774155,
25.));
#22148=CARTESIAN_POINT('Ctrl Pts',(7.96426655575293,-0.327457297642062,
25.));
#22149=CARTESIAN_POINT('Ctrl Pts',(7.94030270069075,-0.436201906481619,
25.));
#22150=CARTESIAN_POINT('Ctrl Pts',(7.9111583335056,-0.543544308822202,25.));
#22151=CARTESIAN_POINT('Ctrl Pts',(7.88176382174181,-0.651808025385636,
25.));
#22152=CARTESIAN_POINT('Ctrl Pts',(7.84709896318544,-0.758646156812924,
25.));
#22153=CARTESIAN_POINT('Ctrl Pts',(7.80737187366647,-0.863705046597303,
25.));
#22154=CARTESIAN_POINT('Ctrl Pts',(7.76796016818941,-0.967929898507259,
25.));
#22155=CARTESIAN_POINT('Ctrl Pts',(7.72356567274187,-1.07040433957342,25.));
#22156=CARTESIAN_POINT('Ctrl Pts',(7.67435221978444,-1.1707512522537,25.));
#22157=CARTESIAN_POINT('Ctrl Pts',(7.63780678964462,-1.24526789082966,25.));
#22158=CARTESIAN_POINT('Ctrl Pts',(7.59860314278265,-1.3186107266499,25.));
#22159=CARTESIAN_POINT('Ctrl Pts',(7.55679710264817,-1.39061045069194,25.));
#22160=CARTESIAN_POINT('Ctrl Pts',(7.54382354621943,-1.41295393215319,25.));
#22161=CARTESIAN_POINT('Ctrl Pts',(7.53059592920725,-1.43517328189461,25.));
#22162=CARTESIAN_POINT('Ctrl Pts',(7.5171342266019,-1.45723356452538,25.));
#22163=CARTESIAN_POINT('Ctrl Pts',(7.45980912985136,-1.5511747154502,25.));
#22164=CARTESIAN_POINT('Ctrl Pts',(7.39819567619662,-1.6423191515338,25.));
#22165=CARTESIAN_POINT('Ctrl Pts',(7.33247571024972,-1.73031495540587,25.));
#22166=CARTESIAN_POINT('Ctrl Pts',(7.26804518737958,-1.81658425838204,25.));
#22167=CARTESIAN_POINT('Ctrl Pts',(7.19966708766734,-1.89982778265251,25.));
#22168=CARTESIAN_POINT('Ctrl Pts',(7.12748327748908,-1.97967407510293,25.));
#22169=CARTESIAN_POINT('Ctrl Pts',(7.0897166865762,-2.02144967901518,25.));
#22170=CARTESIAN_POINT('Ctrl Pts',(7.05090789035874,-2.06229461737513,25.));
#22171=CARTESIAN_POINT('Ctrl Pts',(7.01107473761725,-2.10215051102057,25.));
#22172=CARTESIAN_POINT('Ctrl Pts',(6.99916885841126,-2.11406318733992,25.));
#22173=CARTESIAN_POINT('Ctrl Pts',(6.98717216270953,-2.12588669985116,25.));
#22174=CARTESIAN_POINT('Ctrl Pts',(6.97509242397457,-2.13761259353056,25.));
#22175=CARTESIAN_POINT('Ctrl Pts',(6.89922337743233,-2.21125925036905,25.));
#22176=CARTESIAN_POINT('Ctrl Pts',(6.8200049496152,-2.28113499295858,25.));
#22177=CARTESIAN_POINT('Ctrl Pts',(6.73758357244001,-2.34689524282683,25.));
#22178=CARTESIAN_POINT('Ctrl Pts',(6.65741395726351,-2.41085891471067,25.));
#22179=CARTESIAN_POINT('Ctrl Pts',(6.5742134611503,-2.47092921323422,25.));
#22180=CARTESIAN_POINT('Ctrl Pts',(6.48809738068911,-2.52674429457259,25.));
#22181=CARTESIAN_POINT('Ctrl Pts',(6.4358172361143,-2.56062902906351,25.));
#22182=CARTESIAN_POINT('Ctrl Pts',(6.3824621897991,-2.59294458138693,25.));
#22183=CARTESIAN_POINT('Ctrl Pts',(6.32805563795715,-2.62360084935064,25.));
#22184=CARTESIAN_POINT('Ctrl Pts',(5.88688308661327,2.88166464694226,-0.413294290592403));
#22185=CARTESIAN_POINT('Ctrl Pts',(6.84537358445575,2.40588471549031,-0.347122251455184));
#22186=CARTESIAN_POINT('Ctrl Pts',(8.23365752427788,0.430873938343679,-0.214778173180747));
#22187=CARTESIAN_POINT('Ctrl Pts',(6.86376121760315,-2.94715670275194,-0.0162620557690901));
#22188=CARTESIAN_POINT('Ctrl Pts',(3.28608690294124,-3.61718018023642,0.182254061642566));
#22189=CARTESIAN_POINT('Ctrl Pts',(0.781880406995935,-0.979166244321737,
0.380770179054222));
#22190=CARTESIAN_POINT('Ctrl Pts',(1.64193314359211,2.55787552455616,0.579286296465875));
#22191=CARTESIAN_POINT('Ctrl Pts',(5.07993189931123,3.75125370222575,0.777802413877532));
#22192=CARTESIAN_POINT('Ctrl Pts',(7.94674205925474,1.50993542852403,0.976318531289188));
#22193=CARTESIAN_POINT('Ctrl Pts',(7.61734820438694,-2.11448150974993,1.17483464870084));
#22194=CARTESIAN_POINT('Ctrl Pts',(4.39321803491158,-3.80232526959411,1.3733507661125));
#22195=CARTESIAN_POINT('Ctrl Pts',(1.22704502026327,-2.0081611280352,1.57186688352415));
#22196=CARTESIAN_POINT('Ctrl Pts',(1.01829993859556,1.62508529687376,1.77038300093581));
#22197=CARTESIAN_POINT('Ctrl Pts',(3.95817375267475,3.77008527062174,1.96889911834747));
#22198=CARTESIAN_POINT('Ctrl Pts',(7.35437229592725,2.462525507432,2.16741523575912));
#22199=CARTESIAN_POINT('Ctrl Pts',(8.09672865983581,-1.10017486129741,2.36593135317078));
#22200=CARTESIAN_POINT('Ctrl Pts',(5.50540329893836,-3.65535258567839,2.56444747058243));
#22201=CARTESIAN_POINT('Ctrl Pts',(1.95348461951634,-2.8630297341532,2.76296358799409));
#22202=CARTESIAN_POINT('Ctrl Pts',(0.693751175975549,0.551202220257554,
2.96147970540574));
#22203=CARTESIAN_POINT('Ctrl Pts',(2.87984341841113,3.46065318004877,3.1599958228174));
#22204=CARTESIAN_POINT('Ctrl Pts',(6.50977938134639,3.20090403962421,3.35851194022905));
#22205=CARTESIAN_POINT('Ctrl Pts',(8.25933290131072,0.00982773524565914,
3.55702805764071));
#22206=CARTESIAN_POINT('Ctrl Pts',(6.52629607038668,-3.19024855326339,3.75554417505237));
#22207=CARTESIAN_POINT('Ctrl Pts',(2.89775109124319,-3.46875593755042,3.95406029246402));
#22208=CARTESIAN_POINT('Ctrl Pts',(0.69665041333009,-0.570642598253718,
4.15257640987568));
#22209=CARTESIAN_POINT('Ctrl Pts',(1.93872017863753,2.85005436799852,4.35109252728733));
#22210=CARTESIAN_POINT('Ctrl Pts',(5.48649651727959,3.66072576290342,4.54960864469899));
#22211=CARTESIAN_POINT('Ctrl Pts',(8.09099334705098,1.11897413587954,4.74812476211065));
#22212=CARTESIAN_POINT('Ctrl Pts',(7.36706201253862,-2.44751271825679,4.9466408795223));
#22213=CARTESIAN_POINT('Ctrl Pts',(3.97766506003213,-3.7726139823619,5.14515699693396));
#22214=CARTESIAN_POINT('Ctrl Pts',(1.02674774506536,-1.64282712377203,5.34367311434561));
#22215=CARTESIAN_POINT('Ctrl Pts',(1.21670401249677,1.99142956468722,5.54218923175727));
#22216=CARTESIAN_POINT('Ctrl Pts',(4.37357552585394,3.80197293891488,5.74070534916892));
#22217=CARTESIAN_POINT('Ctrl Pts',(7.60635940332531,2.13074181682499,5.93922146658058));
#22218=CARTESIAN_POINT('Ctrl Pts',(7.95453366396254,-1.49178213007847,6.13773758399224));
#22219=CARTESIAN_POINT('Ctrl Pts',(5.09924694286633,-3.74816037897555,6.33625370140389));
#22220=CARTESIAN_POINT('Ctrl Pts',(1.65531650589596,-2.57204465036969,6.53476981881556));
#22221=CARTESIAN_POINT('Ctrl Pts',(0.776628336729841,0.959500643563771,
6.7332859362272));
#22222=CARTESIAN_POINT('Ctrl Pts',(3.26786834626679,3.6123534997611,6.93180205363886));
#22223=CARTESIAN_POINT('Ctrl Pts',(6.84760632218384,2.95708173512582,7.1303181710505));
#22224=CARTESIAN_POINT('Ctrl Pts',(8.23758631997216,-0.406229232878139,
7.32883428846218));
#22225=CARTESIAN_POINT('Ctrl Pts',(6.16489109788061,-3.39752319671194,7.52735040587382));
#22226=CARTESIAN_POINT('Ctrl Pts',(2.52765551345678,-3.27743004474078,7.72586652328549));
#22227=CARTESIAN_POINT('Ctrl Pts',(0.656790727359,-0.155928801126063,7.92438264069713));
#22228=CARTESIAN_POINT('Ctrl Pts',(2.26559912307384,3.10836907247963,8.1228987581088));
#22229=CARTESIAN_POINT('Ctrl Pts',(5.88076457458627,3.52608167695778,8.32141487552045));
#22230=CARTESIAN_POINT('Ctrl Pts',(8.19158732913988,0.714675754863574,8.5199309929321));
#22231=CARTESIAN_POINT('Ctrl Pts',(7.08185986462416,-2.75121662896035,8.71844711034376));
#22232=CARTESIAN_POINT('Ctrl Pts',(3.56784948378791,-3.69759715767183,8.91696322775543));
#22233=CARTESIAN_POINT('Ctrl Pts',(0.867620049835816,-1.2577885451434,9.11547934516706));
#22234=CARTESIAN_POINT('Ctrl Pts',(1.45399031457103,2.33387889135228,9.31399546257875));
#22235=CARTESIAN_POINT('Ctrl Pts',(4.78997354349419,3.78822443423146,9.51251157999037));
#22236=CARTESIAN_POINT('Ctrl Pts',(7.8205397526871,1.77338609991104,9.71102769740205));
#22237=CARTESIAN_POINT('Ctrl Pts',(7.77035405525285,-1.8654854913274,9.90954381481369));
#22238=CARTESIAN_POINT('Ctrl Pts',(4.68537555826851,-3.79598095490491,10.1080599322253));
#22239=CARTESIAN_POINT('Ctrl Pts',(1.39076888675897,-2.25018926719472,10.306576049637));
#22240=CARTESIAN_POINT('Ctrl Pts',(0.903672160428571,1.35628294827392,10.5050921670486));
#22241=CARTESIAN_POINT('Ctrl Pts',(3.67015929568852,3.72069703895061,10.7036082844603));
#22242=CARTESIAN_POINT('Ctrl Pts',(7.156733998233,2.67776755651859,10.902124401872));
#22243=CARTESIAN_POINT('Ctrl Pts',(8.17045747715504,-0.817410517633158,
11.1006405192836));
#22244=CARTESIAN_POINT('Ctrl Pts',(5.78298105352307,-3.56401958853324,11.2991566366953));
#22245=CARTESIAN_POINT('Ctrl Pts',(2.18071022148213,-3.04676731509573,11.4976727541069));
#22246=CARTESIAN_POINT('Ctrl Pts',(0.662536086558379,0.260656509846819,
11.6961888715186));
#22247=CARTESIAN_POINT('Ctrl Pts',(2.61877364278075,3.32937606128419,11.8947049889302));
#22248=CARTESIAN_POINT('Ctrl Pts',(6.25793774774488,3.34911634724554,12.0932211063419));
#22249=CARTESIAN_POINT('Ctrl Pts',(8.24735113836601,0.301799589347462,12.2917372237535));
#22250=CARTESIAN_POINT('Ctrl Pts',(6.76514687416864,-3.02189949163811,12.4902533411652));
#22251=CARTESIAN_POINT('Ctrl Pts',(3.16869942579002,-3.57820050080496,12.6887694585768));
#22252=CARTESIAN_POINT('Ctrl Pts',(0.751566954770839,-0.857653555925328,
12.8872855759885));
#22253=CARTESIAN_POINT('Ctrl Pts',(1.72731339933552,2.64831620117018,13.0858016934002));
#22254=CARTESIAN_POINT('Ctrl Pts',(5.20236872621718,3.72900835754984,13.2843178108118));
#22255=CARTESIAN_POINT('Ctrl Pts',(7.99434336961907,1.39474559334568,13.4828339282235));
#22256=CARTESIAN_POINT('Ctrl Pts',(7.54640006010282,-2.21679865437008,13.6813500456351));
#22257=CARTESIAN_POINT('Ctrl Pts',(4.26875675973819,-3.79824086239538,13.8798661630468));
#22258=CARTESIAN_POINT('Ctrl Pts',(1.16301685561255,-1.9013263388412,14.0783822804584));
#22259=CARTESIAN_POINT('Ctrl Pts',(1.07335787448695,1.73678667876183,14.2768983978701));
#22260=CARTESIAN_POINT('Ctrl Pts',(4.08188780578152,3.78438349314049,14.4754145152818));
#22261=CARTESIAN_POINT('Ctrl Pts',(7.43345216672421,2.36631389110821,14.6739306326934));
#22262=CARTESIAN_POINT('Ctrl Pts',(8.05875206907788,-1.21878096033793,14.8724467501051));
#22263=CARTESIAN_POINT('Ctrl Pts',(5.38514975673243,-3.68773939197872,15.0709628675167));
#22264=CARTESIAN_POINT('Ctrl Pts',(1.86107937002522,-2.77953623668677,15.2694789849284));
#22265=CARTESIAN_POINT('Ctrl Pts',(0.713817534175901,0.674113331777405,
15.46799510234));
#22266=CARTESIAN_POINT('Ctrl Pts',(2.9940048152212,3.5104227339951,15.6665112197517));
#22267=CARTESIAN_POINT('Ctrl Pts',(6.61348907494099,3.13195377174095,15.8650273371633));
#22268=CARTESIAN_POINT('Ctrl Pts',(8.257615478175,-0.114698878595687,16.063543454575));
#22269=CARTESIAN_POINT('Ctrl Pts',(6.42072433944188,-3.25631247771842,16.2620595719866));
#22270=CARTESIAN_POINT('Ctrl Pts',(2.78500562221897,-3.41585705137789,16.4605756893983));
#22271=CARTESIAN_POINT('Ctrl Pts',(0.67998136903583,-0.447224713876356,
16.65909180681));
#22272=CARTESIAN_POINT('Ctrl Pts',(2.03339274915041,2.93096750947701,16.8576079242216));
#22273=CARTESIAN_POINT('Ctrl Pts',(5.60581136526813,3.62503544056518,17.0561240416333));
#22274=CARTESIAN_POINT('Ctrl Pts',(8.12568420335589,0.999364870669326,17.2546401590449));
#22275=CARTESIAN_POINT('Ctrl Pts',(7.28535965135699,-2.54150503784963,17.4531562764566));
#22276=CARTESIAN_POINT('Ctrl Pts',(3.85439094932391,-3.75491297725849,17.6516723938682));
#22277=CARTESIAN_POINT('Ctrl Pts',(0.974793970633971,-1.52964303811135,
17.8501885112799));
#22278=CARTESIAN_POINT('Ctrl Pts',(1.2836488526281,2.09644489844015,18.0487046286916));
#22279=CARTESIAN_POINT('Ctrl Pts',(4.49811216942012,3.80264847561477,18.2472207461032));
#22280=CARTESIAN_POINT('Ctrl Pts',(7.67443956106538,2.02645891285741,18.4457368635149));
#22281=CARTESIAN_POINT('Ctrl Pts',(7.90381082245328,-1.60552317494378,18.6442529809265));
#22282=CARTESIAN_POINT('Ctrl Pts',(4.9761721155001,-3.76719767944954,18.8427690983382));
#22283=CARTESIAN_POINT('Ctrl Pts',(1.57259927845708,-2.47894420875808,19.0412852157498));
#22284=CARTESIAN_POINT('Ctrl Pts',(0.810019572635768,1.07947921368855,19.2398013331615));
#22285=CARTESIAN_POINT('Ctrl Pts',(3.38678898688482,3.6493361063157,19.4383174505731));
#22286=CARTESIAN_POINT('Ctrl Pts',(6.94315110686829,2.87720041011993,19.6368335679848));
#22287=CARTESIAN_POINT('Ctrl Pts',(8.22225715251285,-0.529820690755693,
19.8353496853965));
#22288=CARTESIAN_POINT('Ctrl Pts',(6.05272613795891,-3.45164208273989,20.0338658028081));
#22289=CARTESIAN_POINT('Ctrl Pts',(2.42137329831411,-3.212515309774,20.2323819202198));
#22290=CARTESIAN_POINT('Ctrl Pts',(0.65372248686789,-0.0314281299545405,
20.4308980376314));
#22291=CARTESIAN_POINT('Ctrl Pts',(2.36855469553213,3.178440343651,20.6294141550431));
#22292=CARTESIAN_POINT('Ctrl Pts',(5.99545920128352,3.47755359131801,20.8279302724548));
#22293=CARTESIAN_POINT('Ctrl Pts',(8.21298586010566,0.591989447683331,21.0264463898664));
#22294=CARTESIAN_POINT('Ctrl Pts',(6.99036591797756,-2.83570744333498,21.2249625072781));
#22295=CARTESIAN_POINT('Ctrl Pts',(3.44725150283742,-3.6665172604341,21.4234786246897));
#22296=CARTESIAN_POINT('Ctrl Pts',(0.828359319011244,-1.13960058009792,
21.6219947421014));
#22297=CARTESIAN_POINT('Ctrl Pts',(1.53202116508044,2.43094114262164,21.820510859513));
#22298=CARTESIAN_POINT('Ctrl Pts',(4.91383661347899,3.77527223251319,22.0190269769247));
#22299=CARTESIAN_POINT('Ctrl Pts',(7.87680396956558,1.66228269728872,22.2175430943363));
#22300=CARTESIAN_POINT('Ctrl Pts',(7.7074930081086,-1.97299730385434,22.416059211748));
#22301=CARTESIAN_POINT('Ctrl Pts',(4.56095756308617,-3.80143701374933,22.6145753291597));
#22302=CARTESIAN_POINT('Ctrl Pts',(1.31873095853907,-2.14860623751896,22.8130914465713));
#22303=CARTESIAN_POINT('Ctrl Pts',(0.949990286798536,1.47190262315773,23.011607563983));
#22304=CARTESIAN_POINT('Ctrl Pts',(3.7924065803434,3.74442240079083,23.2101236813946));
#22305=CARTESIAN_POINT('Ctrl Pts',(7.24297719250067,2.58796472414074,23.4086397988063));
#22306=CARTESIAN_POINT('Ctrl Pts',(8.14168123233833,-0.938680920498277,
23.6071559162179));
#22307=CARTESIAN_POINT('Ctrl Pts',(5.66560616055497,-3.60535681683013,23.8056720336296));
#22308=CARTESIAN_POINT('Ctrl Pts',(2.08209581503262,-2.97097481614092,24.0041881510412));
#22309=CARTESIAN_POINT('Ctrl Pts',(0.673241827254791,0.385434817028999,
24.2027042684529));
#22310=CARTESIAN_POINT('Ctrl Pts',(2.72851506381635,3.38643791990783,24.4012203858645));
#22311=CARTESIAN_POINT('Ctrl Pts',(6.36713580394013,3.29091791303403,24.5997365032762));
#22312=CARTESIAN_POINT('Ctrl Pts',(8.25465969525897,0.17151120336101,24.7982954766299));
#22313=CARTESIAN_POINT('Ctrl Pts',(7.19525837483205,-1.99900958588141,24.9306824108463));
#22314=CARTESIAN_POINT('Ctrl Pts',(6.32311239899223,-2.62025147071356,24.9968973059255));
#22315=CARTESIAN_POINT('Ctrl Pts',(5.99341579333084,3.0962819108244,-0.27495920519366));
#22316=CARTESIAN_POINT('Ctrl Pts',(7.02329163031133,2.58506739568259,-0.208787166056442));
#22317=CARTESIAN_POINT('Ctrl Pts',(8.51497056474962,0.462964065771816,-0.0764430877820045));
#22318=CARTESIAN_POINT('Ctrl Pts',(7.04304871618797,-3.16665160770128,0.122073029629653));
#22319=CARTESIAN_POINT('Ctrl Pts',(3.19892054011338,-3.88657631350085,0.320589147041309));
#22320=CARTESIAN_POINT('Ctrl Pts',(0.508208668906595,-1.05209144762919,
0.519105264452963));
#22321=CARTESIAN_POINT('Ctrl Pts',(1.43231541168923,2.74837799923302,0.717621381864618));
#22322=CARTESIAN_POINT('Ctrl Pts',(5.12636543519397,4.03063520713254,0.916137499276276));
#22323=CARTESIAN_POINT('Ctrl Pts',(8.20668654383497,1.62239064105283,1.11465361668793));
#22324=CARTESIAN_POINT('Ctrl Pts',(7.85276047702285,-2.27196140132349,1.31316973409959));
#22325=CARTESIAN_POINT('Ctrl Pts',(4.38850729527858,-4.08551042322263,1.51168585151124));
#22326=CARTESIAN_POINT('Ctrl Pts',(0.986527733847538,-2.15772261402933,
1.7102019689229));
#22327=CARTESIAN_POINT('Ctrl Pts',(0.7622359790706,1.74611650720567,1.90871808633455));
#22328=CARTESIAN_POINT('Ctrl Pts',(3.92106229159746,4.0508692911502,2.10723420374621));
#22329=CARTESIAN_POINT('Ctrl Pts',(7.57019895508782,2.64592661456843,2.30575032115786));
#22330=CARTESIAN_POINT('Ctrl Pts',(8.36784367179503,-1.18211240346562,2.50426643856952));
#22331=CARTESIAN_POINT('Ctrl Pts',(5.58352459826198,-3.92759167890361,2.70278255598118));
#22332=CARTESIAN_POINT('Ctrl Pts',(1.7670702556363,-3.07625912870098,2.90129867339283));
#22333=CARTESIAN_POINT('Ctrl Pts',(0.413515851644582,0.592254017343965,
3.09981479080449));
#22334=CARTESIAN_POINT('Ctrl Pts',(2.76242132641212,3.7183916776686,3.29833090821614));
#22335=CARTESIAN_POINT('Ctrl Pts',(6.66270343294158,3.43929724324088,3.4968470256278));
#22336=CARTESIAN_POINT('Ctrl Pts',(8.54255816261418,0.0105596738669375,
3.69536314303945));
#22337=CARTESIAN_POINT('Ctrl Pts',(6.6804502327146,-3.42784816997514,3.89387926045112));
#22338=CARTESIAN_POINT('Ctrl Pts',(2.78166270604797,-3.72709790290783,4.09239537786277));
#22339=CARTESIAN_POINT('Ctrl Pts',(0.416631015022661,-0.613142253174304,
4.29091149527442));
#22340=CARTESIAN_POINT('Ctrl Pts',(1.75120620592284,3.06231739833558,4.48942761268608));
#22341=CARTESIAN_POINT('Ctrl Pts',(5.56320969933569,3.93336503336498,4.68794373009773));
#22342=CARTESIAN_POINT('Ctrl Pts',(8.36168121106336,1.20231178852842,4.88645984750939));
#22343=CARTESIAN_POINT('Ctrl Pts',(7.58383376163584,-2.62979572036334,5.08497596492104));
#22344=CARTESIAN_POINT('Ctrl Pts',(3.94200524984668,-4.05358633333867,5.2834920823327));
#22345=CARTESIAN_POINT('Ctrl Pts',(0.771312951433223,-1.76517968922739,
5.48200819974436));
#22346=CARTESIAN_POINT('Ctrl Pts',(0.97541656054666,2.13974493679014,5.68052431715601));
#22347=CARTESIAN_POINT('Ctrl Pts',(4.36740187430494,4.08513185206935,5.87904043456767));
#22348=CARTESIAN_POINT('Ctrl Pts',(7.84095326483218,2.28943272461384,6.07755655197932));
#22349=CARTESIAN_POINT('Ctrl Pts',(8.21505844260491,-1.60288534238506,6.27607266939098));
#22350=CARTESIAN_POINT('Ctrl Pts',(5.14711900207072,-4.02731150295548,6.47458878680263));
#22351=CARTESIAN_POINT('Ctrl Pts',(1.44669552446588,-2.76360239669899,6.6731049042143));
#22352=CARTESIAN_POINT('Ctrl Pts',(0.502565441067234,1.03096121515846,6.87162102162594));
#22353=CARTESIAN_POINT('Ctrl Pts',(3.17934512299035,3.88139015713774,7.07013713903761));
#22354=CARTESIAN_POINT('Ctrl Pts',(7.0256906552799,3.17731582507866,7.26865325644925));
#22355=CARTESIAN_POINT('Ctrl Pts',(8.51919196471455,-0.436483900631263,
7.46716937386092));
#22356=CARTESIAN_POINT('Ctrl Pts',(6.2921289615216,-3.65055997294754,7.66568549127257));
#22357=CARTESIAN_POINT('Ctrl Pts',(2.38400358079477,-3.52152266305215,7.86420160868423));
#22358=CARTESIAN_POINT('Ctrl Pts',(0.373802705776339,-0.16754188479758,
8.06271772609589));
#22359=CARTESIAN_POINT('Ctrl Pts',(2.10243005973299,3.33987056457006,8.26123384350753));
#22360=CARTESIAN_POINT('Ctrl Pts',(5.98684159389007,3.78869308197905,8.4597499609192));
#22361=CARTESIAN_POINT('Ctrl Pts',(8.4697671146088,0.767902543495819,8.65826607833084));
#22362=CARTESIAN_POINT('Ctrl Pts',(7.27739066026635,-2.95611853726567,8.85678219574251));
#22363=CARTESIAN_POINT('Ctrl Pts',(3.50166790634439,-3.97298249293629,9.05529831315416));
#22364=CARTESIAN_POINT('Ctrl Pts',(0.600333929022254,-1.35146465571633,
9.25381443056581));
#22365=CARTESIAN_POINT('Ctrl Pts',(1.23037519550738,2.50769880562501,9.45233054797748));
#22366=CARTESIAN_POINT('Ctrl Pts',(4.81481189860833,4.07035940226423,9.65084666538912));
#22367=CARTESIAN_POINT('Ctrl Pts',(8.07108508884113,1.90546228475562,9.84936278280079));
#22368=CARTESIAN_POINT('Ctrl Pts',(8.01716171947454,-2.00442094739626,10.0478789002124));
#22369=CARTESIAN_POINT('Ctrl Pts',(4.70242378644322,-4.07869360405195,10.2463950176241));
#22370=CARTESIAN_POINT('Ctrl Pts',(1.16244523581599,-2.41777624309588,10.4449111350357));
#22371=CARTESIAN_POINT('Ctrl Pts',(0.639071086725107,1.45729461030662,10.6434272524474));
#22372=CARTESIAN_POINT('Ctrl Pts',(3.61159742927608,3.99780278027315,10.841943369859));
#22373=CARTESIAN_POINT('Ctrl Pts',(7.35784118240728,2.87719921033794,11.0404594872707));
#22374=CARTESIAN_POINT('Ctrl Pts',(8.44706357811351,-0.878288666292467,
11.2389756046823));
#22375=CARTESIAN_POINT('Ctrl Pts',(5.88177546561389,-3.82945648915419,11.437491722094));
#22376=CARTESIAN_POINT('Ctrl Pts',(2.01121890138154,-3.27368090323489,11.6360078395057));
#22377=CARTESIAN_POINT('Ctrl Pts',(0.379975961147697,0.280069381853164,
11.8345239569173));
#22378=CARTESIAN_POINT('Ctrl Pts',(2.4819079000476,3.57733745452462,12.033040074329));
#22379=CARTESIAN_POINT('Ctrl Pts',(6.39210543142176,3.59854793451629,12.2315561917406));
#22380=CARTESIAN_POINT('Ctrl Pts',(8.52968403588164,0.324276667717884,12.4300723091523));
#22381=CARTESIAN_POINT('Ctrl Pts',(6.93708988851933,-3.24696100298028,12.6285884265639));
#22382=CARTESIAN_POINT('Ctrl Pts',(3.07279041513639,-3.84469355089646,12.8271045439756));
#22383=CARTESIAN_POINT('Ctrl Pts',(0.475637566686629,-0.921528878727684,
13.0256206613872));
#22384=CARTESIAN_POINT('Ctrl Pts',(1.52405451869475,2.84555441124189,13.2241367787989));
#22385=CARTESIAN_POINT('Ctrl Pts',(5.25792096951678,4.00673309958052,13.4226528962106));
#22386=CARTESIAN_POINT('Ctrl Pts',(8.257833049161,1.4986218314684,13.6211690136222));
#22387=CARTESIAN_POINT('Ctrl Pts',(7.77652833946771,-2.38189880309254,13.8196851310339));
#22388=CARTESIAN_POINT('Ctrl Pts',(4.25477653818775,-4.08112182230083,14.0182012484455));
#22389=CARTESIAN_POINT('Ctrl Pts',(0.917730954110628,-2.04293110781465,
14.2167173658572));
#22390=CARTESIAN_POINT('Ctrl Pts',(0.821394455796449,1.86613705453794,14.4152334832688));
#22391=CARTESIAN_POINT('Ctrl Pts',(4.05399017588675,4.06623240003544,14.6137496006805));
#22392=CARTESIAN_POINT('Ctrl Pts',(7.65516844441363,2.54254946152231,14.8122657180922));
#22393=CARTESIAN_POINT('Ctrl Pts',(8.32703870473431,-1.30955190943392,15.0107818355038));
#22394=CARTESIAN_POINT('Ctrl Pts',(5.45431495277465,-3.96239055204922,15.2092979529155));
#22395=CARTESIAN_POINT('Ctrl Pts',(1.66778295557931,-2.98654729975826,15.4078140703271));
#22396=CARTESIAN_POINT('Ctrl Pts',(0.435076688703739,0.724319159497842,
15.6063301877388));
#22397=CARTESIAN_POINT('Ctrl Pts',(2.88508510279309,3.77186791049719,15.8048463051504));
#22398=CARTESIAN_POINT('Ctrl Pts',(6.77413709632598,3.36521177759866,16.0033624225621));
#22399=CARTESIAN_POINT('Ctrl Pts',(8.54071283123811,-0.123241288109086,
16.2018785399737));
#22400=CARTESIAN_POINT('Ctrl Pts',(6.56701585333057,-3.49883232646441,16.4003946573854));
#22401=CARTESIAN_POINT('Ctrl Pts',(2.66052031127365,-3.67025927509159,16.598910774797));
#22402=CARTESIAN_POINT('Ctrl Pts',(0.398720513058523,-0.480532595324168,
16.7974268922087));
#22403=CARTESIAN_POINT('Ctrl Pts',(1.85292968989636,3.14925669454191,16.9959430096203));
#22404=CARTESIAN_POINT('Ctrl Pts',(5.69141073963082,3.89501660876095,17.194459127032));
#22405=CARTESIAN_POINT('Ctrl Pts',(8.39895573256671,1.07379440374864,17.3929752444437));
#22406=CARTESIAN_POINT('Ctrl Pts',(7.49604646714037,-2.73078829048094,17.5914913618553));
#22407=CARTESIAN_POINT('Ctrl Pts',(3.80955007347359,-4.03456701338995,17.790007479267));
#22408=CARTESIAN_POINT('Ctrl Pts',(0.715489824289806,-1.64356601103751,
17.9885235966786));
#22409=CARTESIAN_POINT('Ctrl Pts',(1.04734724052415,2.25258148028018,18.1870397140903));
#22410=CARTESIAN_POINT('Ctrl Pts',(4.50121361298798,4.08585770060491,18.3855558315019));
#22411=CARTESIAN_POINT('Ctrl Pts',(7.91410381728119,2.1773831599618,18.5840719489136));
#22412=CARTESIAN_POINT('Ctrl Pts',(8.16055792437237,-1.72509746033864,18.7825880663253));
#22413=CARTESIAN_POINT('Ctrl Pts',(5.0148779510323,-4.04776664132528,18.9811041837369));
#22414=CARTESIAN_POINT('Ctrl Pts',(1.35781777968586,-2.66356812881232,19.1796203011486));
#22415=CARTESIAN_POINT('Ctrl Pts',(0.538443550556935,1.1598754095142,19.3781364185603));
#22416=CARTESIAN_POINT('Ctrl Pts',(3.30712259659747,3.92112711119714,19.5766525359719));
#22417=CARTESIAN_POINT('Ctrl Pts',(7.12835131317638,3.09148519177063,19.7751686533836));
#22418=CARTESIAN_POINT('Ctrl Pts',(8.50272112937199,-0.569280059186615,
19.9736847707952));
#22419=CARTESIAN_POINT('Ctrl Pts',(6.17161031033075,-3.70870946234774,20.1722008882069));
#22420=CARTESIAN_POINT('Ctrl Pts',(2.26980580259814,-3.45177328404759,20.3707170056185));
#22421=CARTESIAN_POINT('Ctrl Pts',(0.370505952442893,-0.0337687976193256,
20.5692331230302));
#22422=CARTESIAN_POINT('Ctrl Pts',(2.21305343742525,3.41516052227788,20.7677492404418));
#22423=CARTESIAN_POINT('Ctrl Pts',(6.11007831343283,3.73655077808788,20.9662653578534));
#22424=CARTESIAN_POINT('Ctrl Pts',(8.49275934044528,0.636078948397367,21.1647814752652));
#22425=CARTESIAN_POINT('Ctrl Pts',(7.17908253400595,-3.04690196012391,21.3632975926768));
#22426=CARTESIAN_POINT('Ctrl Pts',(3.37208816940477,-3.93958786330456,21.5618137100885));
#22427=CARTESIAN_POINT('Ctrl Pts',(0.558149183206385,-1.22447442503984,
21.7603298275001));
#22428=CARTESIAN_POINT('Ctrl Pts',(1.31421753683424,2.61198994621562,21.9588459449118));
#22429=CARTESIAN_POINT('Ctrl Pts',(4.94789989808116,4.05644256154919,22.1573620623234));
#22430=CARTESIAN_POINT('Ctrl Pts',(8.13153968654471,1.78608425229248,22.3558781797351));
#22431=CARTESIAN_POINT('Ctrl Pts',(7.94961898046267,-2.11993989949929,22.5543942971467));
#22432=CARTESIAN_POINT('Ctrl Pts',(4.56873953270021,-4.0845560128934,22.7529104145584));
#22433=CARTESIAN_POINT('Ctrl Pts',(1.08504215066615,-2.30862763082918,22.95142653197));
#22434=CARTESIAN_POINT('Ctrl Pts',(0.688838840573486,1.58152527269752,23.1499426493817));
#22435=CARTESIAN_POINT('Ctrl Pts',(3.74294930484078,4.02329513198439,23.3484587667933));
#22436=CARTESIAN_POINT('Ctrl Pts',(7.45050749686758,2.78070814718547,23.546974884205));
#22437=CARTESIAN_POINT('Ctrl Pts',(8.41614416964521,-1.00859090500303,23.7454910016166));
#22438=CARTESIAN_POINT('Ctrl Pts',(5.75565886205016,-3.87387238340306,23.9440071190283));
#22439=CARTESIAN_POINT('Ctrl Pts',(1.90526000600476,-3.19224361880315,24.14252323644));
#22440=CARTESIAN_POINT('Ctrl Pts',(0.391479031532891,0.414140782493564,
24.3410393538516));
#22441=CARTESIAN_POINT('Ctrl Pts',(2.59982251484541,3.6386490998064,24.5395554712633));
#22442=CARTESIAN_POINT('Ctrl Pts',(6.50943621328541,3.53601506509354,24.7380715886749));
#22443=CARTESIAN_POINT('Ctrl Pts',(8.53753691096405,0.184284815040506,24.9366305620286));
#22444=CARTESIAN_POINT('Ctrl Pts',(7.39923473266516,-2.14788949397592,25.069017496245));
#22445=CARTESIAN_POINT('Ctrl Pts',(6.46213408444902,-2.81539950847165,25.1352323913243));
#22446=CARTESIAN_POINT('Ctrl Pts',(6.0999485000484,3.31089917470656,-0.136624119794918));
#22447=CARTESIAN_POINT('Ctrl Pts',(7.2012096761669,2.76425007587486,-0.0704520806576993));
#22448=CARTESIAN_POINT('Ctrl Pts',(8.79628360522135,0.495054193199949,0.061891997616738));
#22449=CARTESIAN_POINT('Ctrl Pts',(7.22233621477278,-3.38614651265062,0.260408115028396));
#22450=CARTESIAN_POINT('Ctrl Pts',(3.11175417728552,-4.15597244676529,0.458924232440051));
#22451=CARTESIAN_POINT('Ctrl Pts',(0.234536930817258,-1.12501665093665,
0.657440349851707));
#22452=CARTESIAN_POINT('Ctrl Pts',(1.22269767978634,2.93888047390986,0.855956467263361));
#22453=CARTESIAN_POINT('Ctrl Pts',(5.17279897107673,4.31001671203934,1.05447258467502));
#22454=CARTESIAN_POINT('Ctrl Pts',(8.46663102841521,1.73484585358162,1.25298870208667));
#22455=CARTESIAN_POINT('Ctrl Pts',(8.08817274965877,-2.42944129289705,1.45150481949833));
#22456=CARTESIAN_POINT('Ctrl Pts',(4.38379655564558,-4.36869557685114,1.65002093690999));
#22457=CARTESIAN_POINT('Ctrl Pts',(0.746010447431816,-2.30728410002347,
1.84853705432164));
#22458=CARTESIAN_POINT('Ctrl Pts',(0.506172019545635,1.86714771753756,2.04705317173329));
#22459=CARTESIAN_POINT('Ctrl Pts',(3.88395083052018,4.33165331167866,2.24556928914495));
#22460=CARTESIAN_POINT('Ctrl Pts',(7.78602561424836,2.82932772170484,2.4440854065566));
#22461=CARTESIAN_POINT('Ctrl Pts',(8.63895868375428,-1.26404994563383,2.64260152396827));
#22462=CARTESIAN_POINT('Ctrl Pts',(5.66164589758561,-4.19983077212884,2.84111764137992));
#22463=CARTESIAN_POINT('Ctrl Pts',(1.58065589175627,-3.28948852324876,3.03963375879158));
#22464=CARTESIAN_POINT('Ctrl Pts',(0.133280527313607,0.633305814430374,
3.23814987620323));
#22465=CARTESIAN_POINT('Ctrl Pts',(2.6449992344131,3.97613017528841,3.43666599361489));
#22466=CARTESIAN_POINT('Ctrl Pts',(6.81562748453676,3.67769044685756,3.63518211102655));
#22467=CARTESIAN_POINT('Ctrl Pts',(8.82578342391765,0.0112916124882134,
3.8336982284382));
#22468=CARTESIAN_POINT('Ctrl Pts',(6.83460439504253,-3.66544778668689,4.03221434584986));
#22469=CARTESIAN_POINT('Ctrl Pts',(2.66557432085276,-3.98543986826524,4.23073046326151));
#22470=CARTESIAN_POINT('Ctrl Pts',(0.13661161671523,-0.655641908094887,
4.42924658067317));
#22471=CARTESIAN_POINT('Ctrl Pts',(1.56369223320815,3.27458042867263,4.62776269808482));
#22472=CARTESIAN_POINT('Ctrl Pts',(5.63992288139177,4.20600430382654,4.82627881549648));
#22473=CARTESIAN_POINT('Ctrl Pts',(8.63236907507575,1.28564944117731,5.02479493290813));
#22474=CARTESIAN_POINT('Ctrl Pts',(7.80060551073305,-2.81207872246989,5.22331105031979));
#22475=CARTESIAN_POINT('Ctrl Pts',(3.90634543966123,-4.33455868431544,5.42182716773146));
#22476=CARTESIAN_POINT('Ctrl Pts',(0.515878157801087,-1.88753225468275,
5.62034328514309));
#22477=CARTESIAN_POINT('Ctrl Pts',(0.734129108596551,2.28806030889307,5.81885940255477));
#22478=CARTESIAN_POINT('Ctrl Pts',(4.36122822275595,4.36829076522382,6.0173755199664));
#22479=CARTESIAN_POINT('Ctrl Pts',(8.07554712633902,2.44812363240269,6.21589163737808));
#22480=CARTESIAN_POINT('Ctrl Pts',(8.47558322124728,-1.71398855469165,6.41440775478972));
#22481=CARTESIAN_POINT('Ctrl Pts',(5.19499106127511,-4.3064626269354,6.61292387220138));
#22482=CARTESIAN_POINT('Ctrl Pts',(1.2380745430358,-2.9551601430283,6.81143998961304));
#22483=CARTESIAN_POINT('Ctrl Pts',(0.228502545404632,1.10242178675316,7.00995610702469));
#22484=CARTESIAN_POINT('Ctrl Pts',(3.09082189971391,4.15042681451437,7.20847222443635));
#22485=CARTESIAN_POINT('Ctrl Pts',(7.20377498837598,3.39754991503151,7.406988341848));
#22486=CARTESIAN_POINT('Ctrl Pts',(8.80079760945692,-0.466738568384383,
7.60550445925966));
#22487=CARTESIAN_POINT('Ctrl Pts',(6.41936682516261,-3.90359674918315,7.80402057667131));
#22488=CARTESIAN_POINT('Ctrl Pts',(2.24035164813274,-3.7656152813635,8.00253669408298));
#22489=CARTESIAN_POINT('Ctrl Pts',(0.0908146841936848,-0.179154968469096,
8.20105281149462));
#22490=CARTESIAN_POINT('Ctrl Pts',(1.93926099639212,3.57137205666049,8.39956892890629));
#22491=CARTESIAN_POINT('Ctrl Pts',(6.09291861319388,4.05130448700034,8.59808504631793));
#22492=CARTESIAN_POINT('Ctrl Pts',(8.7479469000777,0.821129332128062,8.7966011637296));
#22493=CARTESIAN_POINT('Ctrl Pts',(7.47292145590854,-3.16102044557099,8.99511728114126));
#22494=CARTESIAN_POINT('Ctrl Pts',(3.43548632890085,-4.24836782820074,9.19363339855291));
#22495=CARTESIAN_POINT('Ctrl Pts',(0.333047808208697,-1.44514076628925,
9.39214951596456));
#22496=CARTESIAN_POINT('Ctrl Pts',(1.00676007644372,2.68151871989772,9.59066563337622));
#22497=CARTESIAN_POINT('Ctrl Pts',(4.83965025372247,4.352494370297,9.78918175078787));
#22498=CARTESIAN_POINT('Ctrl Pts',(8.32163042499515,2.03753846960017,9.98769786819953));
#22499=CARTESIAN_POINT('Ctrl Pts',(8.26396938369623,-2.14335640346512,10.1862139856111));
#22500=CARTESIAN_POINT('Ctrl Pts',(4.71947201461794,-4.36140625319899,10.3847301030228));
#22501=CARTESIAN_POINT('Ctrl Pts',(0.934121584873003,-2.58536321899705,
10.5832462204345));
#22502=CARTESIAN_POINT('Ctrl Pts',(0.37447001302165,1.5583062723393,10.7817623378461));
#22503=CARTESIAN_POINT('Ctrl Pts',(3.55303556286365,4.27490852159572,10.9802784552578));
#22504=CARTESIAN_POINT('Ctrl Pts',(7.55894836658157,3.07663086415728,11.1787945726694));
#22505=CARTESIAN_POINT('Ctrl Pts',(8.72366967907197,-0.939166814951776,
11.3773106900811));
#22506=CARTESIAN_POINT('Ctrl Pts',(5.98056987770475,-4.09489338977514,11.5758268074927));
#22507=CARTESIAN_POINT('Ctrl Pts',(1.84172758128094,-3.50059449137405,11.7743429249044));
#22508=CARTESIAN_POINT('Ctrl Pts',(0.0974158357370281,0.299482253859507,
11.9728590423161));
#22509=CARTESIAN_POINT('Ctrl Pts',(2.34504215731444,3.82529884776504,12.1713751597277));
#22510=CARTESIAN_POINT('Ctrl Pts',(6.52627311509865,3.84797952178704,12.3698912771394));
#22511=CARTESIAN_POINT('Ctrl Pts',(8.81201693339725,0.346753746088307,12.568407394551));
#22512=CARTESIAN_POINT('Ctrl Pts',(7.10903290287004,-3.47202251432246,12.7669235119627));
#22513=CARTESIAN_POINT('Ctrl Pts',(2.97688140448274,-4.11118660098796,12.9654396293744));
#22514=CARTESIAN_POINT('Ctrl Pts',(0.199708178602426,-0.985404201530036,
13.163955746786));
#22515=CARTESIAN_POINT('Ctrl Pts',(1.32079563805398,3.0427926213136,13.3624718641977));
#22516=CARTESIAN_POINT('Ctrl Pts',(5.3134732128164,4.28445784161121,13.5609879816093));
#22517=CARTESIAN_POINT('Ctrl Pts',(8.52132272870291,1.60249806959112,13.759504099021));
#22518=CARTESIAN_POINT('Ctrl Pts',(8.00665661883263,-2.546998951815,13.9580202164326));
#22519=CARTESIAN_POINT('Ctrl Pts',(4.24079631663729,-4.36400278220629,14.1565363338443));
#22520=CARTESIAN_POINT('Ctrl Pts',(0.672445052608722,-2.18453587678811,
14.3550524512559));
#22521=CARTESIAN_POINT('Ctrl Pts',(0.569431037105937,1.99548743031406,14.5535685686676));
#22522=CARTESIAN_POINT('Ctrl Pts',(4.02609254599198,4.3480813069304,14.7520846860792));
#22523=CARTESIAN_POINT('Ctrl Pts',(7.87688472210303,2.7187850319364,14.9506008034909));
#22524=CARTESIAN_POINT('Ctrl Pts',(8.59532534039074,-1.40032285852991,15.1491169209026));
#22525=CARTESIAN_POINT('Ctrl Pts',(5.52348014881688,-4.2370417121197,15.3476330383142));
#22526=CARTESIAN_POINT('Ctrl Pts',(1.47448654113341,-3.19355836282975,15.5461491557259));
#22527=CARTESIAN_POINT('Ctrl Pts',(0.156335843231577,0.774524987218279,
15.7446652731375));
#22528=CARTESIAN_POINT('Ctrl Pts',(2.77616539036498,4.03331308699926,15.9431813905492));
#22529=CARTESIAN_POINT('Ctrl Pts',(6.93478511771097,3.59846978345639,16.1416975079608));
#22530=CARTESIAN_POINT('Ctrl Pts',(8.82381018430121,-0.131783697622486,
16.3402136253725));
#22531=CARTESIAN_POINT('Ctrl Pts',(6.71330736721926,-3.74135217521042,16.5387297427841));
#22532=CARTESIAN_POINT('Ctrl Pts',(2.53603500032833,-3.92466149880528,16.7372458601958));
#22533=CARTESIAN_POINT('Ctrl Pts',(0.117459657081213,-0.513840476771981,
16.9357619776075));
#22534=CARTESIAN_POINT('Ctrl Pts',(1.6724666306423,3.3675458796068,17.1342780950191));
#22535=CARTESIAN_POINT('Ctrl Pts',(5.77701011399349,4.16499777695671,17.3327942124308));
#22536=CARTESIAN_POINT('Ctrl Pts',(8.67222726177754,1.14822393682795,17.5313103298424));
#22537=CARTESIAN_POINT('Ctrl Pts',(7.70673328292373,-2.92007154311226,17.7298264472541));
#22538=CARTESIAN_POINT('Ctrl Pts',(3.76470919762329,-4.31422104952143,17.9283425646657));
#22539=CARTESIAN_POINT('Ctrl Pts',(0.456185677945633,-1.75748898396369,
18.1268586820774));
#22540=CARTESIAN_POINT('Ctrl Pts',(0.811045628420214,2.40871806212022,18.3253747994891));
#22541=CARTESIAN_POINT('Ctrl Pts',(4.50431505655582,4.36906692559506,18.5238909169007));
#22542=CARTESIAN_POINT('Ctrl Pts',(8.153768073497,2.32830740706619,18.7224070343124));
#22543=CARTESIAN_POINT('Ctrl Pts',(8.41730502629147,-1.84467174573349,18.920923151724));
#22544=CARTESIAN_POINT('Ctrl Pts',(5.05358378656449,-4.328335603201,19.1194392691357));
#22545=CARTESIAN_POINT('Ctrl Pts',(1.14303628091464,-2.84819204886657,19.3179553865473));
#22546=CARTESIAN_POINT('Ctrl Pts',(0.266867528478102,1.24027160533984,19.516471503959));
#22547=CARTESIAN_POINT('Ctrl Pts',(3.22745620631011,4.19291811607857,19.7149876213706));
#22548=CARTESIAN_POINT('Ctrl Pts',(7.31355151948446,3.30576997342133,19.9135037387823));
#22549=CARTESIAN_POINT('Ctrl Pts',(8.78318510623113,-0.60873942761753,20.112019856194));
#22550=CARTESIAN_POINT('Ctrl Pts',(6.29049448270258,-3.96577684195559,20.3105359736056));
#22551=CARTESIAN_POINT('Ctrl Pts',(2.11823830688215,-3.69103125832118,20.5090520910173));
#22552=CARTESIAN_POINT('Ctrl Pts',(0.0872894180178925,-0.0361094652841183,
20.7075682084289));
#22553=CARTESIAN_POINT('Ctrl Pts',(2.05755217931839,3.65188070090475,20.9060843258406));
#22554=CARTESIAN_POINT('Ctrl Pts',(6.2246974255821,3.99554796485774,21.1046004432522));
#22555=CARTESIAN_POINT('Ctrl Pts',(8.77253282078492,0.680168449111409,21.3031165606639));
#22556=CARTESIAN_POINT('Ctrl Pts',(7.36779915003431,-3.25809647691284,21.5016326780756));
#22557=CARTESIAN_POINT('Ctrl Pts',(3.29692483597213,-4.21265846617502,21.7001487954872));
#22558=CARTESIAN_POINT('Ctrl Pts',(0.287939047401517,-1.30934826998177,
21.8986649128989));
#22559=CARTESIAN_POINT('Ctrl Pts',(1.09641390858805,2.79303874980958,22.0971810303105));
#22560=CARTESIAN_POINT('Ctrl Pts',(4.98196318268333,4.33761289058522,22.2956971477222));
#22561=CARTESIAN_POINT('Ctrl Pts',(8.38627540352384,1.90988580729624,22.4942132651338));
#22562=CARTESIAN_POINT('Ctrl Pts',(8.19174495281671,-2.26688249514424,22.6927293825455));
#22563=CARTESIAN_POINT('Ctrl Pts',(4.57652150231426,-4.36767501203749,22.8912454999571));
#22564=CARTESIAN_POINT('Ctrl Pts',(0.851353342793238,-2.46864902413938,
23.0897616173688));
#22565=CARTESIAN_POINT('Ctrl Pts',(0.42768739434844,1.69114792223732,23.2882777347804));
#22566=CARTESIAN_POINT('Ctrl Pts',(3.69349202933814,4.30216786317793,23.4867938521921));
#22567=CARTESIAN_POINT('Ctrl Pts',(7.65803780123451,2.9734515702302,23.6853099696038));
#22568=CARTESIAN_POINT('Ctrl Pts',(8.6906071069521,-1.07850088950778,23.8838260870154));
#22569=CARTESIAN_POINT('Ctrl Pts',(5.84571156354535,-4.14238794997599,24.0823422044271));
#22570=CARTESIAN_POINT('Ctrl Pts',(1.7284241969769,-3.41351242146536,24.2808583218387));
#22571=CARTESIAN_POINT('Ctrl Pts',(0.109716235810993,0.442846747958131,
24.4793744392504));
#22572=CARTESIAN_POINT('Ctrl Pts',(2.47112996587446,3.89086027970496,24.677890556662));
#22573=CARTESIAN_POINT('Ctrl Pts',(6.6517366226307,3.78111221715306,24.8764066740737));
#22574=CARTESIAN_POINT('Ctrl Pts',(8.82041412666913,0.197058426719993,25.0749656474274));
#22575=CARTESIAN_POINT('Ctrl Pts',(7.60321109049825,-2.29676940207044,25.2073525816438));
#22576=CARTESIAN_POINT('Ctrl Pts',(6.60115576990582,-3.01054754622974,25.273567476723));
#22577=CARTESIAN_POINT('Ctrl Pts',(6.20648120676596,3.5255164385887,0.00171096560382468));
#22578=CARTESIAN_POINT('Ctrl Pts',(7.37912772202248,2.94343275606714,0.0678830047410433));
#22579=CARTESIAN_POINT('Ctrl Pts',(9.07759664569311,0.527144320628084,0.200227083015481));
#22580=CARTESIAN_POINT('Ctrl Pts',(7.40162371335757,-3.60564141759996,0.398743200427137));
#22581=CARTESIAN_POINT('Ctrl Pts',(3.02458781445768,-4.42536858002973,0.597259317838794));
#22582=CARTESIAN_POINT('Ctrl Pts',(-0.0391348072720899,-1.19794185424409,
0.795775435250448));
#22583=CARTESIAN_POINT('Ctrl Pts',(1.01307994788347,3.12938294858669,0.994291552662105));
#22584=CARTESIAN_POINT('Ctrl Pts',(5.21923250695947,4.58939821694615,1.19280767007376));
#22585=CARTESIAN_POINT('Ctrl Pts',(8.72657551299543,1.84730106611042,1.39132378748542));
#22586=CARTESIAN_POINT('Ctrl Pts',(8.32358502229467,-2.58692118447061,1.58983990489707));
#22587=CARTESIAN_POINT('Ctrl Pts',(4.37908581601258,-4.65188073047965,1.78835602230873));
#22588=CARTESIAN_POINT('Ctrl Pts',(0.505493161016087,-2.45684558601761,
1.98687213972038));
#22589=CARTESIAN_POINT('Ctrl Pts',(0.250108060020668,1.98817892786946,2.18538825713204));
#22590=CARTESIAN_POINT('Ctrl Pts',(3.8468393694429,4.61243733220712,2.38390437454369));
#22591=CARTESIAN_POINT('Ctrl Pts',(8.0018522734089,3.01272882884126,2.58242049195535));
#22592=CARTESIAN_POINT('Ctrl Pts',(8.91007369571349,-1.34598748780205,2.78093660936701));
#22593=CARTESIAN_POINT('Ctrl Pts',(5.73976719690925,-4.47206986535408,2.97945272677866));
#22594=CARTESIAN_POINT('Ctrl Pts',(1.39424152787623,-3.50271791779653,3.17796884419032));
#22595=CARTESIAN_POINT('Ctrl Pts',(-0.146954797017362,0.674357611516781,
3.37648496160198));
#22596=CARTESIAN_POINT('Ctrl Pts',(2.5275771424141,4.23386867290823,3.57500107901363));
#22597=CARTESIAN_POINT('Ctrl Pts',(6.96855153613195,3.91608365047424,3.77351719642529));
#22598=CARTESIAN_POINT('Ctrl Pts',(9.10900868522111,0.0120235511094912,
3.97203331383693));
#22599=CARTESIAN_POINT('Ctrl Pts',(6.98875855737045,-3.90304740339865,4.17054943124861));
#22600=CARTESIAN_POINT('Ctrl Pts',(2.54948593565754,-4.24378183362265,4.36906554866025));
#22601=CARTESIAN_POINT('Ctrl Pts',(-0.143407781592193,-0.698141563015474,
4.56758166607191));
#22602=CARTESIAN_POINT('Ctrl Pts',(1.37617826049345,3.48684345900968,4.76609778348356));
#22603=CARTESIAN_POINT('Ctrl Pts',(5.71663606344787,4.47864357428809,4.96461390089523));
#22604=CARTESIAN_POINT('Ctrl Pts',(8.90305693908813,1.36898709382619,5.16313001830687));
#22605=CARTESIAN_POINT('Ctrl Pts',(8.01737725983028,-2.99436172457643,5.36164613571854));
#22606=CARTESIAN_POINT('Ctrl Pts',(3.87068562947579,-4.61553103529222,5.56016225313019));
#22607=CARTESIAN_POINT('Ctrl Pts',(0.260443364168955,-2.00988482013811,
5.75867837054185));
#22608=CARTESIAN_POINT('Ctrl Pts',(0.492841656646439,2.436375680996,5.95719448795349));
#22609=CARTESIAN_POINT('Ctrl Pts',(4.35505457120696,4.6514496783783,6.15571060536516));
#22610=CARTESIAN_POINT('Ctrl Pts',(8.31014098784587,2.60681454019155,6.35422672277681));
#22611=CARTESIAN_POINT('Ctrl Pts',(8.73610799988966,-1.82509176699825,6.55274284018847));
#22612=CARTESIAN_POINT('Ctrl Pts',(5.24286312047947,-4.58561375091533,6.75125895760012));
#22613=CARTESIAN_POINT('Ctrl Pts',(1.02945356160573,-3.14671788935761,6.94977507501179));
#22614=CARTESIAN_POINT('Ctrl Pts',(-0.0455603502579819,1.17388235834786,
7.14829119242343));
#22615=CARTESIAN_POINT('Ctrl Pts',(3.00229867643747,4.41946347189101,7.34680730983509));
#22616=CARTESIAN_POINT('Ctrl Pts',(7.38185932147204,3.61778400498435,7.54532342724674));
#22617=CARTESIAN_POINT('Ctrl Pts',(9.08240325419932,-0.496993236137507,
7.7438395446584));
#22618=CARTESIAN_POINT('Ctrl Pts',(6.5466046888036,-4.15663352541875,7.94235566207006));
#22619=CARTESIAN_POINT('Ctrl Pts',(2.09669971547073,-4.00970789967487,8.1408717794817));
#22620=CARTESIAN_POINT('Ctrl Pts',(-0.192173337388976,-0.19076805214061,
8.33938789689338));
#22621=CARTESIAN_POINT('Ctrl Pts',(1.77609193305126,3.80287354875093,8.53790401430502));
#22622=CARTESIAN_POINT('Ctrl Pts',(6.1989956324977,4.3139158920216,8.73642013171668));
#22623=CARTESIAN_POINT('Ctrl Pts',(9.0261266855466,0.874356120760312,8.93493624912834));
#22624=CARTESIAN_POINT('Ctrl Pts',(7.66845225155073,-3.36592235387631,9.13345236653999));
#22625=CARTESIAN_POINT('Ctrl Pts',(3.36930475145732,-4.52375316346519,9.33196848395166));
#22626=CARTESIAN_POINT('Ctrl Pts',(0.0657616873951493,-1.53881687686219,
9.53048460136329));
#22627=CARTESIAN_POINT('Ctrl Pts',(0.783144957380055,2.85533863417045,9.72900071877498));
#22628=CARTESIAN_POINT('Ctrl Pts',(4.86448860883662,4.63462933832978,9.92751683618659));
#22629=CARTESIAN_POINT('Ctrl Pts',(8.57217576114917,2.16961465444475,10.1260329535983));
#22630=CARTESIAN_POINT('Ctrl Pts',(8.51077704791793,-2.28229185953398,10.3245490710099));
#22631=CARTESIAN_POINT('Ctrl Pts',(4.73652024279266,-4.644118902346,10.5230651884216));
#22632=CARTESIAN_POINT('Ctrl Pts',(0.705797933930029,-2.75295019489822,
10.7215813058332));
#22633=CARTESIAN_POINT('Ctrl Pts',(0.109868939318185,1.65931793437198,10.9200974232449));
#22634=CARTESIAN_POINT('Ctrl Pts',(3.49447369645122,4.55201426291826,11.1186135406565));
#22635=CARTESIAN_POINT('Ctrl Pts',(7.76005555075585,3.27606251797663,11.3171296580682));
#22636=CARTESIAN_POINT('Ctrl Pts',(9.00027578003045,-1.00004496361109,11.5156457754798));
#22637=CARTESIAN_POINT('Ctrl Pts',(6.07936428979557,-4.36033029039609,11.7141618928915));
#22638=CARTESIAN_POINT('Ctrl Pts',(1.67223626118035,-3.72750807951321,11.9126780103032));
#22639=CARTESIAN_POINT('Ctrl Pts',(-0.185144289673645,0.31889512586586,
12.1111941277148));
#22640=CARTESIAN_POINT('Ctrl Pts',(2.20817641458127,4.07326024100545,12.3097102451265));
#22641=CARTESIAN_POINT('Ctrl Pts',(6.66044079877556,4.09741110905781,12.5082263625381));
#22642=CARTESIAN_POINT('Ctrl Pts',(9.09434983091284,0.369230824458725,12.7067424799498));
#22643=CARTESIAN_POINT('Ctrl Pts',(7.28097591722075,-3.69708402566464,12.9052585973614));
#22644=CARTESIAN_POINT('Ctrl Pts',(2.8809723938291,-4.37767965107946,13.1037747147731));
#22645=CARTESIAN_POINT('Ctrl Pts',(-0.0762212094817758,-1.04927952433239,
13.3022908321848));
#22646=CARTESIAN_POINT('Ctrl Pts',(1.11753675741321,3.24003083138531,13.5008069495964));
#22647=CARTESIAN_POINT('Ctrl Pts',(5.369025456116,4.5621825836419,13.6993230670081));
#22648=CARTESIAN_POINT('Ctrl Pts',(8.78481240824481,1.70637430771384,13.8978391844197));
#22649=CARTESIAN_POINT('Ctrl Pts',(8.23678489819753,-2.71209910053747,14.0963553018314));
#22650=CARTESIAN_POINT('Ctrl Pts',(4.22681609508684,-4.64688374211174,14.294871419243));
#22651=CARTESIAN_POINT('Ctrl Pts',(0.427159151106815,-2.32614064576156,
14.4933875366547));
#22652=CARTESIAN_POINT('Ctrl Pts',(0.317467618415429,2.12483780609018,14.6919036540663));
#22653=CARTESIAN_POINT('Ctrl Pts',(3.99819491609722,4.62993021382537,14.890419771478));
#22654=CARTESIAN_POINT('Ctrl Pts',(8.09860099979244,2.8950206023505,15.0889358888896));
#22655=CARTESIAN_POINT('Ctrl Pts',(8.86361197604717,-1.49109380762589,15.2874520063013));
#22656=CARTESIAN_POINT('Ctrl Pts',(5.59264534485911,-4.5116928721902,15.485968123713));
#22657=CARTESIAN_POINT('Ctrl Pts',(1.2811901266875,-3.40056942590122,15.6844842411246));
#22658=CARTESIAN_POINT('Ctrl Pts',(-0.122405002240585,0.824730814938715,
15.8830003585363));
#22659=CARTESIAN_POINT('Ctrl Pts',(2.66724567793686,4.29475826350135,16.0815164759479));
#22660=CARTESIAN_POINT('Ctrl Pts',(7.09543313909595,3.83172778931411,16.2800325933596));
#22661=CARTESIAN_POINT('Ctrl Pts',(9.10690753736432,-0.140326107135887,
16.4785487107712));
#22662=CARTESIAN_POINT('Ctrl Pts',(6.85959888110794,-3.98387202395643,16.6770648281829));
#22663=CARTESIAN_POINT('Ctrl Pts',(2.41154968938301,-4.179063722519,16.8755809455945));
#22664=CARTESIAN_POINT('Ctrl Pts',(-0.163801198896094,-0.547148358219792,
17.0740970630062));
#22665=CARTESIAN_POINT('Ctrl Pts',(1.49200357138825,3.5858350646717,17.2726131804178));
#22666=CARTESIAN_POINT('Ctrl Pts',(5.86260948835618,4.43497894515246,17.4711292978295));
#22667=CARTESIAN_POINT('Ctrl Pts',(8.94549879098837,1.22265346990726,17.6696454152412));
#22668=CARTESIAN_POINT('Ctrl Pts',(7.91742009870712,-3.10935479574357,17.8681615326528));
#22669=CARTESIAN_POINT('Ctrl Pts',(3.71986832177296,-4.59387508565289,18.0666776500645));
#22670=CARTESIAN_POINT('Ctrl Pts',(0.196881531601468,-1.87141195688986,
18.2651937674761));
#22671=CARTESIAN_POINT('Ctrl Pts',(0.574744016316265,2.56485464396025,18.4637098848878));
#22672=CARTESIAN_POINT('Ctrl Pts',(4.50741650012369,4.6522761505852,18.6622260022994));
#22673=CARTESIAN_POINT('Ctrl Pts',(8.3934323297128,2.47923165417059,18.8607421197111));
#22674=CARTESIAN_POINT('Ctrl Pts',(8.67405212821057,-1.96424603112833,19.0592582371228));
#22675=CARTESIAN_POINT('Ctrl Pts',(5.09228962209667,-4.60890456507674,19.2577743545344));
#22676=CARTESIAN_POINT('Ctrl Pts',(0.928254782143413,-3.0328159689208,19.4562904719461));
#22677=CARTESIAN_POINT('Ctrl Pts',(-0.00470849360073685,1.32066780116548,
19.6548065893577));
#22678=CARTESIAN_POINT('Ctrl Pts',(3.14778981602278,4.46470912096001,19.8533227067694));
#22679=CARTESIAN_POINT('Ctrl Pts',(7.49875172579254,3.52005475507203,20.051838824181));
#22680=CARTESIAN_POINT('Ctrl Pts',(9.06364908309027,-0.648198796048447,
20.2503549415927));
#22681=CARTESIAN_POINT('Ctrl Pts',(6.4093786550744,-4.22284422156345,20.4488710590044));
#22682=CARTESIAN_POINT('Ctrl Pts',(1.96667081116617,-3.93028923259476,20.647387176416));
#22683=CARTESIAN_POINT('Ctrl Pts',(-0.195927116407106,-0.0384501329489085,
20.8459032938277));
#22684=CARTESIAN_POINT('Ctrl Pts',(1.90205092121151,3.88860087953163,21.0444194112393));
#22685=CARTESIAN_POINT('Ctrl Pts',(6.3393165377314,4.25454515162759,21.242935528651));
#22686=CARTESIAN_POINT('Ctrl Pts',(9.05230630112455,0.724257949825445,21.4414516460626));
#22687=CARTESIAN_POINT('Ctrl Pts',(7.55651576606266,-3.46929099370176,21.6399677634743));
#22688=CARTESIAN_POINT('Ctrl Pts',(3.22176150253947,-4.48572906904549,21.838483880886));
#22689=CARTESIAN_POINT('Ctrl Pts',(0.0177289115966501,-1.39422211492368,
22.0369999982976));
#22690=CARTESIAN_POINT('Ctrl Pts',(0.878610280341868,2.97408755340353,22.2355161157093));
#22691=CARTESIAN_POINT('Ctrl Pts',(5.01602646728549,4.61878321962123,22.4340322331209));
#22692=CARTESIAN_POINT('Ctrl Pts',(8.64101112050298,2.03368736229999,22.6325483505326));
#22693=CARTESIAN_POINT('Ctrl Pts',(8.43387092517075,-2.41382509078919,22.8310644679442));
#22694=CARTESIAN_POINT('Ctrl Pts',(4.58430347192829,-4.65079401118156,23.0295805853559));
#22695=CARTESIAN_POINT('Ctrl Pts',(0.617664534920323,-2.6286704174496,23.2280967027675));
#22696=CARTESIAN_POINT('Ctrl Pts',(0.166535948123391,1.80077057177711,23.4266128201792));
#22697=CARTESIAN_POINT('Ctrl Pts',(3.64403475383551,4.58104059437149,23.6251289375908));
#22698=CARTESIAN_POINT('Ctrl Pts',(7.86556810560143,3.16619499327494,23.8236450550025));
#22699=CARTESIAN_POINT('Ctrl Pts',(8.96507004425898,-1.14841087401253,24.0221611724142));
#22700=CARTESIAN_POINT('Ctrl Pts',(5.93576426504054,-4.41090351654891,24.2206772898258));
#22701=CARTESIAN_POINT('Ctrl Pts',(1.55158838794904,-3.63478122412758,24.4191934072375));
#22702=CARTESIAN_POINT('Ctrl Pts',(-0.172046559910909,0.471552713422697,
24.6177095246491));
#22703=CARTESIAN_POINT('Ctrl Pts',(2.34243741690352,4.14307145960353,24.8162256420608));
#22704=CARTESIAN_POINT('Ctrl Pts',(6.79403703197597,4.02620936921257,25.0147417594724));
#22705=CARTESIAN_POINT('Ctrl Pts',(9.10329134237422,0.209832038399488,25.2133007328261));
#22706=CARTESIAN_POINT('Ctrl Pts',(7.80718744833136,-2.44564931016495,25.3456876670425));
#22707=CARTESIAN_POINT('Ctrl Pts',(6.7401774553626,-3.20569558398784,25.4119025621217));
#22708=CARTESIAN_POINT('Ctrl Pts',(5.88688308661327,2.88166464694226,-0.413294290592403));
#22709=CARTESIAN_POINT('Ctrl Pts',(6.84537358445575,2.40588471549031,-0.347122251455184));
#22710=CARTESIAN_POINT('Ctrl Pts',(8.23365752427788,0.430873938343679,-0.214778173180747));
#22711=CARTESIAN_POINT('Ctrl Pts',(6.86376121760315,-2.94715670275194,-0.0162620557690901));
#22712=CARTESIAN_POINT('Ctrl Pts',(3.28608690294124,-3.61718018023642,0.182254061642566));
#22713=CARTESIAN_POINT('Ctrl Pts',(0.781880406995935,-0.979166244321737,
0.380770179054222));
#22714=CARTESIAN_POINT('Ctrl Pts',(1.64193314359211,2.55787552455616,0.579286296465875));
#22715=CARTESIAN_POINT('Ctrl Pts',(5.07993189931123,3.75125370222575,0.777802413877532));
#22716=CARTESIAN_POINT('Ctrl Pts',(7.94674205925474,1.50993542852403,0.976318531289188));
#22717=CARTESIAN_POINT('Ctrl Pts',(7.61734820438694,-2.11448150974993,1.17483464870084));
#22718=CARTESIAN_POINT('Ctrl Pts',(4.39321803491158,-3.80232526959411,1.3733507661125));
#22719=CARTESIAN_POINT('Ctrl Pts',(1.22704502026327,-2.0081611280352,1.57186688352415));
#22720=CARTESIAN_POINT('Ctrl Pts',(1.01829993859556,1.62508529687376,1.77038300093581));
#22721=CARTESIAN_POINT('Ctrl Pts',(3.95817375267475,3.77008527062174,1.96889911834747));
#22722=CARTESIAN_POINT('Ctrl Pts',(7.35437229592725,2.462525507432,2.16741523575912));
#22723=CARTESIAN_POINT('Ctrl Pts',(8.09672865983581,-1.10017486129741,2.36593135317078));
#22724=CARTESIAN_POINT('Ctrl Pts',(5.50540329893836,-3.65535258567839,2.56444747058243));
#22725=CARTESIAN_POINT('Ctrl Pts',(1.95348461951634,-2.8630297341532,2.76296358799409));
#22726=CARTESIAN_POINT('Ctrl Pts',(0.693751175975549,0.551202220257554,
2.96147970540574));
#22727=CARTESIAN_POINT('Ctrl Pts',(2.87984341841113,3.46065318004877,3.1599958228174));
#22728=CARTESIAN_POINT('Ctrl Pts',(6.50977938134639,3.20090403962421,3.35851194022905));
#22729=CARTESIAN_POINT('Ctrl Pts',(8.25933290131072,0.00982773524565914,
3.55702805764071));
#22730=CARTESIAN_POINT('Ctrl Pts',(6.52629607038668,-3.19024855326339,3.75554417505237));
#22731=CARTESIAN_POINT('Ctrl Pts',(2.89775109124319,-3.46875593755042,3.95406029246402));
#22732=CARTESIAN_POINT('Ctrl Pts',(0.69665041333009,-0.570642598253718,
4.15257640987568));
#22733=CARTESIAN_POINT('Ctrl Pts',(1.93872017863753,2.85005436799852,4.35109252728733));
#22734=CARTESIAN_POINT('Ctrl Pts',(5.48649651727959,3.66072576290342,4.54960864469899));
#22735=CARTESIAN_POINT('Ctrl Pts',(8.09099334705098,1.11897413587954,4.74812476211065));
#22736=CARTESIAN_POINT('Ctrl Pts',(7.36706201253862,-2.44751271825679,4.9466408795223));
#22737=CARTESIAN_POINT('Ctrl Pts',(3.97766506003213,-3.7726139823619,5.14515699693396));
#22738=CARTESIAN_POINT('Ctrl Pts',(1.02674774506536,-1.64282712377203,5.34367311434561));
#22739=CARTESIAN_POINT('Ctrl Pts',(1.21670401249677,1.99142956468722,5.54218923175727));
#22740=CARTESIAN_POINT('Ctrl Pts',(4.37357552585394,3.80197293891488,5.74070534916892));
#22741=CARTESIAN_POINT('Ctrl Pts',(7.60635940332531,2.13074181682499,5.93922146658058));
#22742=CARTESIAN_POINT('Ctrl Pts',(7.95453366396254,-1.49178213007847,6.13773758399224));
#22743=CARTESIAN_POINT('Ctrl Pts',(5.09924694286633,-3.74816037897555,6.33625370140389));
#22744=CARTESIAN_POINT('Ctrl Pts',(1.65531650589596,-2.57204465036969,6.53476981881556));
#22745=CARTESIAN_POINT('Ctrl Pts',(0.776628336729841,0.959500643563771,
6.7332859362272));
#22746=CARTESIAN_POINT('Ctrl Pts',(3.26786834626679,3.6123534997611,6.93180205363886));
#22747=CARTESIAN_POINT('Ctrl Pts',(6.84760632218384,2.95708173512582,7.1303181710505));
#22748=CARTESIAN_POINT('Ctrl Pts',(8.23758631997216,-0.406229232878139,
7.32883428846218));
#22749=CARTESIAN_POINT('Ctrl Pts',(6.16489109788061,-3.39752319671194,7.52735040587382));
#22750=CARTESIAN_POINT('Ctrl Pts',(2.52765551345678,-3.27743004474078,7.72586652328549));
#22751=CARTESIAN_POINT('Ctrl Pts',(0.656790727359,-0.155928801126063,7.92438264069713));
#22752=CARTESIAN_POINT('Ctrl Pts',(2.26559912307384,3.10836907247963,8.1228987581088));
#22753=CARTESIAN_POINT('Ctrl Pts',(5.88076457458627,3.52608167695778,8.32141487552045));
#22754=CARTESIAN_POINT('Ctrl Pts',(8.19158732913988,0.714675754863574,8.5199309929321));
#22755=CARTESIAN_POINT('Ctrl Pts',(7.08185986462416,-2.75121662896035,8.71844711034376));
#22756=CARTESIAN_POINT('Ctrl Pts',(3.56784948378791,-3.69759715767183,8.91696322775543));
#22757=CARTESIAN_POINT('Ctrl Pts',(0.867620049835816,-1.2577885451434,9.11547934516706));
#22758=CARTESIAN_POINT('Ctrl Pts',(1.45399031457103,2.33387889135228,9.31399546257875));
#22759=CARTESIAN_POINT('Ctrl Pts',(4.78997354349419,3.78822443423146,9.51251157999037));
#22760=CARTESIAN_POINT('Ctrl Pts',(7.8205397526871,1.77338609991104,9.71102769740205));
#22761=CARTESIAN_POINT('Ctrl Pts',(7.77035405525285,-1.8654854913274,9.90954381481369));
#22762=CARTESIAN_POINT('Ctrl Pts',(4.68537555826851,-3.79598095490491,10.1080599322253));
#22763=CARTESIAN_POINT('Ctrl Pts',(1.39076888675897,-2.25018926719472,10.306576049637));
#22764=CARTESIAN_POINT('Ctrl Pts',(0.903672160428571,1.35628294827392,10.5050921670486));
#22765=CARTESIAN_POINT('Ctrl Pts',(3.67015929568852,3.72069703895061,10.7036082844603));
#22766=CARTESIAN_POINT('Ctrl Pts',(7.156733998233,2.67776755651859,10.902124401872));
#22767=CARTESIAN_POINT('Ctrl Pts',(8.17045747715504,-0.817410517633158,
11.1006405192836));
#22768=CARTESIAN_POINT('Ctrl Pts',(5.78298105352307,-3.56401958853324,11.2991566366953));
#22769=CARTESIAN_POINT('Ctrl Pts',(2.18071022148213,-3.04676731509573,11.4976727541069));
#22770=CARTESIAN_POINT('Ctrl Pts',(0.662536086558379,0.260656509846819,
11.6961888715186));
#22771=CARTESIAN_POINT('Ctrl Pts',(2.61877364278075,3.32937606128419,11.8947049889302));
#22772=CARTESIAN_POINT('Ctrl Pts',(6.25793774774488,3.34911634724554,12.0932211063419));
#22773=CARTESIAN_POINT('Ctrl Pts',(8.24735113836601,0.301799589347462,12.2917372237535));
#22774=CARTESIAN_POINT('Ctrl Pts',(6.76514687416864,-3.02189949163811,12.4902533411652));
#22775=CARTESIAN_POINT('Ctrl Pts',(3.16869942579002,-3.57820050080496,12.6887694585768));
#22776=CARTESIAN_POINT('Ctrl Pts',(0.751566954770839,-0.857653555925328,
12.8872855759885));
#22777=CARTESIAN_POINT('Ctrl Pts',(1.72731339933552,2.64831620117018,13.0858016934002));
#22778=CARTESIAN_POINT('Ctrl Pts',(5.20236872621718,3.72900835754984,13.2843178108118));
#22779=CARTESIAN_POINT('Ctrl Pts',(7.99434336961907,1.39474559334568,13.4828339282235));
#22780=CARTESIAN_POINT('Ctrl Pts',(7.54640006010282,-2.21679865437008,13.6813500456351));
#22781=CARTESIAN_POINT('Ctrl Pts',(4.26875675973819,-3.79824086239538,13.8798661630468));
#22782=CARTESIAN_POINT('Ctrl Pts',(1.16301685561255,-1.9013263388412,14.0783822804584));
#22783=CARTESIAN_POINT('Ctrl Pts',(1.07335787448695,1.73678667876183,14.2768983978701));
#22784=CARTESIAN_POINT('Ctrl Pts',(4.08188780578152,3.78438349314049,14.4754145152818));
#22785=CARTESIAN_POINT('Ctrl Pts',(7.43345216672421,2.36631389110821,14.6739306326934));
#22786=CARTESIAN_POINT('Ctrl Pts',(8.05875206907788,-1.21878096033793,14.8724467501051));
#22787=CARTESIAN_POINT('Ctrl Pts',(5.38514975673243,-3.68773939197872,15.0709628675167));
#22788=CARTESIAN_POINT('Ctrl Pts',(1.86107937002522,-2.77953623668677,15.2694789849284));
#22789=CARTESIAN_POINT('Ctrl Pts',(0.713817534175901,0.674113331777405,
15.46799510234));
#22790=CARTESIAN_POINT('Ctrl Pts',(2.9940048152212,3.5104227339951,15.6665112197517));
#22791=CARTESIAN_POINT('Ctrl Pts',(6.61348907494099,3.13195377174095,15.8650273371633));
#22792=CARTESIAN_POINT('Ctrl Pts',(8.257615478175,-0.114698878595687,16.063543454575));
#22793=CARTESIAN_POINT('Ctrl Pts',(6.42072433944188,-3.25631247771842,16.2620595719866));
#22794=CARTESIAN_POINT('Ctrl Pts',(2.78500562221897,-3.41585705137789,16.4605756893983));
#22795=CARTESIAN_POINT('Ctrl Pts',(0.67998136903583,-0.447224713876356,
16.65909180681));
#22796=CARTESIAN_POINT('Ctrl Pts',(2.03339274915041,2.93096750947701,16.8576079242216));
#22797=CARTESIAN_POINT('Ctrl Pts',(5.60581136526813,3.62503544056518,17.0561240416333));
#22798=CARTESIAN_POINT('Ctrl Pts',(8.12568420335589,0.999364870669326,17.2546401590449));
#22799=CARTESIAN_POINT('Ctrl Pts',(7.28535965135699,-2.54150503784963,17.4531562764566));
#22800=CARTESIAN_POINT('Ctrl Pts',(3.85439094932391,-3.75491297725849,17.6516723938682));
#22801=CARTESIAN_POINT('Ctrl Pts',(0.974793970633971,-1.52964303811135,
17.8501885112799));
#22802=CARTESIAN_POINT('Ctrl Pts',(1.2836488526281,2.09644489844015,18.0487046286916));
#22803=CARTESIAN_POINT('Ctrl Pts',(4.49811216942012,3.80264847561477,18.2472207461032));
#22804=CARTESIAN_POINT('Ctrl Pts',(7.67443956106538,2.02645891285741,18.4457368635149));
#22805=CARTESIAN_POINT('Ctrl Pts',(7.90381082245328,-1.60552317494378,18.6442529809265));
#22806=CARTESIAN_POINT('Ctrl Pts',(4.9761721155001,-3.76719767944954,18.8427690983382));
#22807=CARTESIAN_POINT('Ctrl Pts',(1.57259927845708,-2.47894420875808,19.0412852157498));
#22808=CARTESIAN_POINT('Ctrl Pts',(0.810019572635768,1.07947921368855,19.2398013331615));
#22809=CARTESIAN_POINT('Ctrl Pts',(3.38678898688482,3.6493361063157,19.4383174505731));
#22810=CARTESIAN_POINT('Ctrl Pts',(6.94315110686829,2.87720041011993,19.6368335679848));
#22811=CARTESIAN_POINT('Ctrl Pts',(8.22225715251285,-0.529820690755693,
19.8353496853965));
#22812=CARTESIAN_POINT('Ctrl Pts',(6.05272613795891,-3.45164208273989,20.0338658028081));
#22813=CARTESIAN_POINT('Ctrl Pts',(2.42137329831411,-3.212515309774,20.2323819202198));
#22814=CARTESIAN_POINT('Ctrl Pts',(0.65372248686789,-0.0314281299545405,
20.4308980376314));
#22815=CARTESIAN_POINT('Ctrl Pts',(2.36855469553213,3.178440343651,20.6294141550431));
#22816=CARTESIAN_POINT('Ctrl Pts',(5.99545920128352,3.47755359131801,20.8279302724548));
#22817=CARTESIAN_POINT('Ctrl Pts',(8.21298586010566,0.591989447683331,21.0264463898664));
#22818=CARTESIAN_POINT('Ctrl Pts',(6.99036591797756,-2.83570744333498,21.2249625072781));
#22819=CARTESIAN_POINT('Ctrl Pts',(3.44725150283742,-3.6665172604341,21.4234786246897));
#22820=CARTESIAN_POINT('Ctrl Pts',(0.828359319011244,-1.13960058009792,
21.6219947421014));
#22821=CARTESIAN_POINT('Ctrl Pts',(1.53202116508044,2.43094114262164,21.820510859513));
#22822=CARTESIAN_POINT('Ctrl Pts',(4.91383661347899,3.77527223251319,22.0190269769247));
#22823=CARTESIAN_POINT('Ctrl Pts',(7.87680396956558,1.66228269728872,22.2175430943363));
#22824=CARTESIAN_POINT('Ctrl Pts',(7.7074930081086,-1.97299730385434,22.416059211748));
#22825=CARTESIAN_POINT('Ctrl Pts',(4.56095756308617,-3.80143701374933,22.6145753291597));
#22826=CARTESIAN_POINT('Ctrl Pts',(1.31873095853907,-2.14860623751896,22.8130914465713));
#22827=CARTESIAN_POINT('Ctrl Pts',(0.949990286798536,1.47190262315773,23.011607563983));
#22828=CARTESIAN_POINT('Ctrl Pts',(3.7924065803434,3.74442240079083,23.2101236813946));
#22829=CARTESIAN_POINT('Ctrl Pts',(7.24297719250067,2.58796472414074,23.4086397988063));
#22830=CARTESIAN_POINT('Ctrl Pts',(8.14168123233833,-0.938680920498277,
23.6071559162179));
#22831=CARTESIAN_POINT('Ctrl Pts',(5.66560616055497,-3.60535681683013,23.8056720336296));
#22832=CARTESIAN_POINT('Ctrl Pts',(2.08209581503262,-2.97097481614092,24.0041881510412));
#22833=CARTESIAN_POINT('Ctrl Pts',(0.673241827254791,0.385434817028999,
24.2027042684529));
#22834=CARTESIAN_POINT('Ctrl Pts',(2.72851506381635,3.38643791990783,24.4012203858645));
#22835=CARTESIAN_POINT('Ctrl Pts',(6.36713580394013,3.29091791303403,24.5997365032762));
#22836=CARTESIAN_POINT('Ctrl Pts',(8.25465969525897,0.17151120336101,24.7982954766299));
#22837=CARTESIAN_POINT('Ctrl Pts',(7.19525837483205,-1.99900958588141,24.9306824108463));
#22838=CARTESIAN_POINT('Ctrl Pts',(6.32311239899223,-2.62025147071356,24.9968973059255));
#22839=CARTESIAN_POINT('Ctrl Pts',(5.99341579333084,3.0962819108244,-0.27495920519366));
#22840=CARTESIAN_POINT('Ctrl Pts',(7.02329163031133,2.58506739568259,-0.208787166056442));
#22841=CARTESIAN_POINT('Ctrl Pts',(8.51497056474962,0.462964065771816,-0.0764430877820045));
#22842=CARTESIAN_POINT('Ctrl Pts',(7.04304871618797,-3.16665160770128,0.122073029629653));
#22843=CARTESIAN_POINT('Ctrl Pts',(3.19892054011338,-3.88657631350085,0.320589147041309));
#22844=CARTESIAN_POINT('Ctrl Pts',(0.508208668906595,-1.05209144762919,
0.519105264452963));
#22845=CARTESIAN_POINT('Ctrl Pts',(1.43231541168923,2.74837799923302,0.717621381864618));
#22846=CARTESIAN_POINT('Ctrl Pts',(5.12636543519397,4.03063520713254,0.916137499276276));
#22847=CARTESIAN_POINT('Ctrl Pts',(8.20668654383497,1.62239064105283,1.11465361668793));
#22848=CARTESIAN_POINT('Ctrl Pts',(7.85276047702285,-2.27196140132349,1.31316973409959));
#22849=CARTESIAN_POINT('Ctrl Pts',(4.38850729527858,-4.08551042322263,1.51168585151124));
#22850=CARTESIAN_POINT('Ctrl Pts',(0.986527733847538,-2.15772261402933,
1.7102019689229));
#22851=CARTESIAN_POINT('Ctrl Pts',(0.7622359790706,1.74611650720567,1.90871808633455));
#22852=CARTESIAN_POINT('Ctrl Pts',(3.92106229159746,4.0508692911502,2.10723420374621));
#22853=CARTESIAN_POINT('Ctrl Pts',(7.57019895508782,2.64592661456843,2.30575032115786));
#22854=CARTESIAN_POINT('Ctrl Pts',(8.36784367179503,-1.18211240346562,2.50426643856952));
#22855=CARTESIAN_POINT('Ctrl Pts',(5.58352459826198,-3.92759167890361,2.70278255598118));
#22856=CARTESIAN_POINT('Ctrl Pts',(1.7670702556363,-3.07625912870098,2.90129867339283));
#22857=CARTESIAN_POINT('Ctrl Pts',(0.413515851644582,0.592254017343965,
3.09981479080449));
#22858=CARTESIAN_POINT('Ctrl Pts',(2.76242132641212,3.7183916776686,3.29833090821614));
#22859=CARTESIAN_POINT('Ctrl Pts',(6.66270343294158,3.43929724324088,3.4968470256278));
#22860=CARTESIAN_POINT('Ctrl Pts',(8.54255816261418,0.0105596738669375,
3.69536314303945));
#22861=CARTESIAN_POINT('Ctrl Pts',(6.6804502327146,-3.42784816997514,3.89387926045112));
#22862=CARTESIAN_POINT('Ctrl Pts',(2.78166270604797,-3.72709790290783,4.09239537786277));
#22863=CARTESIAN_POINT('Ctrl Pts',(0.416631015022661,-0.613142253174304,
4.29091149527442));
#22864=CARTESIAN_POINT('Ctrl Pts',(1.75120620592284,3.06231739833558,4.48942761268608));
#22865=CARTESIAN_POINT('Ctrl Pts',(5.56320969933569,3.93336503336498,4.68794373009773));
#22866=CARTESIAN_POINT('Ctrl Pts',(8.36168121106336,1.20231178852842,4.88645984750939));
#22867=CARTESIAN_POINT('Ctrl Pts',(7.58383376163584,-2.62979572036334,5.08497596492104));
#22868=CARTESIAN_POINT('Ctrl Pts',(3.94200524984668,-4.05358633333867,5.2834920823327));
#22869=CARTESIAN_POINT('Ctrl Pts',(0.771312951433223,-1.76517968922739,
5.48200819974436));
#22870=CARTESIAN_POINT('Ctrl Pts',(0.97541656054666,2.13974493679014,5.68052431715601));
#22871=CARTESIAN_POINT('Ctrl Pts',(4.36740187430494,4.08513185206935,5.87904043456767));
#22872=CARTESIAN_POINT('Ctrl Pts',(7.84095326483218,2.28943272461384,6.07755655197932));
#22873=CARTESIAN_POINT('Ctrl Pts',(8.21505844260491,-1.60288534238506,6.27607266939098));
#22874=CARTESIAN_POINT('Ctrl Pts',(5.14711900207072,-4.02731150295548,6.47458878680263));
#22875=CARTESIAN_POINT('Ctrl Pts',(1.44669552446588,-2.76360239669899,6.6731049042143));
#22876=CARTESIAN_POINT('Ctrl Pts',(0.502565441067234,1.03096121515846,6.87162102162594));
#22877=CARTESIAN_POINT('Ctrl Pts',(3.17934512299035,3.88139015713774,7.07013713903761));
#22878=CARTESIAN_POINT('Ctrl Pts',(7.0256906552799,3.17731582507866,7.26865325644925));
#22879=CARTESIAN_POINT('Ctrl Pts',(8.51919196471455,-0.436483900631263,
7.46716937386092));
#22880=CARTESIAN_POINT('Ctrl Pts',(6.2921289615216,-3.65055997294754,7.66568549127257));
#22881=CARTESIAN_POINT('Ctrl Pts',(2.38400358079477,-3.52152266305215,7.86420160868423));
#22882=CARTESIAN_POINT('Ctrl Pts',(0.373802705776339,-0.16754188479758,
8.06271772609589));
#22883=CARTESIAN_POINT('Ctrl Pts',(2.10243005973299,3.33987056457006,8.26123384350753));
#22884=CARTESIAN_POINT('Ctrl Pts',(5.98684159389007,3.78869308197905,8.4597499609192));
#22885=CARTESIAN_POINT('Ctrl Pts',(8.4697671146088,0.767902543495819,8.65826607833084));
#22886=CARTESIAN_POINT('Ctrl Pts',(7.27739066026635,-2.95611853726567,8.85678219574251));
#22887=CARTESIAN_POINT('Ctrl Pts',(3.50166790634439,-3.97298249293629,9.05529831315416));
#22888=CARTESIAN_POINT('Ctrl Pts',(0.600333929022254,-1.35146465571633,
9.25381443056581));
#22889=CARTESIAN_POINT('Ctrl Pts',(1.23037519550738,2.50769880562501,9.45233054797748));
#22890=CARTESIAN_POINT('Ctrl Pts',(4.81481189860833,4.07035940226423,9.65084666538912));
#22891=CARTESIAN_POINT('Ctrl Pts',(8.07108508884113,1.90546228475562,9.84936278280079));
#22892=CARTESIAN_POINT('Ctrl Pts',(8.01716171947454,-2.00442094739626,10.0478789002124));
#22893=CARTESIAN_POINT('Ctrl Pts',(4.70242378644322,-4.07869360405195,10.2463950176241));
#22894=CARTESIAN_POINT('Ctrl Pts',(1.16244523581599,-2.41777624309588,10.4449111350357));
#22895=CARTESIAN_POINT('Ctrl Pts',(0.639071086725107,1.45729461030662,10.6434272524474));
#22896=CARTESIAN_POINT('Ctrl Pts',(3.61159742927608,3.99780278027315,10.841943369859));
#22897=CARTESIAN_POINT('Ctrl Pts',(7.35784118240728,2.87719921033794,11.0404594872707));
#22898=CARTESIAN_POINT('Ctrl Pts',(8.44706357811351,-0.878288666292467,
11.2389756046823));
#22899=CARTESIAN_POINT('Ctrl Pts',(5.88177546561389,-3.82945648915419,11.437491722094));
#22900=CARTESIAN_POINT('Ctrl Pts',(2.01121890138154,-3.27368090323489,11.6360078395057));
#22901=CARTESIAN_POINT('Ctrl Pts',(0.379975961147697,0.280069381853164,
11.8345239569173));
#22902=CARTESIAN_POINT('Ctrl Pts',(2.4819079000476,3.57733745452462,12.033040074329));
#22903=CARTESIAN_POINT('Ctrl Pts',(6.39210543142176,3.59854793451629,12.2315561917406));
#22904=CARTESIAN_POINT('Ctrl Pts',(8.52968403588164,0.324276667717884,12.4300723091523));
#22905=CARTESIAN_POINT('Ctrl Pts',(6.93708988851933,-3.24696100298028,12.6285884265639));
#22906=CARTESIAN_POINT('Ctrl Pts',(3.07279041513639,-3.84469355089646,12.8271045439756));
#22907=CARTESIAN_POINT('Ctrl Pts',(0.475637566686629,-0.921528878727684,
13.0256206613872));
#22908=CARTESIAN_POINT('Ctrl Pts',(1.52405451869475,2.84555441124189,13.2241367787989));
#22909=CARTESIAN_POINT('Ctrl Pts',(5.25792096951678,4.00673309958052,13.4226528962106));
#22910=CARTESIAN_POINT('Ctrl Pts',(8.257833049161,1.4986218314684,13.6211690136222));
#22911=CARTESIAN_POINT('Ctrl Pts',(7.77652833946771,-2.38189880309254,13.8196851310339));
#22912=CARTESIAN_POINT('Ctrl Pts',(4.25477653818775,-4.08112182230083,14.0182012484455));
#22913=CARTESIAN_POINT('Ctrl Pts',(0.917730954110628,-2.04293110781465,
14.2167173658572));
#22914=CARTESIAN_POINT('Ctrl Pts',(0.821394455796449,1.86613705453794,14.4152334832688));
#22915=CARTESIAN_POINT('Ctrl Pts',(4.05399017588675,4.06623240003544,14.6137496006805));
#22916=CARTESIAN_POINT('Ctrl Pts',(7.65516844441363,2.54254946152231,14.8122657180922));
#22917=CARTESIAN_POINT('Ctrl Pts',(8.32703870473431,-1.30955190943392,15.0107818355038));
#22918=CARTESIAN_POINT('Ctrl Pts',(5.45431495277465,-3.96239055204922,15.2092979529155));
#22919=CARTESIAN_POINT('Ctrl Pts',(1.66778295557931,-2.98654729975826,15.4078140703271));
#22920=CARTESIAN_POINT('Ctrl Pts',(0.435076688703739,0.724319159497842,
15.6063301877388));
#22921=CARTESIAN_POINT('Ctrl Pts',(2.88508510279309,3.77186791049719,15.8048463051504));
#22922=CARTESIAN_POINT('Ctrl Pts',(6.77413709632598,3.36521177759866,16.0033624225621));
#22923=CARTESIAN_POINT('Ctrl Pts',(8.54071283123811,-0.123241288109086,
16.2018785399737));
#22924=CARTESIAN_POINT('Ctrl Pts',(6.56701585333057,-3.49883232646441,16.4003946573854));
#22925=CARTESIAN_POINT('Ctrl Pts',(2.66052031127365,-3.67025927509159,16.598910774797));
#22926=CARTESIAN_POINT('Ctrl Pts',(0.398720513058523,-0.480532595324168,
16.7974268922087));
#22927=CARTESIAN_POINT('Ctrl Pts',(1.85292968989636,3.14925669454191,16.9959430096203));
#22928=CARTESIAN_POINT('Ctrl Pts',(5.69141073963082,3.89501660876095,17.194459127032));
#22929=CARTESIAN_POINT('Ctrl Pts',(8.39895573256671,1.07379440374864,17.3929752444437));
#22930=CARTESIAN_POINT('Ctrl Pts',(7.49604646714037,-2.73078829048094,17.5914913618553));
#22931=CARTESIAN_POINT('Ctrl Pts',(3.80955007347359,-4.03456701338995,17.790007479267));
#22932=CARTESIAN_POINT('Ctrl Pts',(0.715489824289806,-1.64356601103751,
17.9885235966786));
#22933=CARTESIAN_POINT('Ctrl Pts',(1.04734724052415,2.25258148028018,18.1870397140903));
#22934=CARTESIAN_POINT('Ctrl Pts',(4.50121361298798,4.08585770060491,18.3855558315019));
#22935=CARTESIAN_POINT('Ctrl Pts',(7.91410381728119,2.1773831599618,18.5840719489136));
#22936=CARTESIAN_POINT('Ctrl Pts',(8.16055792437237,-1.72509746033864,18.7825880663253));
#22937=CARTESIAN_POINT('Ctrl Pts',(5.0148779510323,-4.04776664132528,18.9811041837369));
#22938=CARTESIAN_POINT('Ctrl Pts',(1.35781777968586,-2.66356812881232,19.1796203011486));
#22939=CARTESIAN_POINT('Ctrl Pts',(0.538443550556935,1.1598754095142,19.3781364185603));
#22940=CARTESIAN_POINT('Ctrl Pts',(3.30712259659747,3.92112711119714,19.5766525359719));
#22941=CARTESIAN_POINT('Ctrl Pts',(7.12835131317638,3.09148519177063,19.7751686533836));
#22942=CARTESIAN_POINT('Ctrl Pts',(8.50272112937199,-0.569280059186615,
19.9736847707952));
#22943=CARTESIAN_POINT('Ctrl Pts',(6.17161031033075,-3.70870946234774,20.1722008882069));
#22944=CARTESIAN_POINT('Ctrl Pts',(2.26980580259814,-3.45177328404759,20.3707170056185));
#22945=CARTESIAN_POINT('Ctrl Pts',(0.370505952442893,-0.0337687976193256,
20.5692331230302));
#22946=CARTESIAN_POINT('Ctrl Pts',(2.21305343742525,3.41516052227788,20.7677492404418));
#22947=CARTESIAN_POINT('Ctrl Pts',(6.11007831343283,3.73655077808788,20.9662653578534));
#22948=CARTESIAN_POINT('Ctrl Pts',(8.49275934044528,0.636078948397367,21.1647814752652));
#22949=CARTESIAN_POINT('Ctrl Pts',(7.17908253400595,-3.04690196012391,21.3632975926768));
#22950=CARTESIAN_POINT('Ctrl Pts',(3.37208816940477,-3.93958786330456,21.5618137100885));
#22951=CARTESIAN_POINT('Ctrl Pts',(0.558149183206385,-1.22447442503984,
21.7603298275001));
#22952=CARTESIAN_POINT('Ctrl Pts',(1.31421753683424,2.61198994621562,21.9588459449118));
#22953=CARTESIAN_POINT('Ctrl Pts',(4.94789989808116,4.05644256154919,22.1573620623234));
#22954=CARTESIAN_POINT('Ctrl Pts',(8.13153968654471,1.78608425229248,22.3558781797351));
#22955=CARTESIAN_POINT('Ctrl Pts',(7.94961898046267,-2.11993989949929,22.5543942971467));
#22956=CARTESIAN_POINT('Ctrl Pts',(4.56873953270021,-4.0845560128934,22.7529104145584));
#22957=CARTESIAN_POINT('Ctrl Pts',(1.08504215066615,-2.30862763082918,22.95142653197));
#22958=CARTESIAN_POINT('Ctrl Pts',(0.688838840573486,1.58152527269752,23.1499426493817));
#22959=CARTESIAN_POINT('Ctrl Pts',(3.74294930484078,4.02329513198439,23.3484587667933));
#22960=CARTESIAN_POINT('Ctrl Pts',(7.45050749686758,2.78070814718547,23.546974884205));
#22961=CARTESIAN_POINT('Ctrl Pts',(8.41614416964521,-1.00859090500303,23.7454910016166));
#22962=CARTESIAN_POINT('Ctrl Pts',(5.75565886205016,-3.87387238340306,23.9440071190283));
#22963=CARTESIAN_POINT('Ctrl Pts',(1.90526000600476,-3.19224361880315,24.14252323644));
#22964=CARTESIAN_POINT('Ctrl Pts',(0.391479031532891,0.414140782493564,
24.3410393538516));
#22965=CARTESIAN_POINT('Ctrl Pts',(2.59982251484541,3.6386490998064,24.5395554712633));
#22966=CARTESIAN_POINT('Ctrl Pts',(6.50943621328541,3.53601506509354,24.7380715886749));
#22967=CARTESIAN_POINT('Ctrl Pts',(8.53753691096405,0.184284815040506,24.9366305620286));
#22968=CARTESIAN_POINT('Ctrl Pts',(7.39923473266516,-2.14788949397592,25.069017496245));
#22969=CARTESIAN_POINT('Ctrl Pts',(6.46213408444902,-2.81539950847165,25.1352323913243));
#22970=CARTESIAN_POINT('Ctrl Pts',(6.0999485000484,3.31089917470656,-0.136624119794918));
#22971=CARTESIAN_POINT('Ctrl Pts',(7.2012096761669,2.76425007587486,-0.0704520806576993));
#22972=CARTESIAN_POINT('Ctrl Pts',(8.79628360522135,0.495054193199949,0.061891997616738));
#22973=CARTESIAN_POINT('Ctrl Pts',(7.22233621477278,-3.38614651265062,0.260408115028396));
#22974=CARTESIAN_POINT('Ctrl Pts',(3.11175417728552,-4.15597244676529,0.458924232440051));
#22975=CARTESIAN_POINT('Ctrl Pts',(0.234536930817258,-1.12501665093665,
0.657440349851707));
#22976=CARTESIAN_POINT('Ctrl Pts',(1.22269767978634,2.93888047390986,0.855956467263361));
#22977=CARTESIAN_POINT('Ctrl Pts',(5.17279897107673,4.31001671203934,1.05447258467502));
#22978=CARTESIAN_POINT('Ctrl Pts',(8.46663102841521,1.73484585358162,1.25298870208667));
#22979=CARTESIAN_POINT('Ctrl Pts',(8.08817274965877,-2.42944129289705,1.45150481949833));
#22980=CARTESIAN_POINT('Ctrl Pts',(4.38379655564558,-4.36869557685114,1.65002093690999));
#22981=CARTESIAN_POINT('Ctrl Pts',(0.746010447431816,-2.30728410002347,
1.84853705432164));
#22982=CARTESIAN_POINT('Ctrl Pts',(0.506172019545635,1.86714771753756,2.04705317173329));
#22983=CARTESIAN_POINT('Ctrl Pts',(3.88395083052018,4.33165331167866,2.24556928914495));
#22984=CARTESIAN_POINT('Ctrl Pts',(7.78602561424836,2.82932772170484,2.4440854065566));
#22985=CARTESIAN_POINT('Ctrl Pts',(8.63895868375428,-1.26404994563383,2.64260152396827));
#22986=CARTESIAN_POINT('Ctrl Pts',(5.66164589758561,-4.19983077212884,2.84111764137992));
#22987=CARTESIAN_POINT('Ctrl Pts',(1.58065589175627,-3.28948852324876,3.03963375879158));
#22988=CARTESIAN_POINT('Ctrl Pts',(0.133280527313607,0.633305814430374,
3.23814987620323));
#22989=CARTESIAN_POINT('Ctrl Pts',(2.6449992344131,3.97613017528841,3.43666599361489));
#22990=CARTESIAN_POINT('Ctrl Pts',(6.81562748453676,3.67769044685756,3.63518211102655));
#22991=CARTESIAN_POINT('Ctrl Pts',(8.82578342391765,0.0112916124882134,
3.8336982284382));
#22992=CARTESIAN_POINT('Ctrl Pts',(6.83460439504253,-3.66544778668689,4.03221434584986));
#22993=CARTESIAN_POINT('Ctrl Pts',(2.66557432085276,-3.98543986826524,4.23073046326151));
#22994=CARTESIAN_POINT('Ctrl Pts',(0.13661161671523,-0.655641908094887,
4.42924658067317));
#22995=CARTESIAN_POINT('Ctrl Pts',(1.56369223320815,3.27458042867263,4.62776269808482));
#22996=CARTESIAN_POINT('Ctrl Pts',(5.63992288139177,4.20600430382654,4.82627881549648));
#22997=CARTESIAN_POINT('Ctrl Pts',(8.63236907507575,1.28564944117731,5.02479493290813));
#22998=CARTESIAN_POINT('Ctrl Pts',(7.80060551073305,-2.81207872246989,5.22331105031979));
#22999=CARTESIAN_POINT('Ctrl Pts',(3.90634543966123,-4.33455868431544,5.42182716773146));
#23000=CARTESIAN_POINT('Ctrl Pts',(0.515878157801087,-1.88753225468275,
5.62034328514309));
#23001=CARTESIAN_POINT('Ctrl Pts',(0.734129108596551,2.28806030889307,5.81885940255477));
#23002=CARTESIAN_POINT('Ctrl Pts',(4.36122822275595,4.36829076522382,6.0173755199664));
#23003=CARTESIAN_POINT('Ctrl Pts',(8.07554712633902,2.44812363240269,6.21589163737808));
#23004=CARTESIAN_POINT('Ctrl Pts',(8.47558322124728,-1.71398855469165,6.41440775478972));
#23005=CARTESIAN_POINT('Ctrl Pts',(5.19499106127511,-4.3064626269354,6.61292387220138));
#23006=CARTESIAN_POINT('Ctrl Pts',(1.2380745430358,-2.9551601430283,6.81143998961304));
#23007=CARTESIAN_POINT('Ctrl Pts',(0.228502545404632,1.10242178675316,7.00995610702469));
#23008=CARTESIAN_POINT('Ctrl Pts',(3.09082189971391,4.15042681451437,7.20847222443635));
#23009=CARTESIAN_POINT('Ctrl Pts',(7.20377498837598,3.39754991503151,7.406988341848));
#23010=CARTESIAN_POINT('Ctrl Pts',(8.80079760945692,-0.466738568384383,
7.60550445925966));
#23011=CARTESIAN_POINT('Ctrl Pts',(6.41936682516261,-3.90359674918315,7.80402057667131));
#23012=CARTESIAN_POINT('Ctrl Pts',(2.24035164813274,-3.7656152813635,8.00253669408298));
#23013=CARTESIAN_POINT('Ctrl Pts',(0.0908146841936848,-0.179154968469096,
8.20105281149462));
#23014=CARTESIAN_POINT('Ctrl Pts',(1.93926099639212,3.57137205666049,8.39956892890629));
#23015=CARTESIAN_POINT('Ctrl Pts',(6.09291861319388,4.05130448700034,8.59808504631793));
#23016=CARTESIAN_POINT('Ctrl Pts',(8.7479469000777,0.821129332128062,8.7966011637296));
#23017=CARTESIAN_POINT('Ctrl Pts',(7.47292145590854,-3.16102044557099,8.99511728114126));
#23018=CARTESIAN_POINT('Ctrl Pts',(3.43548632890085,-4.24836782820074,9.19363339855291));
#23019=CARTESIAN_POINT('Ctrl Pts',(0.333047808208697,-1.44514076628925,
9.39214951596456));
#23020=CARTESIAN_POINT('Ctrl Pts',(1.00676007644372,2.68151871989772,9.59066563337622));
#23021=CARTESIAN_POINT('Ctrl Pts',(4.83965025372247,4.352494370297,9.78918175078787));
#23022=CARTESIAN_POINT('Ctrl Pts',(8.32163042499515,2.03753846960017,9.98769786819953));
#23023=CARTESIAN_POINT('Ctrl Pts',(8.26396938369623,-2.14335640346512,10.1862139856111));
#23024=CARTESIAN_POINT('Ctrl Pts',(4.71947201461794,-4.36140625319899,10.3847301030228));
#23025=CARTESIAN_POINT('Ctrl Pts',(0.934121584873003,-2.58536321899705,
10.5832462204345));
#23026=CARTESIAN_POINT('Ctrl Pts',(0.37447001302165,1.5583062723393,10.7817623378461));
#23027=CARTESIAN_POINT('Ctrl Pts',(3.55303556286365,4.27490852159572,10.9802784552578));
#23028=CARTESIAN_POINT('Ctrl Pts',(7.55894836658157,3.07663086415728,11.1787945726694));
#23029=CARTESIAN_POINT('Ctrl Pts',(8.72366967907197,-0.939166814951776,
11.3773106900811));
#23030=CARTESIAN_POINT('Ctrl Pts',(5.98056987770475,-4.09489338977514,11.5758268074927));
#23031=CARTESIAN_POINT('Ctrl Pts',(1.84172758128094,-3.50059449137405,11.7743429249044));
#23032=CARTESIAN_POINT('Ctrl Pts',(0.0974158357370281,0.299482253859507,
11.9728590423161));
#23033=CARTESIAN_POINT('Ctrl Pts',(2.34504215731444,3.82529884776504,12.1713751597277));
#23034=CARTESIAN_POINT('Ctrl Pts',(6.52627311509865,3.84797952178704,12.3698912771394));
#23035=CARTESIAN_POINT('Ctrl Pts',(8.81201693339725,0.346753746088307,12.568407394551));
#23036=CARTESIAN_POINT('Ctrl Pts',(7.10903290287004,-3.47202251432246,12.7669235119627));
#23037=CARTESIAN_POINT('Ctrl Pts',(2.97688140448274,-4.11118660098796,12.9654396293744));
#23038=CARTESIAN_POINT('Ctrl Pts',(0.199708178602426,-0.985404201530036,
13.163955746786));
#23039=CARTESIAN_POINT('Ctrl Pts',(1.32079563805398,3.0427926213136,13.3624718641977));
#23040=CARTESIAN_POINT('Ctrl Pts',(5.3134732128164,4.28445784161121,13.5609879816093));
#23041=CARTESIAN_POINT('Ctrl Pts',(8.52132272870291,1.60249806959112,13.759504099021));
#23042=CARTESIAN_POINT('Ctrl Pts',(8.00665661883263,-2.546998951815,13.9580202164326));
#23043=CARTESIAN_POINT('Ctrl Pts',(4.24079631663729,-4.36400278220629,14.1565363338443));
#23044=CARTESIAN_POINT('Ctrl Pts',(0.672445052608722,-2.18453587678811,
14.3550524512559));
#23045=CARTESIAN_POINT('Ctrl Pts',(0.569431037105937,1.99548743031406,14.5535685686676));
#23046=CARTESIAN_POINT('Ctrl Pts',(4.02609254599198,4.3480813069304,14.7520846860792));
#23047=CARTESIAN_POINT('Ctrl Pts',(7.87688472210303,2.7187850319364,14.9506008034909));
#23048=CARTESIAN_POINT('Ctrl Pts',(8.59532534039074,-1.40032285852991,15.1491169209026));
#23049=CARTESIAN_POINT('Ctrl Pts',(5.52348014881688,-4.2370417121197,15.3476330383142));
#23050=CARTESIAN_POINT('Ctrl Pts',(1.47448654113341,-3.19355836282975,15.5461491557259));
#23051=CARTESIAN_POINT('Ctrl Pts',(0.156335843231577,0.774524987218279,
15.7446652731375));
#23052=CARTESIAN_POINT('Ctrl Pts',(2.77616539036498,4.03331308699926,15.9431813905492));
#23053=CARTESIAN_POINT('Ctrl Pts',(6.93478511771097,3.59846978345639,16.1416975079608));
#23054=CARTESIAN_POINT('Ctrl Pts',(8.82381018430121,-0.131783697622486,
16.3402136253725));
#23055=CARTESIAN_POINT('Ctrl Pts',(6.71330736721926,-3.74135217521042,16.5387297427841));
#23056=CARTESIAN_POINT('Ctrl Pts',(2.53603500032833,-3.92466149880528,16.7372458601958));
#23057=CARTESIAN_POINT('Ctrl Pts',(0.117459657081213,-0.513840476771981,
16.9357619776075));
#23058=CARTESIAN_POINT('Ctrl Pts',(1.6724666306423,3.3675458796068,17.1342780950191));
#23059=CARTESIAN_POINT('Ctrl Pts',(5.77701011399349,4.16499777695671,17.3327942124308));
#23060=CARTESIAN_POINT('Ctrl Pts',(8.67222726177754,1.14822393682795,17.5313103298424));
#23061=CARTESIAN_POINT('Ctrl Pts',(7.70673328292373,-2.92007154311226,17.7298264472541));
#23062=CARTESIAN_POINT('Ctrl Pts',(3.76470919762329,-4.31422104952143,17.9283425646657));
#23063=CARTESIAN_POINT('Ctrl Pts',(0.456185677945633,-1.75748898396369,
18.1268586820774));
#23064=CARTESIAN_POINT('Ctrl Pts',(0.811045628420214,2.40871806212022,18.3253747994891));
#23065=CARTESIAN_POINT('Ctrl Pts',(4.50431505655582,4.36906692559506,18.5238909169007));
#23066=CARTESIAN_POINT('Ctrl Pts',(8.153768073497,2.32830740706619,18.7224070343124));
#23067=CARTESIAN_POINT('Ctrl Pts',(8.41730502629147,-1.84467174573349,18.920923151724));
#23068=CARTESIAN_POINT('Ctrl Pts',(5.05358378656449,-4.328335603201,19.1194392691357));
#23069=CARTESIAN_POINT('Ctrl Pts',(1.14303628091464,-2.84819204886657,19.3179553865473));
#23070=CARTESIAN_POINT('Ctrl Pts',(0.266867528478102,1.24027160533984,19.516471503959));
#23071=CARTESIAN_POINT('Ctrl Pts',(3.22745620631011,4.19291811607857,19.7149876213706));
#23072=CARTESIAN_POINT('Ctrl Pts',(7.31355151948446,3.30576997342133,19.9135037387823));
#23073=CARTESIAN_POINT('Ctrl Pts',(8.78318510623113,-0.60873942761753,20.112019856194));
#23074=CARTESIAN_POINT('Ctrl Pts',(6.29049448270258,-3.96577684195559,20.3105359736056));
#23075=CARTESIAN_POINT('Ctrl Pts',(2.11823830688215,-3.69103125832118,20.5090520910173));
#23076=CARTESIAN_POINT('Ctrl Pts',(0.0872894180178925,-0.0361094652841183,
20.7075682084289));
#23077=CARTESIAN_POINT('Ctrl Pts',(2.05755217931839,3.65188070090475,20.9060843258406));
#23078=CARTESIAN_POINT('Ctrl Pts',(6.2246974255821,3.99554796485774,21.1046004432522));
#23079=CARTESIAN_POINT('Ctrl Pts',(8.77253282078492,0.680168449111409,21.3031165606639));
#23080=CARTESIAN_POINT('Ctrl Pts',(7.36779915003431,-3.25809647691284,21.5016326780756));
#23081=CARTESIAN_POINT('Ctrl Pts',(3.29692483597213,-4.21265846617502,21.7001487954872));
#23082=CARTESIAN_POINT('Ctrl Pts',(0.287939047401517,-1.30934826998177,
21.8986649128989));
#23083=CARTESIAN_POINT('Ctrl Pts',(1.09641390858805,2.79303874980958,22.0971810303105));
#23084=CARTESIAN_POINT('Ctrl Pts',(4.98196318268333,4.33761289058522,22.2956971477222));
#23085=CARTESIAN_POINT('Ctrl Pts',(8.38627540352384,1.90988580729624,22.4942132651338));
#23086=CARTESIAN_POINT('Ctrl Pts',(8.19174495281671,-2.26688249514424,22.6927293825455));
#23087=CARTESIAN_POINT('Ctrl Pts',(4.57652150231426,-4.36767501203749,22.8912454999571));
#23088=CARTESIAN_POINT('Ctrl Pts',(0.851353342793238,-2.46864902413938,
23.0897616173688));
#23089=CARTESIAN_POINT('Ctrl Pts',(0.42768739434844,1.69114792223732,23.2882777347804));
#23090=CARTESIAN_POINT('Ctrl Pts',(3.69349202933814,4.30216786317793,23.4867938521921));
#23091=CARTESIAN_POINT('Ctrl Pts',(7.65803780123451,2.9734515702302,23.6853099696038));
#23092=CARTESIAN_POINT('Ctrl Pts',(8.6906071069521,-1.07850088950778,23.8838260870154));
#23093=CARTESIAN_POINT('Ctrl Pts',(5.84571156354535,-4.14238794997599,24.0823422044271));
#23094=CARTESIAN_POINT('Ctrl Pts',(1.7284241969769,-3.41351242146536,24.2808583218387));
#23095=CARTESIAN_POINT('Ctrl Pts',(0.109716235810993,0.442846747958131,
24.4793744392504));
#23096=CARTESIAN_POINT('Ctrl Pts',(2.47112996587446,3.89086027970496,24.677890556662));
#23097=CARTESIAN_POINT('Ctrl Pts',(6.6517366226307,3.78111221715306,24.8764066740737));
#23098=CARTESIAN_POINT('Ctrl Pts',(8.82041412666913,0.197058426719993,25.0749656474274));
#23099=CARTESIAN_POINT('Ctrl Pts',(7.60321109049825,-2.29676940207044,25.2073525816438));
#23100=CARTESIAN_POINT('Ctrl Pts',(6.60115576990582,-3.01054754622974,25.273567476723));
#23101=CARTESIAN_POINT('Ctrl Pts',(6.20648120676596,3.5255164385887,0.00171096560382468));
#23102=CARTESIAN_POINT('Ctrl Pts',(7.37912772202248,2.94343275606714,0.0678830047410433));
#23103=CARTESIAN_POINT('Ctrl Pts',(9.07759664569311,0.527144320628084,0.200227083015481));
#23104=CARTESIAN_POINT('Ctrl Pts',(7.40162371335757,-3.60564141759996,0.398743200427137));
#23105=CARTESIAN_POINT('Ctrl Pts',(3.02458781445768,-4.42536858002973,0.597259317838794));
#23106=CARTESIAN_POINT('Ctrl Pts',(-0.0391348072720899,-1.19794185424409,
0.795775435250448));
#23107=CARTESIAN_POINT('Ctrl Pts',(1.01307994788347,3.12938294858669,0.994291552662105));
#23108=CARTESIAN_POINT('Ctrl Pts',(5.21923250695947,4.58939821694615,1.19280767007376));
#23109=CARTESIAN_POINT('Ctrl Pts',(8.72657551299543,1.84730106611042,1.39132378748542));
#23110=CARTESIAN_POINT('Ctrl Pts',(8.32358502229467,-2.58692118447061,1.58983990489707));
#23111=CARTESIAN_POINT('Ctrl Pts',(4.37908581601258,-4.65188073047965,1.78835602230873));
#23112=CARTESIAN_POINT('Ctrl Pts',(0.505493161016087,-2.45684558601761,
1.98687213972038));
#23113=CARTESIAN_POINT('Ctrl Pts',(0.250108060020668,1.98817892786946,2.18538825713204));
#23114=CARTESIAN_POINT('Ctrl Pts',(3.8468393694429,4.61243733220712,2.38390437454369));
#23115=CARTESIAN_POINT('Ctrl Pts',(8.0018522734089,3.01272882884126,2.58242049195535));
#23116=CARTESIAN_POINT('Ctrl Pts',(8.91007369571349,-1.34598748780205,2.78093660936701));
#23117=CARTESIAN_POINT('Ctrl Pts',(5.73976719690925,-4.47206986535408,2.97945272677866));
#23118=CARTESIAN_POINT('Ctrl Pts',(1.39424152787623,-3.50271791779653,3.17796884419032));
#23119=CARTESIAN_POINT('Ctrl Pts',(-0.146954797017362,0.674357611516781,
3.37648496160198));
#23120=CARTESIAN_POINT('Ctrl Pts',(2.5275771424141,4.23386867290823,3.57500107901363));
#23121=CARTESIAN_POINT('Ctrl Pts',(6.96855153613195,3.91608365047424,3.77351719642529));
#23122=CARTESIAN_POINT('Ctrl Pts',(9.10900868522111,0.0120235511094912,
3.97203331383693));
#23123=CARTESIAN_POINT('Ctrl Pts',(6.98875855737045,-3.90304740339865,4.17054943124861));
#23124=CARTESIAN_POINT('Ctrl Pts',(2.54948593565754,-4.24378183362265,4.36906554866025));
#23125=CARTESIAN_POINT('Ctrl Pts',(-0.143407781592193,-0.698141563015474,
4.56758166607191));
#23126=CARTESIAN_POINT('Ctrl Pts',(1.37617826049345,3.48684345900968,4.76609778348356));
#23127=CARTESIAN_POINT('Ctrl Pts',(5.71663606344787,4.47864357428809,4.96461390089523));
#23128=CARTESIAN_POINT('Ctrl Pts',(8.90305693908813,1.36898709382619,5.16313001830687));
#23129=CARTESIAN_POINT('Ctrl Pts',(8.01737725983028,-2.99436172457643,5.36164613571854));
#23130=CARTESIAN_POINT('Ctrl Pts',(3.87068562947579,-4.61553103529222,5.56016225313019));
#23131=CARTESIAN_POINT('Ctrl Pts',(0.260443364168955,-2.00988482013811,
5.75867837054185));
#23132=CARTESIAN_POINT('Ctrl Pts',(0.492841656646439,2.436375680996,5.95719448795349));
#23133=CARTESIAN_POINT('Ctrl Pts',(4.35505457120696,4.6514496783783,6.15571060536516));
#23134=CARTESIAN_POINT('Ctrl Pts',(8.31014098784587,2.60681454019155,6.35422672277681));
#23135=CARTESIAN_POINT('Ctrl Pts',(8.73610799988966,-1.82509176699825,6.55274284018847));
#23136=CARTESIAN_POINT('Ctrl Pts',(5.24286312047947,-4.58561375091533,6.75125895760012));
#23137=CARTESIAN_POINT('Ctrl Pts',(1.02945356160573,-3.14671788935761,6.94977507501179));
#23138=CARTESIAN_POINT('Ctrl Pts',(-0.0455603502579819,1.17388235834786,
7.14829119242343));
#23139=CARTESIAN_POINT('Ctrl Pts',(3.00229867643747,4.41946347189101,7.34680730983509));
#23140=CARTESIAN_POINT('Ctrl Pts',(7.38185932147204,3.61778400498435,7.54532342724674));
#23141=CARTESIAN_POINT('Ctrl Pts',(9.08240325419932,-0.496993236137507,
7.7438395446584));
#23142=CARTESIAN_POINT('Ctrl Pts',(6.5466046888036,-4.15663352541875,7.94235566207006));
#23143=CARTESIAN_POINT('Ctrl Pts',(2.09669971547073,-4.00970789967487,8.1408717794817));
#23144=CARTESIAN_POINT('Ctrl Pts',(-0.192173337388976,-0.19076805214061,
8.33938789689338));
#23145=CARTESIAN_POINT('Ctrl Pts',(1.77609193305126,3.80287354875093,8.53790401430502));
#23146=CARTESIAN_POINT('Ctrl Pts',(6.1989956324977,4.3139158920216,8.73642013171668));
#23147=CARTESIAN_POINT('Ctrl Pts',(9.0261266855466,0.874356120760312,8.93493624912834));
#23148=CARTESIAN_POINT('Ctrl Pts',(7.66845225155073,-3.36592235387631,9.13345236653999));
#23149=CARTESIAN_POINT('Ctrl Pts',(3.36930475145732,-4.52375316346519,9.33196848395166));
#23150=CARTESIAN_POINT('Ctrl Pts',(0.0657616873951493,-1.53881687686219,
9.53048460136329));
#23151=CARTESIAN_POINT('Ctrl Pts',(0.783144957380055,2.85533863417045,9.72900071877498));
#23152=CARTESIAN_POINT('Ctrl Pts',(4.86448860883662,4.63462933832978,9.92751683618659));
#23153=CARTESIAN_POINT('Ctrl Pts',(8.57217576114917,2.16961465444475,10.1260329535983));
#23154=CARTESIAN_POINT('Ctrl Pts',(8.51077704791793,-2.28229185953398,10.3245490710099));
#23155=CARTESIAN_POINT('Ctrl Pts',(4.73652024279266,-4.644118902346,10.5230651884216));
#23156=CARTESIAN_POINT('Ctrl Pts',(0.705797933930029,-2.75295019489822,
10.7215813058332));
#23157=CARTESIAN_POINT('Ctrl Pts',(0.109868939318185,1.65931793437198,10.9200974232449));
#23158=CARTESIAN_POINT('Ctrl Pts',(3.49447369645122,4.55201426291826,11.1186135406565));
#23159=CARTESIAN_POINT('Ctrl Pts',(7.76005555075585,3.27606251797663,11.3171296580682));
#23160=CARTESIAN_POINT('Ctrl Pts',(9.00027578003045,-1.00004496361109,11.5156457754798));
#23161=CARTESIAN_POINT('Ctrl Pts',(6.07936428979557,-4.36033029039609,11.7141618928915));
#23162=CARTESIAN_POINT('Ctrl Pts',(1.67223626118035,-3.72750807951321,11.9126780103032));
#23163=CARTESIAN_POINT('Ctrl Pts',(-0.185144289673645,0.31889512586586,
12.1111941277148));
#23164=CARTESIAN_POINT('Ctrl Pts',(2.20817641458127,4.07326024100545,12.3097102451265));
#23165=CARTESIAN_POINT('Ctrl Pts',(6.66044079877556,4.09741110905781,12.5082263625381));
#23166=CARTESIAN_POINT('Ctrl Pts',(9.09434983091284,0.369230824458725,12.7067424799498));
#23167=CARTESIAN_POINT('Ctrl Pts',(7.28097591722075,-3.69708402566464,12.9052585973614));
#23168=CARTESIAN_POINT('Ctrl Pts',(2.8809723938291,-4.37767965107946,13.1037747147731));
#23169=CARTESIAN_POINT('Ctrl Pts',(-0.0762212094817758,-1.04927952433239,
13.3022908321848));
#23170=CARTESIAN_POINT('Ctrl Pts',(1.11753675741321,3.24003083138531,13.5008069495964));
#23171=CARTESIAN_POINT('Ctrl Pts',(5.369025456116,4.5621825836419,13.6993230670081));
#23172=CARTESIAN_POINT('Ctrl Pts',(8.78481240824481,1.70637430771384,13.8978391844197));
#23173=CARTESIAN_POINT('Ctrl Pts',(8.23678489819753,-2.71209910053747,14.0963553018314));
#23174=CARTESIAN_POINT('Ctrl Pts',(4.22681609508684,-4.64688374211174,14.294871419243));
#23175=CARTESIAN_POINT('Ctrl Pts',(0.427159151106815,-2.32614064576156,
14.4933875366547));
#23176=CARTESIAN_POINT('Ctrl Pts',(0.317467618415429,2.12483780609018,14.6919036540663));
#23177=CARTESIAN_POINT('Ctrl Pts',(3.99819491609722,4.62993021382537,14.890419771478));
#23178=CARTESIAN_POINT('Ctrl Pts',(8.09860099979244,2.8950206023505,15.0889358888896));
#23179=CARTESIAN_POINT('Ctrl Pts',(8.86361197604717,-1.49109380762589,15.2874520063013));
#23180=CARTESIAN_POINT('Ctrl Pts',(5.59264534485911,-4.5116928721902,15.485968123713));
#23181=CARTESIAN_POINT('Ctrl Pts',(1.2811901266875,-3.40056942590122,15.6844842411246));
#23182=CARTESIAN_POINT('Ctrl Pts',(-0.122405002240585,0.824730814938715,
15.8830003585363));
#23183=CARTESIAN_POINT('Ctrl Pts',(2.66724567793686,4.29475826350135,16.0815164759479));
#23184=CARTESIAN_POINT('Ctrl Pts',(7.09543313909595,3.83172778931411,16.2800325933596));
#23185=CARTESIAN_POINT('Ctrl Pts',(9.10690753736432,-0.140326107135887,
16.4785487107712));
#23186=CARTESIAN_POINT('Ctrl Pts',(6.85959888110794,-3.98387202395643,16.6770648281829));
#23187=CARTESIAN_POINT('Ctrl Pts',(2.41154968938301,-4.179063722519,16.8755809455945));
#23188=CARTESIAN_POINT('Ctrl Pts',(-0.163801198896094,-0.547148358219792,
17.0740970630062));
#23189=CARTESIAN_POINT('Ctrl Pts',(1.49200357138825,3.5858350646717,17.2726131804178));
#23190=CARTESIAN_POINT('Ctrl Pts',(5.86260948835618,4.43497894515246,17.4711292978295));
#23191=CARTESIAN_POINT('Ctrl Pts',(8.94549879098837,1.22265346990726,17.6696454152412));
#23192=CARTESIAN_POINT('Ctrl Pts',(7.91742009870712,-3.10935479574357,17.8681615326528));
#23193=CARTESIAN_POINT('Ctrl Pts',(3.71986832177296,-4.59387508565289,18.0666776500645));
#23194=CARTESIAN_POINT('Ctrl Pts',(0.196881531601468,-1.87141195688986,
18.2651937674761));
#23195=CARTESIAN_POINT('Ctrl Pts',(0.574744016316265,2.56485464396025,18.4637098848878));
#23196=CARTESIAN_POINT('Ctrl Pts',(4.50741650012369,4.6522761505852,18.6622260022994));
#23197=CARTESIAN_POINT('Ctrl Pts',(8.3934323297128,2.47923165417059,18.8607421197111));
#23198=CARTESIAN_POINT('Ctrl Pts',(8.67405212821057,-1.96424603112833,19.0592582371228));
#23199=CARTESIAN_POINT('Ctrl Pts',(5.09228962209667,-4.60890456507674,19.2577743545344));
#23200=CARTESIAN_POINT('Ctrl Pts',(0.928254782143413,-3.0328159689208,19.4562904719461));
#23201=CARTESIAN_POINT('Ctrl Pts',(-0.00470849360073685,1.32066780116548,
19.6548065893577));
#23202=CARTESIAN_POINT('Ctrl Pts',(3.14778981602278,4.46470912096001,19.8533227067694));
#23203=CARTESIAN_POINT('Ctrl Pts',(7.49875172579254,3.52005475507203,20.051838824181));
#23204=CARTESIAN_POINT('Ctrl Pts',(9.06364908309027,-0.648198796048447,
20.2503549415927));
#23205=CARTESIAN_POINT('Ctrl Pts',(6.4093786550744,-4.22284422156345,20.4488710590044));
#23206=CARTESIAN_POINT('Ctrl Pts',(1.96667081116617,-3.93028923259476,20.647387176416));
#23207=CARTESIAN_POINT('Ctrl Pts',(-0.195927116407106,-0.0384501329489085,
20.8459032938277));
#23208=CARTESIAN_POINT('Ctrl Pts',(1.90205092121151,3.88860087953163,21.0444194112393));
#23209=CARTESIAN_POINT('Ctrl Pts',(6.3393165377314,4.25454515162759,21.242935528651));
#23210=CARTESIAN_POINT('Ctrl Pts',(9.05230630112455,0.724257949825445,21.4414516460626));
#23211=CARTESIAN_POINT('Ctrl Pts',(7.55651576606266,-3.46929099370176,21.6399677634743));
#23212=CARTESIAN_POINT('Ctrl Pts',(3.22176150253947,-4.48572906904549,21.838483880886));
#23213=CARTESIAN_POINT('Ctrl Pts',(0.0177289115966501,-1.39422211492368,
22.0369999982976));
#23214=CARTESIAN_POINT('Ctrl Pts',(0.878610280341868,2.97408755340353,22.2355161157093));
#23215=CARTESIAN_POINT('Ctrl Pts',(5.01602646728549,4.61878321962123,22.4340322331209));
#23216=CARTESIAN_POINT('Ctrl Pts',(8.64101112050298,2.03368736229999,22.6325483505326));
#23217=CARTESIAN_POINT('Ctrl Pts',(8.43387092517075,-2.41382509078919,22.8310644679442));
#23218=CARTESIAN_POINT('Ctrl Pts',(4.58430347192829,-4.65079401118156,23.0295805853559));
#23219=CARTESIAN_POINT('Ctrl Pts',(0.617664534920323,-2.6286704174496,23.2280967027675));
#23220=CARTESIAN_POINT('Ctrl Pts',(0.166535948123391,1.80077057177711,23.4266128201792));
#23221=CARTESIAN_POINT('Ctrl Pts',(3.64403475383551,4.58104059437149,23.6251289375908));
#23222=CARTESIAN_POINT('Ctrl Pts',(7.86556810560143,3.16619499327494,23.8236450550025));
#23223=CARTESIAN_POINT('Ctrl Pts',(8.96507004425898,-1.14841087401253,24.0221611724142));
#23224=CARTESIAN_POINT('Ctrl Pts',(5.93576426504054,-4.41090351654891,24.2206772898258));
#23225=CARTESIAN_POINT('Ctrl Pts',(1.55158838794904,-3.63478122412758,24.4191934072375));
#23226=CARTESIAN_POINT('Ctrl Pts',(-0.172046559910909,0.471552713422697,
24.6177095246491));
#23227=CARTESIAN_POINT('Ctrl Pts',(2.34243741690352,4.14307145960353,24.8162256420608));
#23228=CARTESIAN_POINT('Ctrl Pts',(6.79403703197597,4.02620936921257,25.0147417594724));
#23229=CARTESIAN_POINT('Ctrl Pts',(9.10329134237422,0.209832038399488,25.2133007328261));
#23230=CARTESIAN_POINT('Ctrl Pts',(7.80718744833136,-2.44564931016495,25.3456876670425));
#23231=CARTESIAN_POINT('Ctrl Pts',(6.7401774553626,-3.20569558398784,25.4119025621217));
#23232=CARTESIAN_POINT('Ctrl Pts',(5.88688308661327,2.88166464694226,-0.413294290592403));
#23233=CARTESIAN_POINT('Ctrl Pts',(6.84537358445575,2.40588471549031,-0.347122251455184));
#23234=CARTESIAN_POINT('Ctrl Pts',(8.23365752427788,0.430873938343679,-0.214778173180747));
#23235=CARTESIAN_POINT('Ctrl Pts',(6.86376121760315,-2.94715670275194,-0.0162620557690901));
#23236=CARTESIAN_POINT('Ctrl Pts',(3.28608690294124,-3.61718018023642,0.182254061642566));
#23237=CARTESIAN_POINT('Ctrl Pts',(0.781880406995935,-0.979166244321737,
0.380770179054222));
#23238=CARTESIAN_POINT('Ctrl Pts',(1.64193314359211,2.55787552455616,0.579286296465875));
#23239=CARTESIAN_POINT('Ctrl Pts',(5.07993189931123,3.75125370222575,0.777802413877532));
#23240=CARTESIAN_POINT('Ctrl Pts',(7.94674205925474,1.50993542852403,0.976318531289188));
#23241=CARTESIAN_POINT('Ctrl Pts',(7.61734820438694,-2.11448150974993,1.17483464870084));
#23242=CARTESIAN_POINT('Ctrl Pts',(4.39321803491158,-3.80232526959411,1.3733507661125));
#23243=CARTESIAN_POINT('Ctrl Pts',(1.22704502026327,-2.0081611280352,1.57186688352415));
#23244=CARTESIAN_POINT('Ctrl Pts',(1.01829993859556,1.62508529687376,1.77038300093581));
#23245=CARTESIAN_POINT('Ctrl Pts',(3.95817375267475,3.77008527062174,1.96889911834747));
#23246=CARTESIAN_POINT('Ctrl Pts',(7.35437229592725,2.462525507432,2.16741523575912));
#23247=CARTESIAN_POINT('Ctrl Pts',(8.09672865983581,-1.10017486129741,2.36593135317078));
#23248=CARTESIAN_POINT('Ctrl Pts',(5.50540329893836,-3.65535258567839,2.56444747058243));
#23249=CARTESIAN_POINT('Ctrl Pts',(1.95348461951634,-2.8630297341532,2.76296358799409));
#23250=CARTESIAN_POINT('Ctrl Pts',(0.693751175975549,0.551202220257554,
2.96147970540574));
#23251=CARTESIAN_POINT('Ctrl Pts',(2.87984341841113,3.46065318004877,3.1599958228174));
#23252=CARTESIAN_POINT('Ctrl Pts',(6.50977938134639,3.20090403962421,3.35851194022905));
#23253=CARTESIAN_POINT('Ctrl Pts',(8.25933290131072,0.00982773524565914,
3.55702805764071));
#23254=CARTESIAN_POINT('Ctrl Pts',(6.52629607038668,-3.19024855326339,3.75554417505237));
#23255=CARTESIAN_POINT('Ctrl Pts',(2.89775109124319,-3.46875593755042,3.95406029246402));
#23256=CARTESIAN_POINT('Ctrl Pts',(0.69665041333009,-0.570642598253718,
4.15257640987568));
#23257=CARTESIAN_POINT('Ctrl Pts',(1.93872017863753,2.85005436799852,4.35109252728733));
#23258=CARTESIAN_POINT('Ctrl Pts',(5.48649651727959,3.66072576290342,4.54960864469899));
#23259=CARTESIAN_POINT('Ctrl Pts',(8.09099334705098,1.11897413587954,4.74812476211065));
#23260=CARTESIAN_POINT('Ctrl Pts',(7.36706201253862,-2.44751271825679,4.9466408795223));
#23261=CARTESIAN_POINT('Ctrl Pts',(3.97766506003213,-3.7726139823619,5.14515699693396));
#23262=CARTESIAN_POINT('Ctrl Pts',(1.02674774506536,-1.64282712377203,5.34367311434561));
#23263=CARTESIAN_POINT('Ctrl Pts',(1.21670401249677,1.99142956468722,5.54218923175727));
#23264=CARTESIAN_POINT('Ctrl Pts',(4.37357552585394,3.80197293891488,5.74070534916892));
#23265=CARTESIAN_POINT('Ctrl Pts',(7.60635940332531,2.13074181682499,5.93922146658058));
#23266=CARTESIAN_POINT('Ctrl Pts',(7.95453366396254,-1.49178213007847,6.13773758399224));
#23267=CARTESIAN_POINT('Ctrl Pts',(5.09924694286633,-3.74816037897555,6.33625370140389));
#23268=CARTESIAN_POINT('Ctrl Pts',(1.65531650589596,-2.57204465036969,6.53476981881556));
#23269=CARTESIAN_POINT('Ctrl Pts',(0.776628336729841,0.959500643563771,
6.7332859362272));
#23270=CARTESIAN_POINT('Ctrl Pts',(3.26786834626679,3.6123534997611,6.93180205363886));
#23271=CARTESIAN_POINT('Ctrl Pts',(6.84760632218384,2.95708173512582,7.1303181710505));
#23272=CARTESIAN_POINT('Ctrl Pts',(8.23758631997216,-0.406229232878139,
7.32883428846218));
#23273=CARTESIAN_POINT('Ctrl Pts',(6.16489109788061,-3.39752319671194,7.52735040587382));
#23274=CARTESIAN_POINT('Ctrl Pts',(2.52765551345678,-3.27743004474078,7.72586652328549));
#23275=CARTESIAN_POINT('Ctrl Pts',(0.656790727359,-0.155928801126063,7.92438264069713));
#23276=CARTESIAN_POINT('Ctrl Pts',(2.26559912307384,3.10836907247963,8.1228987581088));
#23277=CARTESIAN_POINT('Ctrl Pts',(5.88076457458627,3.52608167695778,8.32141487552045));
#23278=CARTESIAN_POINT('Ctrl Pts',(8.19158732913988,0.714675754863574,8.5199309929321));
#23279=CARTESIAN_POINT('Ctrl Pts',(7.08185986462416,-2.75121662896035,8.71844711034376));
#23280=CARTESIAN_POINT('Ctrl Pts',(3.56784948378791,-3.69759715767183,8.91696322775543));
#23281=CARTESIAN_POINT('Ctrl Pts',(0.867620049835816,-1.2577885451434,9.11547934516706));
#23282=CARTESIAN_POINT('Ctrl Pts',(1.45399031457103,2.33387889135228,9.31399546257875));
#23283=CARTESIAN_POINT('Ctrl Pts',(4.78997354349419,3.78822443423146,9.51251157999037));
#23284=CARTESIAN_POINT('Ctrl Pts',(7.8205397526871,1.77338609991104,9.71102769740205));
#23285=CARTESIAN_POINT('Ctrl Pts',(7.77035405525285,-1.8654854913274,9.90954381481369));
#23286=CARTESIAN_POINT('Ctrl Pts',(4.68537555826851,-3.79598095490491,10.1080599322253));
#23287=CARTESIAN_POINT('Ctrl Pts',(1.39076888675897,-2.25018926719472,10.306576049637));
#23288=CARTESIAN_POINT('Ctrl Pts',(0.903672160428571,1.35628294827392,10.5050921670486));
#23289=CARTESIAN_POINT('Ctrl Pts',(3.67015929568852,3.72069703895061,10.7036082844603));
#23290=CARTESIAN_POINT('Ctrl Pts',(7.156733998233,2.67776755651859,10.902124401872));
#23291=CARTESIAN_POINT('Ctrl Pts',(8.17045747715504,-0.817410517633158,
11.1006405192836));
#23292=CARTESIAN_POINT('Ctrl Pts',(5.78298105352307,-3.56401958853324,11.2991566366953));
#23293=CARTESIAN_POINT('Ctrl Pts',(2.18071022148213,-3.04676731509573,11.4976727541069));
#23294=CARTESIAN_POINT('Ctrl Pts',(0.662536086558379,0.260656509846819,
11.6961888715186));
#23295=CARTESIAN_POINT('Ctrl Pts',(2.61877364278075,3.32937606128419,11.8947049889302));
#23296=CARTESIAN_POINT('Ctrl Pts',(6.25793774774488,3.34911634724554,12.0932211063419));
#23297=CARTESIAN_POINT('Ctrl Pts',(8.24735113836601,0.301799589347462,12.2917372237535));
#23298=CARTESIAN_POINT('Ctrl Pts',(6.76514687416864,-3.02189949163811,12.4902533411652));
#23299=CARTESIAN_POINT('Ctrl Pts',(3.16869942579002,-3.57820050080496,12.6887694585768));
#23300=CARTESIAN_POINT('Ctrl Pts',(0.751566954770839,-0.857653555925328,
12.8872855759885));
#23301=CARTESIAN_POINT('Ctrl Pts',(1.72731339933552,2.64831620117018,13.0858016934002));
#23302=CARTESIAN_POINT('Ctrl Pts',(5.20236872621718,3.72900835754984,13.2843178108118));
#23303=CARTESIAN_POINT('Ctrl Pts',(7.99434336961907,1.39474559334568,13.4828339282235));
#23304=CARTESIAN_POINT('Ctrl Pts',(7.54640006010282,-2.21679865437008,13.6813500456351));
#23305=CARTESIAN_POINT('Ctrl Pts',(4.26875675973819,-3.79824086239538,13.8798661630468));
#23306=CARTESIAN_POINT('Ctrl Pts',(1.16301685561255,-1.9013263388412,14.0783822804584));
#23307=CARTESIAN_POINT('Ctrl Pts',(1.07335787448695,1.73678667876183,14.2768983978701));
#23308=CARTESIAN_POINT('Ctrl Pts',(4.08188780578152,3.78438349314049,14.4754145152818));
#23309=CARTESIAN_POINT('Ctrl Pts',(7.43345216672421,2.36631389110821,14.6739306326934));
#23310=CARTESIAN_POINT('Ctrl Pts',(8.05875206907788,-1.21878096033793,14.8724467501051));
#23311=CARTESIAN_POINT('Ctrl Pts',(5.38514975673243,-3.68773939197872,15.0709628675167));
#23312=CARTESIAN_POINT('Ctrl Pts',(1.86107937002522,-2.77953623668677,15.2694789849284));
#23313=CARTESIAN_POINT('Ctrl Pts',(0.713817534175901,0.674113331777405,
15.46799510234));
#23314=CARTESIAN_POINT('Ctrl Pts',(2.9940048152212,3.5104227339951,15.6665112197517));
#23315=CARTESIAN_POINT('Ctrl Pts',(6.61348907494099,3.13195377174095,15.8650273371633));
#23316=CARTESIAN_POINT('Ctrl Pts',(8.257615478175,-0.114698878595687,16.063543454575));
#23317=CARTESIAN_POINT('Ctrl Pts',(6.42072433944188,-3.25631247771842,16.2620595719866));
#23318=CARTESIAN_POINT('Ctrl Pts',(2.78500562221897,-3.41585705137789,16.4605756893983));
#23319=CARTESIAN_POINT('Ctrl Pts',(0.67998136903583,-0.447224713876356,
16.65909180681));
#23320=CARTESIAN_POINT('Ctrl Pts',(2.03339274915041,2.93096750947701,16.8576079242216));
#23321=CARTESIAN_POINT('Ctrl Pts',(5.60581136526813,3.62503544056518,17.0561240416333));
#23322=CARTESIAN_POINT('Ctrl Pts',(8.12568420335589,0.999364870669326,17.2546401590449));
#23323=CARTESIAN_POINT('Ctrl Pts',(7.28535965135699,-2.54150503784963,17.4531562764566));
#23324=CARTESIAN_POINT('Ctrl Pts',(3.85439094932391,-3.75491297725849,17.6516723938682));
#23325=CARTESIAN_POINT('Ctrl Pts',(0.974793970633971,-1.52964303811135,
17.8501885112799));
#23326=CARTESIAN_POINT('Ctrl Pts',(1.2836488526281,2.09644489844015,18.0487046286916));
#23327=CARTESIAN_POINT('Ctrl Pts',(4.49811216942012,3.80264847561477,18.2472207461032));
#23328=CARTESIAN_POINT('Ctrl Pts',(7.67443956106538,2.02645891285741,18.4457368635149));
#23329=CARTESIAN_POINT('Ctrl Pts',(7.90381082245328,-1.60552317494378,18.6442529809265));
#23330=CARTESIAN_POINT('Ctrl Pts',(4.9761721155001,-3.76719767944954,18.8427690983382));
#23331=CARTESIAN_POINT('Ctrl Pts',(1.57259927845708,-2.47894420875808,19.0412852157498));
#23332=CARTESIAN_POINT('Ctrl Pts',(0.810019572635768,1.07947921368855,19.2398013331615));
#23333=CARTESIAN_POINT('Ctrl Pts',(3.38678898688482,3.6493361063157,19.4383174505731));
#23334=CARTESIAN_POINT('Ctrl Pts',(6.94315110686829,2.87720041011993,19.6368335679848));
#23335=CARTESIAN_POINT('Ctrl Pts',(8.22225715251285,-0.529820690755693,
19.8353496853965));
#23336=CARTESIAN_POINT('Ctrl Pts',(6.05272613795891,-3.45164208273989,20.0338658028081));
#23337=CARTESIAN_POINT('Ctrl Pts',(2.42137329831411,-3.212515309774,20.2323819202198));
#23338=CARTESIAN_POINT('Ctrl Pts',(0.65372248686789,-0.0314281299545405,
20.4308980376314));
#23339=CARTESIAN_POINT('Ctrl Pts',(2.36855469553213,3.178440343651,20.6294141550431));
#23340=CARTESIAN_POINT('Ctrl Pts',(5.99545920128352,3.47755359131801,20.8279302724548));
#23341=CARTESIAN_POINT('Ctrl Pts',(8.21298586010566,0.591989447683331,21.0264463898664));
#23342=CARTESIAN_POINT('Ctrl Pts',(6.99036591797756,-2.83570744333498,21.2249625072781));
#23343=CARTESIAN_POINT('Ctrl Pts',(3.44725150283742,-3.6665172604341,21.4234786246897));
#23344=CARTESIAN_POINT('Ctrl Pts',(0.828359319011244,-1.13960058009792,
21.6219947421014));
#23345=CARTESIAN_POINT('Ctrl Pts',(1.53202116508044,2.43094114262164,21.820510859513));
#23346=CARTESIAN_POINT('Ctrl Pts',(4.91383661347899,3.77527223251319,22.0190269769247));
#23347=CARTESIAN_POINT('Ctrl Pts',(7.87680396956558,1.66228269728872,22.2175430943363));
#23348=CARTESIAN_POINT('Ctrl Pts',(7.7074930081086,-1.97299730385434,22.416059211748));
#23349=CARTESIAN_POINT('Ctrl Pts',(4.56095756308617,-3.80143701374933,22.6145753291597));
#23350=CARTESIAN_POINT('Ctrl Pts',(1.31873095853907,-2.14860623751896,22.8130914465713));
#23351=CARTESIAN_POINT('Ctrl Pts',(0.949990286798536,1.47190262315773,23.011607563983));
#23352=CARTESIAN_POINT('Ctrl Pts',(3.7924065803434,3.74442240079083,23.2101236813946));
#23353=CARTESIAN_POINT('Ctrl Pts',(7.24297719250067,2.58796472414074,23.4086397988063));
#23354=CARTESIAN_POINT('Ctrl Pts',(8.14168123233833,-0.938680920498277,
23.6071559162179));
#23355=CARTESIAN_POINT('Ctrl Pts',(5.66560616055497,-3.60535681683013,23.8056720336296));
#23356=CARTESIAN_POINT('Ctrl Pts',(2.08209581503262,-2.97097481614092,24.0041881510412));
#23357=CARTESIAN_POINT('Ctrl Pts',(0.673241827254791,0.385434817028999,
24.2027042684529));
#23358=CARTESIAN_POINT('Ctrl Pts',(2.72851506381635,3.38643791990783,24.4012203858645));
#23359=CARTESIAN_POINT('Ctrl Pts',(6.36713580394013,3.29091791303403,24.5997365032762));
#23360=CARTESIAN_POINT('Ctrl Pts',(8.25465969525897,0.17151120336101,24.7982954766299));
#23361=CARTESIAN_POINT('Ctrl Pts',(7.19525837483205,-1.99900958588141,24.9306824108463));
#23362=CARTESIAN_POINT('Ctrl Pts',(6.32311239899223,-2.62025147071356,24.9968973059255));
#23363=CARTESIAN_POINT('Ctrl Pts',(5.99341579333084,3.0962819108244,-0.27495920519366));
#23364=CARTESIAN_POINT('Ctrl Pts',(7.02329163031133,2.58506739568259,-0.208787166056442));
#23365=CARTESIAN_POINT('Ctrl Pts',(8.51497056474962,0.462964065771816,-0.0764430877820045));
#23366=CARTESIAN_POINT('Ctrl Pts',(7.04304871618797,-3.16665160770128,0.122073029629653));
#23367=CARTESIAN_POINT('Ctrl Pts',(3.19892054011338,-3.88657631350085,0.320589147041309));
#23368=CARTESIAN_POINT('Ctrl Pts',(0.508208668906595,-1.05209144762919,
0.519105264452963));
#23369=CARTESIAN_POINT('Ctrl Pts',(1.43231541168923,2.74837799923302,0.717621381864618));
#23370=CARTESIAN_POINT('Ctrl Pts',(5.12636543519397,4.03063520713254,0.916137499276276));
#23371=CARTESIAN_POINT('Ctrl Pts',(8.20668654383497,1.62239064105283,1.11465361668793));
#23372=CARTESIAN_POINT('Ctrl Pts',(7.85276047702285,-2.27196140132349,1.31316973409959));
#23373=CARTESIAN_POINT('Ctrl Pts',(4.38850729527858,-4.08551042322263,1.51168585151124));
#23374=CARTESIAN_POINT('Ctrl Pts',(0.986527733847538,-2.15772261402933,
1.7102019689229));
#23375=CARTESIAN_POINT('Ctrl Pts',(0.7622359790706,1.74611650720567,1.90871808633455));
#23376=CARTESIAN_POINT('Ctrl Pts',(3.92106229159746,4.0508692911502,2.10723420374621));
#23377=CARTESIAN_POINT('Ctrl Pts',(7.57019895508782,2.64592661456843,2.30575032115786));
#23378=CARTESIAN_POINT('Ctrl Pts',(8.36784367179503,-1.18211240346562,2.50426643856952));
#23379=CARTESIAN_POINT('Ctrl Pts',(5.58352459826198,-3.92759167890361,2.70278255598118));
#23380=CARTESIAN_POINT('Ctrl Pts',(1.7670702556363,-3.07625912870098,2.90129867339283));
#23381=CARTESIAN_POINT('Ctrl Pts',(0.413515851644582,0.592254017343965,
3.09981479080449));
#23382=CARTESIAN_POINT('Ctrl Pts',(2.76242132641212,3.7183916776686,3.29833090821614));
#23383=CARTESIAN_POINT('Ctrl Pts',(6.66270343294158,3.43929724324088,3.4968470256278));
#23384=CARTESIAN_POINT('Ctrl Pts',(8.54255816261418,0.0105596738669375,
3.69536314303945));
#23385=CARTESIAN_POINT('Ctrl Pts',(6.6804502327146,-3.42784816997514,3.89387926045112));
#23386=CARTESIAN_POINT('Ctrl Pts',(2.78166270604797,-3.72709790290783,4.09239537786277));
#23387=CARTESIAN_POINT('Ctrl Pts',(0.416631015022661,-0.613142253174304,
4.29091149527442));
#23388=CARTESIAN_POINT('Ctrl Pts',(1.75120620592284,3.06231739833558,4.48942761268608));
#23389=CARTESIAN_POINT('Ctrl Pts',(5.56320969933569,3.93336503336498,4.68794373009773));
#23390=CARTESIAN_POINT('Ctrl Pts',(8.36168121106336,1.20231178852842,4.88645984750939));
#23391=CARTESIAN_POINT('Ctrl Pts',(7.58383376163584,-2.62979572036334,5.08497596492104));
#23392=CARTESIAN_POINT('Ctrl Pts',(3.94200524984668,-4.05358633333867,5.2834920823327));
#23393=CARTESIAN_POINT('Ctrl Pts',(0.771312951433223,-1.76517968922739,
5.48200819974436));
#23394=CARTESIAN_POINT('Ctrl Pts',(0.97541656054666,2.13974493679014,5.68052431715601));
#23395=CARTESIAN_POINT('Ctrl Pts',(4.36740187430494,4.08513185206935,5.87904043456767));
#23396=CARTESIAN_POINT('Ctrl Pts',(7.84095326483218,2.28943272461384,6.07755655197932));
#23397=CARTESIAN_POINT('Ctrl Pts',(8.21505844260491,-1.60288534238506,6.27607266939098));
#23398=CARTESIAN_POINT('Ctrl Pts',(5.14711900207072,-4.02731150295548,6.47458878680263));
#23399=CARTESIAN_POINT('Ctrl Pts',(1.44669552446588,-2.76360239669899,6.6731049042143));
#23400=CARTESIAN_POINT('Ctrl Pts',(0.502565441067234,1.03096121515846,6.87162102162594));
#23401=CARTESIAN_POINT('Ctrl Pts',(3.17934512299035,3.88139015713774,7.07013713903761));
#23402=CARTESIAN_POINT('Ctrl Pts',(7.0256906552799,3.17731582507866,7.26865325644925));
#23403=CARTESIAN_POINT('Ctrl Pts',(8.51919196471455,-0.436483900631263,
7.46716937386092));
#23404=CARTESIAN_POINT('Ctrl Pts',(6.2921289615216,-3.65055997294754,7.66568549127257));
#23405=CARTESIAN_POINT('Ctrl Pts',(2.38400358079477,-3.52152266305215,7.86420160868423));
#23406=CARTESIAN_POINT('Ctrl Pts',(0.373802705776339,-0.16754188479758,
8.06271772609589));
#23407=CARTESIAN_POINT('Ctrl Pts',(2.10243005973299,3.33987056457006,8.26123384350753));
#23408=CARTESIAN_POINT('Ctrl Pts',(5.98684159389007,3.78869308197905,8.4597499609192));
#23409=CARTESIAN_POINT('Ctrl Pts',(8.4697671146088,0.767902543495819,8.65826607833084));
#23410=CARTESIAN_POINT('Ctrl Pts',(7.27739066026635,-2.95611853726567,8.85678219574251));
#23411=CARTESIAN_POINT('Ctrl Pts',(3.50166790634439,-3.97298249293629,9.05529831315416));
#23412=CARTESIAN_POINT('Ctrl Pts',(0.600333929022254,-1.35146465571633,
9.25381443056581));
#23413=CARTESIAN_POINT('Ctrl Pts',(1.23037519550738,2.50769880562501,9.45233054797748));
#23414=CARTESIAN_POINT('Ctrl Pts',(4.81481189860833,4.07035940226423,9.65084666538912));
#23415=CARTESIAN_POINT('Ctrl Pts',(8.07108508884113,1.90546228475562,9.84936278280079));
#23416=CARTESIAN_POINT('Ctrl Pts',(8.01716171947454,-2.00442094739626,10.0478789002124));
#23417=CARTESIAN_POINT('Ctrl Pts',(4.70242378644322,-4.07869360405195,10.2463950176241));
#23418=CARTESIAN_POINT('Ctrl Pts',(1.16244523581599,-2.41777624309588,10.4449111350357));
#23419=CARTESIAN_POINT('Ctrl Pts',(0.639071086725107,1.45729461030662,10.6434272524474));
#23420=CARTESIAN_POINT('Ctrl Pts',(3.61159742927608,3.99780278027315,10.841943369859));
#23421=CARTESIAN_POINT('Ctrl Pts',(7.35784118240728,2.87719921033794,11.0404594872707));
#23422=CARTESIAN_POINT('Ctrl Pts',(8.44706357811351,-0.878288666292467,
11.2389756046823));
#23423=CARTESIAN_POINT('Ctrl Pts',(5.88177546561389,-3.82945648915419,11.437491722094));
#23424=CARTESIAN_POINT('Ctrl Pts',(2.01121890138154,-3.27368090323489,11.6360078395057));
#23425=CARTESIAN_POINT('Ctrl Pts',(0.379975961147697,0.280069381853164,
11.8345239569173));
#23426=CARTESIAN_POINT('Ctrl Pts',(2.4819079000476,3.57733745452462,12.033040074329));
#23427=CARTESIAN_POINT('Ctrl Pts',(6.39210543142176,3.59854793451629,12.2315561917406));
#23428=CARTESIAN_POINT('Ctrl Pts',(8.52968403588164,0.324276667717884,12.4300723091523));
#23429=CARTESIAN_POINT('Ctrl Pts',(6.93708988851933,-3.24696100298028,12.6285884265639));
#23430=CARTESIAN_POINT('Ctrl Pts',(3.07279041513639,-3.84469355089646,12.8271045439756));
#23431=CARTESIAN_POINT('Ctrl Pts',(0.475637566686629,-0.921528878727684,
13.0256206613872));
#23432=CARTESIAN_POINT('Ctrl Pts',(1.52405451869475,2.84555441124189,13.2241367787989));
#23433=CARTESIAN_POINT('Ctrl Pts',(5.25792096951678,4.00673309958052,13.4226528962106));
#23434=CARTESIAN_POINT('Ctrl Pts',(8.257833049161,1.4986218314684,13.6211690136222));
#23435=CARTESIAN_POINT('Ctrl Pts',(7.77652833946771,-2.38189880309254,13.8196851310339));
#23436=CARTESIAN_POINT('Ctrl Pts',(4.25477653818775,-4.08112182230083,14.0182012484455));
#23437=CARTESIAN_POINT('Ctrl Pts',(0.917730954110628,-2.04293110781465,
14.2167173658572));
#23438=CARTESIAN_POINT('Ctrl Pts',(0.821394455796449,1.86613705453794,14.4152334832688));
#23439=CARTESIAN_POINT('Ctrl Pts',(4.05399017588675,4.06623240003544,14.6137496006805));
#23440=CARTESIAN_POINT('Ctrl Pts',(7.65516844441363,2.54254946152231,14.8122657180922));
#23441=CARTESIAN_POINT('Ctrl Pts',(8.32703870473431,-1.30955190943392,15.0107818355038));
#23442=CARTESIAN_POINT('Ctrl Pts',(5.45431495277465,-3.96239055204922,15.2092979529155));
#23443=CARTESIAN_POINT('Ctrl Pts',(1.66778295557931,-2.98654729975826,15.4078140703271));
#23444=CARTESIAN_POINT('Ctrl Pts',(0.435076688703739,0.724319159497842,
15.6063301877388));
#23445=CARTESIAN_POINT('Ctrl Pts',(2.88508510279309,3.77186791049719,15.8048463051504));
#23446=CARTESIAN_POINT('Ctrl Pts',(6.77413709632598,3.36521177759866,16.0033624225621));
#23447=CARTESIAN_POINT('Ctrl Pts',(8.54071283123811,-0.123241288109086,
16.2018785399737));
#23448=CARTESIAN_POINT('Ctrl Pts',(6.56701585333057,-3.49883232646441,16.4003946573854));
#23449=CARTESIAN_POINT('Ctrl Pts',(2.66052031127365,-3.67025927509159,16.598910774797));
#23450=CARTESIAN_POINT('Ctrl Pts',(0.398720513058523,-0.480532595324168,
16.7974268922087));
#23451=CARTESIAN_POINT('Ctrl Pts',(1.85292968989636,3.14925669454191,16.9959430096203));
#23452=CARTESIAN_POINT('Ctrl Pts',(5.69141073963082,3.89501660876095,17.194459127032));
#23453=CARTESIAN_POINT('Ctrl Pts',(8.39895573256671,1.07379440374864,17.3929752444437));
#23454=CARTESIAN_POINT('Ctrl Pts',(7.49604646714037,-2.73078829048094,17.5914913618553));
#23455=CARTESIAN_POINT('Ctrl Pts',(3.80955007347359,-4.03456701338995,17.790007479267));
#23456=CARTESIAN_POINT('Ctrl Pts',(0.715489824289806,-1.64356601103751,
17.9885235966786));
#23457=CARTESIAN_POINT('Ctrl Pts',(1.04734724052415,2.25258148028018,18.1870397140903));
#23458=CARTESIAN_POINT('Ctrl Pts',(4.50121361298798,4.08585770060491,18.3855558315019));
#23459=CARTESIAN_POINT('Ctrl Pts',(7.91410381728119,2.1773831599618,18.5840719489136));
#23460=CARTESIAN_POINT('Ctrl Pts',(8.16055792437237,-1.72509746033864,18.7825880663253));
#23461=CARTESIAN_POINT('Ctrl Pts',(5.0148779510323,-4.04776664132528,18.9811041837369));
#23462=CARTESIAN_POINT('Ctrl Pts',(1.35781777968586,-2.66356812881232,19.1796203011486));
#23463=CARTESIAN_POINT('Ctrl Pts',(0.538443550556935,1.1598754095142,19.3781364185603));
#23464=CARTESIAN_POINT('Ctrl Pts',(3.30712259659747,3.92112711119714,19.5766525359719));
#23465=CARTESIAN_POINT('Ctrl Pts',(7.12835131317638,3.09148519177063,19.7751686533836));
#23466=CARTESIAN_POINT('Ctrl Pts',(8.50272112937199,-0.569280059186615,
19.9736847707952));
#23467=CARTESIAN_POINT('Ctrl Pts',(6.17161031033075,-3.70870946234774,20.1722008882069));
#23468=CARTESIAN_POINT('Ctrl Pts',(2.26980580259814,-3.45177328404759,20.3707170056185));
#23469=CARTESIAN_POINT('Ctrl Pts',(0.370505952442893,-0.0337687976193256,
20.5692331230302));
#23470=CARTESIAN_POINT('Ctrl Pts',(2.21305343742525,3.41516052227788,20.7677492404418));
#23471=CARTESIAN_POINT('Ctrl Pts',(6.11007831343283,3.73655077808788,20.9662653578534));
#23472=CARTESIAN_POINT('Ctrl Pts',(8.49275934044528,0.636078948397367,21.1647814752652));
#23473=CARTESIAN_POINT('Ctrl Pts',(7.17908253400595,-3.04690196012391,21.3632975926768));
#23474=CARTESIAN_POINT('Ctrl Pts',(3.37208816940477,-3.93958786330456,21.5618137100885));
#23475=CARTESIAN_POINT('Ctrl Pts',(0.558149183206385,-1.22447442503984,
21.7603298275001));
#23476=CARTESIAN_POINT('Ctrl Pts',(1.31421753683424,2.61198994621562,21.9588459449118));
#23477=CARTESIAN_POINT('Ctrl Pts',(4.94789989808116,4.05644256154919,22.1573620623234));
#23478=CARTESIAN_POINT('Ctrl Pts',(8.13153968654471,1.78608425229248,22.3558781797351));
#23479=CARTESIAN_POINT('Ctrl Pts',(7.94961898046267,-2.11993989949929,22.5543942971467));
#23480=CARTESIAN_POINT('Ctrl Pts',(4.56873953270021,-4.0845560128934,22.7529104145584));
#23481=CARTESIAN_POINT('Ctrl Pts',(1.08504215066615,-2.30862763082918,22.95142653197));
#23482=CARTESIAN_POINT('Ctrl Pts',(0.688838840573486,1.58152527269752,23.1499426493817));
#23483=CARTESIAN_POINT('Ctrl Pts',(3.74294930484078,4.02329513198439,23.3484587667933));
#23484=CARTESIAN_POINT('Ctrl Pts',(7.45050749686758,2.78070814718547,23.546974884205));
#23485=CARTESIAN_POINT('Ctrl Pts',(8.41614416964521,-1.00859090500303,23.7454910016166));
#23486=CARTESIAN_POINT('Ctrl Pts',(5.75565886205016,-3.87387238340306,23.9440071190283));
#23487=CARTESIAN_POINT('Ctrl Pts',(1.90526000600476,-3.19224361880315,24.14252323644));
#23488=CARTESIAN_POINT('Ctrl Pts',(0.391479031532891,0.414140782493564,
24.3410393538516));
#23489=CARTESIAN_POINT('Ctrl Pts',(2.59982251484541,3.6386490998064,24.5395554712633));
#23490=CARTESIAN_POINT('Ctrl Pts',(6.50943621328541,3.53601506509354,24.7380715886749));
#23491=CARTESIAN_POINT('Ctrl Pts',(8.53753691096405,0.184284815040506,24.9366305620286));
#23492=CARTESIAN_POINT('Ctrl Pts',(7.39923473266516,-2.14788949397592,25.069017496245));
#23493=CARTESIAN_POINT('Ctrl Pts',(6.46213408444902,-2.81539950847165,25.1352323913243));
#23494=CARTESIAN_POINT('Ctrl Pts',(6.0999485000484,3.31089917470656,-0.136624119794918));
#23495=CARTESIAN_POINT('Ctrl Pts',(7.2012096761669,2.76425007587486,-0.0704520806576993));
#23496=CARTESIAN_POINT('Ctrl Pts',(8.79628360522135,0.495054193199949,0.061891997616738));
#23497=CARTESIAN_POINT('Ctrl Pts',(7.22233621477278,-3.38614651265062,0.260408115028396));
#23498=CARTESIAN_POINT('Ctrl Pts',(3.11175417728552,-4.15597244676529,0.458924232440051));
#23499=CARTESIAN_POINT('Ctrl Pts',(0.234536930817258,-1.12501665093665,
0.657440349851707));
#23500=CARTESIAN_POINT('Ctrl Pts',(1.22269767978634,2.93888047390986,0.855956467263361));
#23501=CARTESIAN_POINT('Ctrl Pts',(5.17279897107673,4.31001671203934,1.05447258467502));
#23502=CARTESIAN_POINT('Ctrl Pts',(8.46663102841521,1.73484585358162,1.25298870208667));
#23503=CARTESIAN_POINT('Ctrl Pts',(8.08817274965877,-2.42944129289705,1.45150481949833));
#23504=CARTESIAN_POINT('Ctrl Pts',(4.38379655564558,-4.36869557685114,1.65002093690999));
#23505=CARTESIAN_POINT('Ctrl Pts',(0.746010447431816,-2.30728410002347,
1.84853705432164));
#23506=CARTESIAN_POINT('Ctrl Pts',(0.506172019545635,1.86714771753756,2.04705317173329));
#23507=CARTESIAN_POINT('Ctrl Pts',(3.88395083052018,4.33165331167866,2.24556928914495));
#23508=CARTESIAN_POINT('Ctrl Pts',(7.78602561424836,2.82932772170484,2.4440854065566));
#23509=CARTESIAN_POINT('Ctrl Pts',(8.63895868375428,-1.26404994563383,2.64260152396827));
#23510=CARTESIAN_POINT('Ctrl Pts',(5.66164589758561,-4.19983077212884,2.84111764137992));
#23511=CARTESIAN_POINT('Ctrl Pts',(1.58065589175627,-3.28948852324876,3.03963375879158));
#23512=CARTESIAN_POINT('Ctrl Pts',(0.133280527313607,0.633305814430374,
3.23814987620323));
#23513=CARTESIAN_POINT('Ctrl Pts',(2.6449992344131,3.97613017528841,3.43666599361489));
#23514=CARTESIAN_POINT('Ctrl Pts',(6.81562748453676,3.67769044685756,3.63518211102655));
#23515=CARTESIAN_POINT('Ctrl Pts',(8.82578342391765,0.0112916124882134,
3.8336982284382));
#23516=CARTESIAN_POINT('Ctrl Pts',(6.83460439504253,-3.66544778668689,4.03221434584986));
#23517=CARTESIAN_POINT('Ctrl Pts',(2.66557432085276,-3.98543986826524,4.23073046326151));
#23518=CARTESIAN_POINT('Ctrl Pts',(0.13661161671523,-0.655641908094887,
4.42924658067317));
#23519=CARTESIAN_POINT('Ctrl Pts',(1.56369223320815,3.27458042867263,4.62776269808482));
#23520=CARTESIAN_POINT('Ctrl Pts',(5.63992288139177,4.20600430382654,4.82627881549648));
#23521=CARTESIAN_POINT('Ctrl Pts',(8.63236907507575,1.28564944117731,5.02479493290813));
#23522=CARTESIAN_POINT('Ctrl Pts',(7.80060551073305,-2.81207872246989,5.22331105031979));
#23523=CARTESIAN_POINT('Ctrl Pts',(3.90634543966123,-4.33455868431544,5.42182716773146));
#23524=CARTESIAN_POINT('Ctrl Pts',(0.515878157801087,-1.88753225468275,
5.62034328514309));
#23525=CARTESIAN_POINT('Ctrl Pts',(0.734129108596551,2.28806030889307,5.81885940255477));
#23526=CARTESIAN_POINT('Ctrl Pts',(4.36122822275595,4.36829076522382,6.0173755199664));
#23527=CARTESIAN_POINT('Ctrl Pts',(8.07554712633902,2.44812363240269,6.21589163737808));
#23528=CARTESIAN_POINT('Ctrl Pts',(8.47558322124728,-1.71398855469165,6.41440775478972));
#23529=CARTESIAN_POINT('Ctrl Pts',(5.19499106127511,-4.3064626269354,6.61292387220138));
#23530=CARTESIAN_POINT('Ctrl Pts',(1.2380745430358,-2.9551601430283,6.81143998961304));
#23531=CARTESIAN_POINT('Ctrl Pts',(0.228502545404632,1.10242178675316,7.00995610702469));
#23532=CARTESIAN_POINT('Ctrl Pts',(3.09082189971391,4.15042681451437,7.20847222443635));
#23533=CARTESIAN_POINT('Ctrl Pts',(7.20377498837598,3.39754991503151,7.406988341848));
#23534=CARTESIAN_POINT('Ctrl Pts',(8.80079760945692,-0.466738568384383,
7.60550445925966));
#23535=CARTESIAN_POINT('Ctrl Pts',(6.41936682516261,-3.90359674918315,7.80402057667131));
#23536=CARTESIAN_POINT('Ctrl Pts',(2.24035164813274,-3.7656152813635,8.00253669408298));
#23537=CARTESIAN_POINT('Ctrl Pts',(0.0908146841936848,-0.179154968469096,
8.20105281149462));
#23538=CARTESIAN_POINT('Ctrl Pts',(1.93926099639212,3.57137205666049,8.39956892890629));
#23539=CARTESIAN_POINT('Ctrl Pts',(6.09291861319388,4.05130448700034,8.59808504631793));
#23540=CARTESIAN_POINT('Ctrl Pts',(8.7479469000777,0.821129332128062,8.7966011637296));
#23541=CARTESIAN_POINT('Ctrl Pts',(7.47292145590854,-3.16102044557099,8.99511728114126));
#23542=CARTESIAN_POINT('Ctrl Pts',(3.43548632890085,-4.24836782820074,9.19363339855291));
#23543=CARTESIAN_POINT('Ctrl Pts',(0.333047808208697,-1.44514076628925,
9.39214951596456));
#23544=CARTESIAN_POINT('Ctrl Pts',(1.00676007644372,2.68151871989772,9.59066563337622));
#23545=CARTESIAN_POINT('Ctrl Pts',(4.83965025372247,4.352494370297,9.78918175078787));
#23546=CARTESIAN_POINT('Ctrl Pts',(8.32163042499515,2.03753846960017,9.98769786819953));
#23547=CARTESIAN_POINT('Ctrl Pts',(8.26396938369623,-2.14335640346512,10.1862139856111));
#23548=CARTESIAN_POINT('Ctrl Pts',(4.71947201461794,-4.36140625319899,10.3847301030228));
#23549=CARTESIAN_POINT('Ctrl Pts',(0.934121584873003,-2.58536321899705,
10.5832462204345));
#23550=CARTESIAN_POINT('Ctrl Pts',(0.37447001302165,1.5583062723393,10.7817623378461));
#23551=CARTESIAN_POINT('Ctrl Pts',(3.55303556286365,4.27490852159572,10.9802784552578));
#23552=CARTESIAN_POINT('Ctrl Pts',(7.55894836658157,3.07663086415728,11.1787945726694));
#23553=CARTESIAN_POINT('Ctrl Pts',(8.72366967907197,-0.939166814951776,
11.3773106900811));
#23554=CARTESIAN_POINT('Ctrl Pts',(5.98056987770475,-4.09489338977514,11.5758268074927));
#23555=CARTESIAN_POINT('Ctrl Pts',(1.84172758128094,-3.50059449137405,11.7743429249044));
#23556=CARTESIAN_POINT('Ctrl Pts',(0.0974158357370281,0.299482253859507,
11.9728590423161));
#23557=CARTESIAN_POINT('Ctrl Pts',(2.34504215731444,3.82529884776504,12.1713751597277));
#23558=CARTESIAN_POINT('Ctrl Pts',(6.52627311509865,3.84797952178704,12.3698912771394));
#23559=CARTESIAN_POINT('Ctrl Pts',(8.81201693339725,0.346753746088307,12.568407394551));
#23560=CARTESIAN_POINT('Ctrl Pts',(7.10903290287004,-3.47202251432246,12.7669235119627));
#23561=CARTESIAN_POINT('Ctrl Pts',(2.97688140448274,-4.11118660098796,12.9654396293744));
#23562=CARTESIAN_POINT('Ctrl Pts',(0.199708178602426,-0.985404201530036,
13.163955746786));
#23563=CARTESIAN_POINT('Ctrl Pts',(1.32079563805398,3.0427926213136,13.3624718641977));
#23564=CARTESIAN_POINT('Ctrl Pts',(5.3134732128164,4.28445784161121,13.5609879816093));
#23565=CARTESIAN_POINT('Ctrl Pts',(8.52132272870291,1.60249806959112,13.759504099021));
#23566=CARTESIAN_POINT('Ctrl Pts',(8.00665661883263,-2.546998951815,13.9580202164326));
#23567=CARTESIAN_POINT('Ctrl Pts',(4.24079631663729,-4.36400278220629,14.1565363338443));
#23568=CARTESIAN_POINT('Ctrl Pts',(0.672445052608722,-2.18453587678811,
14.3550524512559));
#23569=CARTESIAN_POINT('Ctrl Pts',(0.569431037105937,1.99548743031406,14.5535685686676));
#23570=CARTESIAN_POINT('Ctrl Pts',(4.02609254599198,4.3480813069304,14.7520846860792));
#23571=CARTESIAN_POINT('Ctrl Pts',(7.87688472210303,2.7187850319364,14.9506008034909));
#23572=CARTESIAN_POINT('Ctrl Pts',(8.59532534039074,-1.40032285852991,15.1491169209026));
#23573=CARTESIAN_POINT('Ctrl Pts',(5.52348014881688,-4.2370417121197,15.3476330383142));
#23574=CARTESIAN_POINT('Ctrl Pts',(1.47448654113341,-3.19355836282975,15.5461491557259));
#23575=CARTESIAN_POINT('Ctrl Pts',(0.156335843231577,0.774524987218279,
15.7446652731375));
#23576=CARTESIAN_POINT('Ctrl Pts',(2.77616539036498,4.03331308699926,15.9431813905492));
#23577=CARTESIAN_POINT('Ctrl Pts',(6.93478511771097,3.59846978345639,16.1416975079608));
#23578=CARTESIAN_POINT('Ctrl Pts',(8.82381018430121,-0.131783697622486,
16.3402136253725));
#23579=CARTESIAN_POINT('Ctrl Pts',(6.71330736721926,-3.74135217521042,16.5387297427841));
#23580=CARTESIAN_POINT('Ctrl Pts',(2.53603500032833,-3.92466149880528,16.7372458601958));
#23581=CARTESIAN_POINT('Ctrl Pts',(0.117459657081213,-0.513840476771981,
16.9357619776075));
#23582=CARTESIAN_POINT('Ctrl Pts',(1.6724666306423,3.3675458796068,17.1342780950191));
#23583=CARTESIAN_POINT('Ctrl Pts',(5.77701011399349,4.16499777695671,17.3327942124308));
#23584=CARTESIAN_POINT('Ctrl Pts',(8.67222726177754,1.14822393682795,17.5313103298424));
#23585=CARTESIAN_POINT('Ctrl Pts',(7.70673328292373,-2.92007154311226,17.7298264472541));
#23586=CARTESIAN_POINT('Ctrl Pts',(3.76470919762329,-4.31422104952143,17.9283425646657));
#23587=CARTESIAN_POINT('Ctrl Pts',(0.456185677945633,-1.75748898396369,
18.1268586820774));
#23588=CARTESIAN_POINT('Ctrl Pts',(0.811045628420214,2.40871806212022,18.3253747994891));
#23589=CARTESIAN_POINT('Ctrl Pts',(4.50431505655582,4.36906692559506,18.5238909169007));
#23590=CARTESIAN_POINT('Ctrl Pts',(8.153768073497,2.32830740706619,18.7224070343124));
#23591=CARTESIAN_POINT('Ctrl Pts',(8.41730502629147,-1.84467174573349,18.920923151724));
#23592=CARTESIAN_POINT('Ctrl Pts',(5.05358378656449,-4.328335603201,19.1194392691357));
#23593=CARTESIAN_POINT('Ctrl Pts',(1.14303628091464,-2.84819204886657,19.3179553865473));
#23594=CARTESIAN_POINT('Ctrl Pts',(0.266867528478102,1.24027160533984,19.516471503959));
#23595=CARTESIAN_POINT('Ctrl Pts',(3.22745620631011,4.19291811607857,19.7149876213706));
#23596=CARTESIAN_POINT('Ctrl Pts',(7.31355151948446,3.30576997342133,19.9135037387823));
#23597=CARTESIAN_POINT('Ctrl Pts',(8.78318510623113,-0.60873942761753,20.112019856194));
#23598=CARTESIAN_POINT('Ctrl Pts',(6.29049448270258,-3.96577684195559,20.3105359736056));
#23599=CARTESIAN_POINT('Ctrl Pts',(2.11823830688215,-3.69103125832118,20.5090520910173));
#23600=CARTESIAN_POINT('Ctrl Pts',(0.0872894180178925,-0.0361094652841183,
20.7075682084289));
#23601=CARTESIAN_POINT('Ctrl Pts',(2.05755217931839,3.65188070090475,20.9060843258406));
#23602=CARTESIAN_POINT('Ctrl Pts',(6.2246974255821,3.99554796485774,21.1046004432522));
#23603=CARTESIAN_POINT('Ctrl Pts',(8.77253282078492,0.680168449111409,21.3031165606639));
#23604=CARTESIAN_POINT('Ctrl Pts',(7.36779915003431,-3.25809647691284,21.5016326780756));
#23605=CARTESIAN_POINT('Ctrl Pts',(3.29692483597213,-4.21265846617502,21.7001487954872));
#23606=CARTESIAN_POINT('Ctrl Pts',(0.287939047401517,-1.30934826998177,
21.8986649128989));
#23607=CARTESIAN_POINT('Ctrl Pts',(1.09641390858805,2.79303874980958,22.0971810303105));
#23608=CARTESIAN_POINT('Ctrl Pts',(4.98196318268333,4.33761289058522,22.2956971477222));
#23609=CARTESIAN_POINT('Ctrl Pts',(8.38627540352384,1.90988580729624,22.4942132651338));
#23610=CARTESIAN_POINT('Ctrl Pts',(8.19174495281671,-2.26688249514424,22.6927293825455));
#23611=CARTESIAN_POINT('Ctrl Pts',(4.57652150231426,-4.36767501203749,22.8912454999571));
#23612=CARTESIAN_POINT('Ctrl Pts',(0.851353342793238,-2.46864902413938,
23.0897616173688));
#23613=CARTESIAN_POINT('Ctrl Pts',(0.42768739434844,1.69114792223732,23.2882777347804));
#23614=CARTESIAN_POINT('Ctrl Pts',(3.69349202933814,4.30216786317793,23.4867938521921));
#23615=CARTESIAN_POINT('Ctrl Pts',(7.65803780123451,2.9734515702302,23.6853099696038));
#23616=CARTESIAN_POINT('Ctrl Pts',(8.6906071069521,-1.07850088950778,23.8838260870154));
#23617=CARTESIAN_POINT('Ctrl Pts',(5.84571156354535,-4.14238794997599,24.0823422044271));
#23618=CARTESIAN_POINT('Ctrl Pts',(1.7284241969769,-3.41351242146536,24.2808583218387));
#23619=CARTESIAN_POINT('Ctrl Pts',(0.109716235810993,0.442846747958131,
24.4793744392504));
#23620=CARTESIAN_POINT('Ctrl Pts',(2.47112996587446,3.89086027970496,24.677890556662));
#23621=CARTESIAN_POINT('Ctrl Pts',(6.6517366226307,3.78111221715306,24.8764066740737));
#23622=CARTESIAN_POINT('Ctrl Pts',(8.82041412666913,0.197058426719993,25.0749656474274));
#23623=CARTESIAN_POINT('Ctrl Pts',(7.60321109049825,-2.29676940207044,25.2073525816438));
#23624=CARTESIAN_POINT('Ctrl Pts',(6.60115576990582,-3.01054754622974,25.273567476723));
#23625=CARTESIAN_POINT('Ctrl Pts',(6.20648120676596,3.5255164385887,0.00171096560382468));
#23626=CARTESIAN_POINT('Ctrl Pts',(7.37912772202248,2.94343275606714,0.0678830047410433));
#23627=CARTESIAN_POINT('Ctrl Pts',(9.07759664569311,0.527144320628084,0.200227083015481));
#23628=CARTESIAN_POINT('Ctrl Pts',(7.40162371335757,-3.60564141759996,0.398743200427137));
#23629=CARTESIAN_POINT('Ctrl Pts',(3.02458781445768,-4.42536858002973,0.597259317838794));
#23630=CARTESIAN_POINT('Ctrl Pts',(-0.0391348072720899,-1.19794185424409,
0.795775435250448));
#23631=CARTESIAN_POINT('Ctrl Pts',(1.01307994788347,3.12938294858669,0.994291552662105));
#23632=CARTESIAN_POINT('Ctrl Pts',(5.21923250695947,4.58939821694615,1.19280767007376));
#23633=CARTESIAN_POINT('Ctrl Pts',(8.72657551299543,1.84730106611042,1.39132378748542));
#23634=CARTESIAN_POINT('Ctrl Pts',(8.32358502229467,-2.58692118447061,1.58983990489707));
#23635=CARTESIAN_POINT('Ctrl Pts',(4.37908581601258,-4.65188073047965,1.78835602230873));
#23636=CARTESIAN_POINT('Ctrl Pts',(0.505493161016087,-2.45684558601761,
1.98687213972038));
#23637=CARTESIAN_POINT('Ctrl Pts',(0.250108060020668,1.98817892786946,2.18538825713204));
#23638=CARTESIAN_POINT('Ctrl Pts',(3.8468393694429,4.61243733220712,2.38390437454369));
#23639=CARTESIAN_POINT('Ctrl Pts',(8.0018522734089,3.01272882884126,2.58242049195535));
#23640=CARTESIAN_POINT('Ctrl Pts',(8.91007369571349,-1.34598748780205,2.78093660936701));
#23641=CARTESIAN_POINT('Ctrl Pts',(5.73976719690925,-4.47206986535408,2.97945272677866));
#23642=CARTESIAN_POINT('Ctrl Pts',(1.39424152787623,-3.50271791779653,3.17796884419032));
#23643=CARTESIAN_POINT('Ctrl Pts',(-0.146954797017362,0.674357611516781,
3.37648496160198));
#23644=CARTESIAN_POINT('Ctrl Pts',(2.5275771424141,4.23386867290823,3.57500107901363));
#23645=CARTESIAN_POINT('Ctrl Pts',(6.96855153613195,3.91608365047424,3.77351719642529));
#23646=CARTESIAN_POINT('Ctrl Pts',(9.10900868522111,0.0120235511094912,
3.97203331383693));
#23647=CARTESIAN_POINT('Ctrl Pts',(6.98875855737045,-3.90304740339865,4.17054943124861));
#23648=CARTESIAN_POINT('Ctrl Pts',(2.54948593565754,-4.24378183362265,4.36906554866025));
#23649=CARTESIAN_POINT('Ctrl Pts',(-0.143407781592193,-0.698141563015474,
4.56758166607191));
#23650=CARTESIAN_POINT('Ctrl Pts',(1.37617826049345,3.48684345900968,4.76609778348356));
#23651=CARTESIAN_POINT('Ctrl Pts',(5.71663606344787,4.47864357428809,4.96461390089523));
#23652=CARTESIAN_POINT('Ctrl Pts',(8.90305693908813,1.36898709382619,5.16313001830687));
#23653=CARTESIAN_POINT('Ctrl Pts',(8.01737725983028,-2.99436172457643,5.36164613571854));
#23654=CARTESIAN_POINT('Ctrl Pts',(3.87068562947579,-4.61553103529222,5.56016225313019));
#23655=CARTESIAN_POINT('Ctrl Pts',(0.260443364168955,-2.00988482013811,
5.75867837054185));
#23656=CARTESIAN_POINT('Ctrl Pts',(0.492841656646439,2.436375680996,5.95719448795349));
#23657=CARTESIAN_POINT('Ctrl Pts',(4.35505457120696,4.6514496783783,6.15571060536516));
#23658=CARTESIAN_POINT('Ctrl Pts',(8.31014098784587,2.60681454019155,6.35422672277681));
#23659=CARTESIAN_POINT('Ctrl Pts',(8.73610799988966,-1.82509176699825,6.55274284018847));
#23660=CARTESIAN_POINT('Ctrl Pts',(5.24286312047947,-4.58561375091533,6.75125895760012));
#23661=CARTESIAN_POINT('Ctrl Pts',(1.02945356160573,-3.14671788935761,6.94977507501179));
#23662=CARTESIAN_POINT('Ctrl Pts',(-0.0455603502579819,1.17388235834786,
7.14829119242343));
#23663=CARTESIAN_POINT('Ctrl Pts',(3.00229867643747,4.41946347189101,7.34680730983509));
#23664=CARTESIAN_POINT('Ctrl Pts',(7.38185932147204,3.61778400498435,7.54532342724674));
#23665=CARTESIAN_POINT('Ctrl Pts',(9.08240325419932,-0.496993236137507,
7.7438395446584));
#23666=CARTESIAN_POINT('Ctrl Pts',(6.5466046888036,-4.15663352541875,7.94235566207006));
#23667=CARTESIAN_POINT('Ctrl Pts',(2.09669971547073,-4.00970789967487,8.1408717794817));
#23668=CARTESIAN_POINT('Ctrl Pts',(-0.192173337388976,-0.19076805214061,
8.33938789689338));
#23669=CARTESIAN_POINT('Ctrl Pts',(1.77609193305126,3.80287354875093,8.53790401430502));
#23670=CARTESIAN_POINT('Ctrl Pts',(6.1989956324977,4.3139158920216,8.73642013171668));
#23671=CARTESIAN_POINT('Ctrl Pts',(9.0261266855466,0.874356120760312,8.93493624912834));
#23672=CARTESIAN_POINT('Ctrl Pts',(7.66845225155073,-3.36592235387631,9.13345236653999));
#23673=CARTESIAN_POINT('Ctrl Pts',(3.36930475145732,-4.52375316346519,9.33196848395166));
#23674=CARTESIAN_POINT('Ctrl Pts',(0.0657616873951493,-1.53881687686219,
9.53048460136329));
#23675=CARTESIAN_POINT('Ctrl Pts',(0.783144957380055,2.85533863417045,9.72900071877498));
#23676=CARTESIAN_POINT('Ctrl Pts',(4.86448860883662,4.63462933832978,9.92751683618659));
#23677=CARTESIAN_POINT('Ctrl Pts',(8.57217576114917,2.16961465444475,10.1260329535983));
#23678=CARTESIAN_POINT('Ctrl Pts',(8.51077704791793,-2.28229185953398,10.3245490710099));
#23679=CARTESIAN_POINT('Ctrl Pts',(4.73652024279266,-4.644118902346,10.5230651884216));
#23680=CARTESIAN_POINT('Ctrl Pts',(0.705797933930029,-2.75295019489822,
10.7215813058332));
#23681=CARTESIAN_POINT('Ctrl Pts',(0.109868939318185,1.65931793437198,10.9200974232449));
#23682=CARTESIAN_POINT('Ctrl Pts',(3.49447369645122,4.55201426291826,11.1186135406565));
#23683=CARTESIAN_POINT('Ctrl Pts',(7.76005555075585,3.27606251797663,11.3171296580682));
#23684=CARTESIAN_POINT('Ctrl Pts',(9.00027578003045,-1.00004496361109,11.5156457754798));
#23685=CARTESIAN_POINT('Ctrl Pts',(6.07936428979557,-4.36033029039609,11.7141618928915));
#23686=CARTESIAN_POINT('Ctrl Pts',(1.67223626118035,-3.72750807951321,11.9126780103032));
#23687=CARTESIAN_POINT('Ctrl Pts',(-0.185144289673645,0.31889512586586,
12.1111941277148));
#23688=CARTESIAN_POINT('Ctrl Pts',(2.20817641458127,4.07326024100545,12.3097102451265));
#23689=CARTESIAN_POINT('Ctrl Pts',(6.66044079877556,4.09741110905781,12.5082263625381));
#23690=CARTESIAN_POINT('Ctrl Pts',(9.09434983091284,0.369230824458725,12.7067424799498));
#23691=CARTESIAN_POINT('Ctrl Pts',(7.28097591722075,-3.69708402566464,12.9052585973614));
#23692=CARTESIAN_POINT('Ctrl Pts',(2.8809723938291,-4.37767965107946,13.1037747147731));
#23693=CARTESIAN_POINT('Ctrl Pts',(-0.0762212094817758,-1.04927952433239,
13.3022908321848));
#23694=CARTESIAN_POINT('Ctrl Pts',(1.11753675741321,3.24003083138531,13.5008069495964));
#23695=CARTESIAN_POINT('Ctrl Pts',(5.369025456116,4.5621825836419,13.6993230670081));
#23696=CARTESIAN_POINT('Ctrl Pts',(8.78481240824481,1.70637430771384,13.8978391844197));
#23697=CARTESIAN_POINT('Ctrl Pts',(8.23678489819753,-2.71209910053747,14.0963553018314));
#23698=CARTESIAN_POINT('Ctrl Pts',(4.22681609508684,-4.64688374211174,14.294871419243));
#23699=CARTESIAN_POINT('Ctrl Pts',(0.427159151106815,-2.32614064576156,
14.4933875366547));
#23700=CARTESIAN_POINT('Ctrl Pts',(0.317467618415429,2.12483780609018,14.6919036540663));
#23701=CARTESIAN_POINT('Ctrl Pts',(3.99819491609722,4.62993021382537,14.890419771478));
#23702=CARTESIAN_POINT('Ctrl Pts',(8.09860099979244,2.8950206023505,15.0889358888896));
#23703=CARTESIAN_POINT('Ctrl Pts',(8.86361197604717,-1.49109380762589,15.2874520063013));
#23704=CARTESIAN_POINT('Ctrl Pts',(5.59264534485911,-4.5116928721902,15.485968123713));
#23705=CARTESIAN_POINT('Ctrl Pts',(1.2811901266875,-3.40056942590122,15.6844842411246));
#23706=CARTESIAN_POINT('Ctrl Pts',(-0.122405002240585,0.824730814938715,
15.8830003585363));
#23707=CARTESIAN_POINT('Ctrl Pts',(2.66724567793686,4.29475826350135,16.0815164759479));
#23708=CARTESIAN_POINT('Ctrl Pts',(7.09543313909595,3.83172778931411,16.2800325933596));
#23709=CARTESIAN_POINT('Ctrl Pts',(9.10690753736432,-0.140326107135887,
16.4785487107712));
#23710=CARTESIAN_POINT('Ctrl Pts',(6.85959888110794,-3.98387202395643,16.6770648281829));
#23711=CARTESIAN_POINT('Ctrl Pts',(2.41154968938301,-4.179063722519,16.8755809455945));
#23712=CARTESIAN_POINT('Ctrl Pts',(-0.163801198896094,-0.547148358219792,
17.0740970630062));
#23713=CARTESIAN_POINT('Ctrl Pts',(1.49200357138825,3.5858350646717,17.2726131804178));
#23714=CARTESIAN_POINT('Ctrl Pts',(5.86260948835618,4.43497894515246,17.4711292978295));
#23715=CARTESIAN_POINT('Ctrl Pts',(8.94549879098837,1.22265346990726,17.6696454152412));
#23716=CARTESIAN_POINT('Ctrl Pts',(7.91742009870712,-3.10935479574357,17.8681615326528));
#23717=CARTESIAN_POINT('Ctrl Pts',(3.71986832177296,-4.59387508565289,18.0666776500645));
#23718=CARTESIAN_POINT('Ctrl Pts',(0.196881531601468,-1.87141195688986,
18.2651937674761));
#23719=CARTESIAN_POINT('Ctrl Pts',(0.574744016316265,2.56485464396025,18.4637098848878));
#23720=CARTESIAN_POINT('Ctrl Pts',(4.50741650012369,4.6522761505852,18.6622260022994));
#23721=CARTESIAN_POINT('Ctrl Pts',(8.3934323297128,2.47923165417059,18.8607421197111));
#23722=CARTESIAN_POINT('Ctrl Pts',(8.67405212821057,-1.96424603112833,19.0592582371228));
#23723=CARTESIAN_POINT('Ctrl Pts',(5.09228962209667,-4.60890456507674,19.2577743545344));
#23724=CARTESIAN_POINT('Ctrl Pts',(0.928254782143413,-3.0328159689208,19.4562904719461));
#23725=CARTESIAN_POINT('Ctrl Pts',(-0.00470849360073685,1.32066780116548,
19.6548065893577));
#23726=CARTESIAN_POINT('Ctrl Pts',(3.14778981602278,4.46470912096001,19.8533227067694));
#23727=CARTESIAN_POINT('Ctrl Pts',(7.49875172579254,3.52005475507203,20.051838824181));
#23728=CARTESIAN_POINT('Ctrl Pts',(9.06364908309027,-0.648198796048447,
20.2503549415927));
#23729=CARTESIAN_POINT('Ctrl Pts',(6.4093786550744,-4.22284422156345,20.4488710590044));
#23730=CARTESIAN_POINT('Ctrl Pts',(1.96667081116617,-3.93028923259476,20.647387176416));
#23731=CARTESIAN_POINT('Ctrl Pts',(-0.195927116407106,-0.0384501329489085,
20.8459032938277));
#23732=CARTESIAN_POINT('Ctrl Pts',(1.90205092121151,3.88860087953163,21.0444194112393));
#23733=CARTESIAN_POINT('Ctrl Pts',(6.3393165377314,4.25454515162759,21.242935528651));
#23734=CARTESIAN_POINT('Ctrl Pts',(9.05230630112455,0.724257949825445,21.4414516460626));
#23735=CARTESIAN_POINT('Ctrl Pts',(7.55651576606266,-3.46929099370176,21.6399677634743));
#23736=CARTESIAN_POINT('Ctrl Pts',(3.22176150253947,-4.48572906904549,21.838483880886));
#23737=CARTESIAN_POINT('Ctrl Pts',(0.0177289115966501,-1.39422211492368,
22.0369999982976));
#23738=CARTESIAN_POINT('Ctrl Pts',(0.878610280341868,2.97408755340353,22.2355161157093));
#23739=CARTESIAN_POINT('Ctrl Pts',(5.01602646728549,4.61878321962123,22.4340322331209));
#23740=CARTESIAN_POINT('Ctrl Pts',(8.64101112050298,2.03368736229999,22.6325483505326));
#23741=CARTESIAN_POINT('Ctrl Pts',(8.43387092517075,-2.41382509078919,22.8310644679442));
#23742=CARTESIAN_POINT('Ctrl Pts',(4.58430347192829,-4.65079401118156,23.0295805853559));
#23743=CARTESIAN_POINT('Ctrl Pts',(0.617664534920323,-2.6286704174496,23.2280967027675));
#23744=CARTESIAN_POINT('Ctrl Pts',(0.166535948123391,1.80077057177711,23.4266128201792));
#23745=CARTESIAN_POINT('Ctrl Pts',(3.64403475383551,4.58104059437149,23.6251289375908));
#23746=CARTESIAN_POINT('Ctrl Pts',(7.86556810560143,3.16619499327494,23.8236450550025));
#23747=CARTESIAN_POINT('Ctrl Pts',(8.96507004425898,-1.14841087401253,24.0221611724142));
#23748=CARTESIAN_POINT('Ctrl Pts',(5.93576426504054,-4.41090351654891,24.2206772898258));
#23749=CARTESIAN_POINT('Ctrl Pts',(1.55158838794904,-3.63478122412758,24.4191934072375));
#23750=CARTESIAN_POINT('Ctrl Pts',(-0.172046559910909,0.471552713422697,
24.6177095246491));
#23751=CARTESIAN_POINT('Ctrl Pts',(2.34243741690352,4.14307145960353,24.8162256420608));
#23752=CARTESIAN_POINT('Ctrl Pts',(6.79403703197597,4.02620936921257,25.0147417594724));
#23753=CARTESIAN_POINT('Ctrl Pts',(9.10329134237422,0.209832038399488,25.2133007328261));
#23754=CARTESIAN_POINT('Ctrl Pts',(7.80718744833136,-2.44564931016495,25.3456876670425));
#23755=CARTESIAN_POINT('Ctrl Pts',(6.7401774553626,-3.20569558398784,25.4119025621217));
#23756=CARTESIAN_POINT('Ctrl Pts',(6.28979540306975,-2.65047774028997,2.34187669256869E-16));
#23757=CARTESIAN_POINT('Ctrl Pts',(6.07824975460912,-2.79680313454321,0.0168403156216635));
#23758=CARTESIAN_POINT('Ctrl Pts',(5.84989216698747,-2.91731508079941,0.0345979173544468));
#23759=CARTESIAN_POINT('Ctrl Pts',(5.51500906830149,-3.04563029082768,0.0584806141104239));
#23760=CARTESIAN_POINT('Ctrl Pts',(5.41879312933457,-3.07738628407187,0.0651272920591958));
#23761=CARTESIAN_POINT('Ctrl Pts',(5.2796709515883,-3.11613828015728,0.0744133179630824));
#23762=CARTESIAN_POINT('Ctrl Pts',(5.23787838666673,-3.12688005475488,0.0771625196878118));
#23763=CARTESIAN_POINT('Ctrl Pts',(5.16290892864459,-3.14455210035684,0.0820236116212797));
#23764=CARTESIAN_POINT('Ctrl Pts',(5.12981532258863,-3.15180426839707,0.0841452115614535));
#23765=CARTESIAN_POINT('Ctrl Pts',(5.07951773377748,-3.16199813479694,0.0873343454331657));
#23766=CARTESIAN_POINT('Ctrl Pts',(5.06239487350367,-3.1653239613259,0.0884138587685488));
#23767=CARTESIAN_POINT('Ctrl Pts',(5.0313026349073,-3.17110155867653,0.0903631796000517));
#23768=CARTESIAN_POINT('Ctrl Pts',(5.01734256342,-3.17360042478014,0.0912344378453712));
#23769=CARTESIAN_POINT('Ctrl Pts',(4.98724043292739,-3.17878390500948,0.0931048058941783));
#23770=CARTESIAN_POINT('Ctrl Pts',(4.97109345313393,-3.18143790017822,0.0941029416431362));
#23771=CARTESIAN_POINT('Ctrl Pts',(4.92727497325308,-3.18829778367847,0.0967981379299586));
#23772=CARTESIAN_POINT('Ctrl Pts',(4.89956738031451,-3.19226642284397,0.0984878499755184));
#23773=CARTESIAN_POINT('Ctrl Pts',(4.75398224404875,-3.21118694447669,0.107295236621157));
#23774=CARTESIAN_POINT('Ctrl Pts',(4.63538973943275,-3.21997319506732,0.114221706112698));
#23775=CARTESIAN_POINT('Ctrl Pts',(4.30095042759944,-3.22621149833508,0.13337700064414));
#23776=CARTESIAN_POINT('Ctrl Pts',(4.08547929171809,-3.20858045444597,0.145250495204097));
#23777=CARTESIAN_POINT('Ctrl Pts',(3.80133532677102,-3.156308727449,0.161766932561653));
#23778=CARTESIAN_POINT('Ctrl Pts',(3.72975840286589,-3.14060110737571,0.166006889533671));
#23779=CARTESIAN_POINT('Ctrl Pts',(3.61736503521311,-3.11188839215322,0.172876824823414));
#23780=CARTESIAN_POINT('Ctrl Pts',(3.57616339916112,-3.1004848786294,0.175441320926198));
#23781=CARTESIAN_POINT('Ctrl Pts',(3.52227753763667,-3.08441009116031,0.178870895262747));
#23782=CARTESIAN_POINT('Ctrl Pts',(3.50937666961836,-3.08047324277195,0.179697728734765));
#23783=CARTESIAN_POINT('Ctrl Pts',(3.48839742123833,-3.07392694119639,0.1810522852053));
#23784=CARTESIAN_POINT('Ctrl Pts',(3.48030382138514,-3.07136630181977,0.181577288984605));
#23785=CARTESIAN_POINT('Ctrl Pts',(3.46464166595954,-3.06634297482279,0.182598119865996));
#23786=CARTESIAN_POINT('Ctrl Pts',(3.45707206542002,-3.06388421131902,0.183093728839097));
#23787=CARTESIAN_POINT('Ctrl Pts',(3.43874556002866,-3.05785624189087,0.184299002209445));
#23788=CARTESIAN_POINT('Ctrl Pts',(3.42799835660854,-3.05425832581353,0.185010290454013));
#23789=CARTESIAN_POINT('Ctrl Pts',(3.39175714586998,-3.04191263431934,0.187423497374185));
#23790=CARTESIAN_POINT('Ctrl Pts',(3.36635472913545,-3.0329020045397,0.189139518999491));
#23791=CARTESIAN_POINT('Ctrl Pts',(3.18676606562611,-2.9666515504672,0.20143179357128));
#23792=CARTESIAN_POINT('Ctrl Pts',(3.03706086767606,-2.89800574240346,0.212511569449416));
#23793=CARTESIAN_POINT('Ctrl Pts',(2.75593821241035,-2.74207447322503,0.234233226407782));
#23794=CARTESIAN_POINT('Ctrl Pts',(2.6243541678938,-2.65596297714111,0.244842751365906));
#23795=CARTESIAN_POINT('Ctrl Pts',(2.40483061592065,-2.48819488821331,0.263043278354808));
#23796=CARTESIAN_POINT('Ctrl Pts',(2.31417740986267,-2.41058629886545,0.270735581712772));
#23797=CARTESIAN_POINT('Ctrl Pts',(2.2084003264213,-2.30933806977478,0.27993104622173));
#23798=CARTESIAN_POINT('Ctrl Pts',(2.1890133115413,-2.29030562382644,0.281626447688871));
#23799=CARTESIAN_POINT('Ctrl Pts',(2.15865709979275,-2.25974128583443,0.284297867569297));
#23800=CARTESIAN_POINT('Ctrl Pts',(2.14752900807433,-2.24836970567203,0.285280840394977));
#23801=CARTESIAN_POINT('Ctrl Pts',(2.1267340987307,-2.22680257934588,0.287124882972914));
#23802=CARTESIAN_POINT('Ctrl Pts',(2.11704888995185,-2.21662536168207,0.287986737897884));
#23803=CARTESIAN_POINT('Ctrl Pts',(2.09536992067828,-2.1935447400592,0.289922870727941));
#23804=CARTESIAN_POINT('Ctrl Pts',(2.08341472592883,-2.18060560805158,0.290995491095302));
#23805=CARTESIAN_POINT('Ctrl Pts',(2.05301110921061,-2.14715353240371,0.293736531578305));
#23806=CARTESIAN_POINT('Ctrl Pts',(2.03471867019213,-2.12650030132646,0.295398433992035));
#23807=CARTESIAN_POINT('Ctrl Pts',(1.88234579830737,-1.9499458084177,0.309358858105313));
#23808=CARTESIAN_POINT('Ctrl Pts',(1.76319789510205,-1.78177019902244,0.3210139179675));
#23809=CARTESIAN_POINT('Ctrl Pts',(1.58764529498356,-1.47568089556482,0.340776631952162));
#23810=CARTESIAN_POINT('Ctrl Pts',(1.52325019859249,-1.34313346058477,0.348939672724235));
#23811=CARTESIAN_POINT('Ctrl Pts',(1.44230346334175,-1.14266590260818,0.361295114701718));
#23812=CARTESIAN_POINT('Ctrl Pts',(1.41852858174535,-1.07786645243649,0.365291698488638));
#23813=CARTESIAN_POINT('Ctrl Pts',(1.3840003923293,-0.973513071877454,0.371804634554866));
#23814=CARTESIAN_POINT('Ctrl Pts',(1.37188904586178,-0.934428807614549,
0.374260799611263));
#23815=CARTESIAN_POINT('Ctrl Pts',(1.35689880148942,-0.882582572681532,
0.377553881129702));
#23816=CARTESIAN_POINT('Ctrl Pts',(1.353348278791,-0.870016774840268,0.378354696523691));
#23817=CARTESIAN_POINT('Ctrl Pts',(1.34764524460579,-0.849353844300361,
0.379676458285701));
#23818=CARTESIAN_POINT('Ctrl Pts',(1.34544773269429,-0.841269139498996,
0.380194850194701));
#23819=CARTESIAN_POINT('Ctrl Pts',(1.34121604497553,-0.825457311698112,
0.381211273027812));
#23820=CARTESIAN_POINT('Ctrl Pts',(1.3391790561386,-0.817731097122878,0.381709141636219));
#23821=CARTESIAN_POINT('Ctrl Pts',(1.33468755813399,-0.800434350578908,
0.382826319689283));
#23822=CARTESIAN_POINT('Ctrl Pts',(1.33224828992365,-0.790859955080673,
0.383446487637849));
#23823=CARTESIAN_POINT('Ctrl Pts',(1.32393629749912,-0.75759584165232,0.385606885925548));
#23824=CARTESIAN_POINT('Ctrl Pts',(1.31828885549605,-0.733851407024439,
0.387159129623654));
#23825=CARTESIAN_POINT('Ctrl Pts',(1.2626755135077,-0.487636749627222,0.403343102159934));
#23826=CARTESIAN_POINT('Ctrl Pts',(1.23618781672172,-0.260541477067284,
0.418962728927435));
#23827=CARTESIAN_POINT('Ctrl Pts',(1.23243065565391,0.111194142621663,0.444046930361003));
#23828=CARTESIAN_POINT('Ctrl Pts',(1.24059942131418,0.254907803355904,0.453638284958007));
#23829=CARTESIAN_POINT('Ctrl Pts',(1.26830131528543,0.477725481866437,0.46820130328789));
#23830=CARTESIAN_POINT('Ctrl Pts',(1.28126951186522,0.557444978040998,0.473351480650301));
#23831=CARTESIAN_POINT('Ctrl Pts',(1.30194285132137,0.660040507109251,0.479904653015137));
#23832=CARTESIAN_POINT('Ctrl Pts',(1.30692718052677,0.683428907810724,0.481393548603338));
#23833=CARTESIAN_POINT('Ctrl Pts',(1.31547759917252,0.721468771378009,0.483807449117055));
#23834=CARTESIAN_POINT('Ctrl Pts',(1.31888693478886,0.736154172267918,0.484737462799632));
#23835=CARTESIAN_POINT('Ctrl Pts',(1.32566686527217,0.764455107891654,0.486526288552673));
#23836=CARTESIAN_POINT('Ctrl Pts',(1.32902353900982,0.778073594161443,0.48738552793633));
#23837=CARTESIAN_POINT('Ctrl Pts',(1.33696390011297,0.809406967195871,0.489359097967962));
#23838=CARTESIAN_POINT('Ctrl Pts',(1.34160979225497,0.827105703792237,0.490471383566467));
#23839=CARTESIAN_POINT('Ctrl Pts',(1.35707337969441,0.884036062422387,0.494041901107027));
#23840=CARTESIAN_POINT('Ctrl Pts',(1.36848374583208,0.923103606732883,0.496480832792461));
#23841=CARTESIAN_POINT('Ctrl Pts',(1.45357435458562,1.19518220536396,0.513409151783491));
#23842=CARTESIAN_POINT('Ctrl Pts',(1.55280772962875,1.41936708491062,0.526981581655514));
#23843=CARTESIAN_POINT('Ctrl Pts',(1.74477144619794,1.74672892300823,0.548187431600153));
#23844=CARTESIAN_POINT('Ctrl Pts',(1.82035847873746,1.858838747653,0.55575927780709));
#23845=CARTESIAN_POINT('Ctrl Pts',(1.92832043772892,1.99908459132599,0.566076921365318));
#23846=CARTESIAN_POINT('Ctrl Pts',(1.95453634583702,2.03179896372779,0.568549147416395));
#23847=CARTESIAN_POINT('Ctrl Pts',(1.99960984760573,2.08585000050386,0.572763008061946));
#23848=CARTESIAN_POINT('Ctrl Pts',(2.01812614747818,2.10746557009875,0.574484240749538));
#23849=CARTESIAN_POINT('Ctrl Pts',(2.04439029989786,2.13731633065713,0.57691682031363));
#23850=CARTESIAN_POINT('Ctrl Pts',(2.05189948459756,2.14576098180312,0.577611332813173));
#23851=CARTESIAN_POINT('Ctrl Pts',(2.06478228629329,2.16009612980221,0.578801525782487));
#23852=CARTESIAN_POINT('Ctrl Pts',(2.07013360476026,2.16600646535647,0.579295537778655));
#23853=CARTESIAN_POINT('Ctrl Pts',(2.08054845969122,2.17742384642834,0.580256371139919));
#23854=CARTESIAN_POINT('Ctrl Pts',(2.08560917047652,2.18293304706993,0.580722954137346));
#23855=CARTESIAN_POINT('Ctrl Pts',(2.09935110683142,2.19778866584626,0.581988994081901));
#23856=CARTESIAN_POINT('Ctrl Pts',(2.10806861051188,2.20710112631449,0.582791141795677));
#23857=CARTESIAN_POINT('Ctrl Pts',(2.14111009866999,2.2419802729716,0.585826918297046));
#23858=CARTESIAN_POINT('Ctrl Pts',(2.1657972161716,2.26719759451342,0.588085888836404));
#23859=CARTESIAN_POINT('Ctrl Pts',(2.34770486563578,2.44700788611533,0.604631936191454));
#23860=CARTESIAN_POINT('Ctrl Pts',(2.52000102485704,2.58550114333554,0.619733168426974));
#23861=CARTESIAN_POINT('Ctrl Pts',(2.82158340239779,2.78074273679449,0.643940663509552));
#23862=CARTESIAN_POINT('Ctrl Pts',(2.94285408867079,2.84857123274083,0.653181261672033));
#23863=CARTESIAN_POINT('Ctrl Pts',(3.13955858634984,2.94246980027581,0.667304720540197));
#23864=CARTESIAN_POINT('Ctrl Pts',(3.21222130786266,2.97392518504451,0.672350674394824));
#23865=CARTESIAN_POINT('Ctrl Pts',(3.30823673738015,3.01135367129709,0.67880290808403));
#23866=CARTESIAN_POINT('Ctrl Pts',(3.33059576293847,3.01978439141837,0.680290666522021));
#23867=CARTESIAN_POINT('Ctrl Pts',(3.36729831834166,3.03315918289536,0.682709296296089));
#23868=CARTESIAN_POINT('Ctrl Pts',(3.38158633492913,3.0382519109594,0.68364507372935));
#23869=CARTESIAN_POINT('Ctrl Pts',(3.40930565845442,3.04791199250808,0.685449562534719));
#23870=CARTESIAN_POINT('Ctrl Pts',(3.42273218827009,3.05249189925252,0.68631867114754));
#23871=CARTESIAN_POINT('Ctrl Pts',(3.453847531493,3.06287677042547,0.688321612512623));
#23872=CARTESIAN_POINT('Ctrl Pts',(3.47155738560099,3.06861745057343,0.689453315858022));
#23873=CARTESIAN_POINT('Ctrl Pts',(3.52928504695514,3.08677872506566,0.693116135910914));
#23874=CARTESIAN_POINT('Ctrl Pts',(3.56949652694581,3.0985727461866,0.695626901293803));
#23875=CARTESIAN_POINT('Ctrl Pts',(3.80563017808011,3.16285694558108,0.710155383560904));
#23876=CARTESIAN_POINT('Ctrl Pts',(4.00593161318787,3.19754341870944,0.721581594756166));
#23877=CARTESIAN_POINT('Ctrl Pts',(4.41491592618508,3.22914602457896,0.744544645105131));
#23878=CARTESIAN_POINT('Ctrl Pts',(4.62268116641124,3.22512989545908,0.756035684623915));
#23879=CARTESIAN_POINT('Ctrl Pts',(4.86097535314046,3.19742946533819,0.770350365044164));
#23880=CARTESIAN_POINT('Ctrl Pts',(4.89329945355423,3.19317389942722,0.772317143053407));
#23881=CARTESIAN_POINT('Ctrl Pts',(4.93743154918083,3.18668116842424,0.775043475043542));
#23882=CARTESIAN_POINT('Ctrl Pts',(4.94930102138977,3.18486709826258,0.775780814329541));
#23883=CARTESIAN_POINT('Ctrl Pts',(4.96922863750572,3.18170739816267,0.777026015788556));
#23884=CARTESIAN_POINT('Ctrl Pts',(4.97729242935448,3.18039736001144,0.777531900574851));
#23885=CARTESIAN_POINT('Ctrl Pts',(4.9926217782942,3.17784710159476,0.778497564797928));
#23886=CARTESIAN_POINT('Ctrl Pts',(4.99988823540604,3.17661258833065,0.778957009798921));
#23887=CARTESIAN_POINT('Ctrl Pts',(5.01717103467575,3.17361534294314,0.780053710117017));
#23888=CARTESIAN_POINT('Ctrl Pts',(5.02718332294179,3.17183011428051,0.780692205754548));
#23889=CARTESIAN_POINT('Ctrl Pts',(5.06265609270367,3.1653317918268,0.782965136001058));
#23890=CARTESIAN_POINT('Ctrl Pts',(5.08806727625383,3.16035942076377,0.784613102857243));
#23891=CARTESIAN_POINT('Ctrl Pts',(5.31536599923246,3.11303166670219,0.799514700325313));
#23892=CARTESIAN_POINT('Ctrl Pts',(5.51279641204211,3.05169284891943,0.813566914622217));
#23893=CARTESIAN_POINT('Ctrl Pts',(5.84809026026377,2.91105907337854,0.838134275200583));
#23894=CARTESIAN_POINT('Ctrl Pts',(5.98854849914638,2.83965078211244,0.848672215806842));
#23895=CARTESIAN_POINT('Ctrl Pts',(6.17170786092387,2.7289706073794,0.862579864170383));
#23896=CARTESIAN_POINT('Ctrl Pts',(6.21939794582009,2.69840825166359,0.866219333358702));
#23897=CARTESIAN_POINT('Ctrl Pts',(6.30077041072072,2.64318175420469,0.872461399371499));
#23898=CARTESIAN_POINT('Ctrl Pts',(6.33482388456517,2.61909157455961,0.875083913608399));
#23899=CARTESIAN_POINT('Ctrl Pts',(6.37199826894543,2.59169549764984,0.87795954337468));
#23900=CARTESIAN_POINT('Ctrl Pts',(6.37558956385616,2.58903731045176,0.878237483634976));
#23901=CARTESIAN_POINT('Ctrl Pts',(6.37917532099386,2.58637166203218,0.878515132681521));
#23902=CARTESIAN_POINT('Origin',(4.45646910621825,0.,0.));
#23903=CARTESIAN_POINT('Ctrl Pts',(6.20516358154934,3.52286199445085,6.93889390390723E-16));
#23904=CARTESIAN_POINT('Ctrl Pts',(6.26399827345772,3.49365735888464,0.00332252301440561));
#23905=CARTESIAN_POINT('Ctrl Pts',(6.32201823097654,3.4628755617916,0.00664504602881051));
#23906=CARTESIAN_POINT('Ctrl Pts',(6.37917532067789,3.43058507618661,0.00996756904321544));
#23907=CARTESIAN_POINT('Ctrl Pts',(6.37857781428809,3.43132439655042,0.193274600733303));
#23908=CARTESIAN_POINT('Ctrl Pts',(6.33400076845272,3.45629490883027,0.190678175003209));
#23909=CARTESIAN_POINT('Ctrl Pts',(6.2889659255652,3.48038043910034,0.188081749273116));
#23910=CARTESIAN_POINT('Ctrl Pts',(6.24351184914418,3.50356493231619,0.185485323543022));
#23911=CARTESIAN_POINT('Ctrl Pts',(6.14158456595626,3.55555438170445,0.179663037809694));
#23912=CARTESIAN_POINT('Ctrl Pts',(6.03720488368621,3.6031847036311,0.173840752076367));
#23913=CARTESIAN_POINT('Ctrl Pts',(5.93078566897907,3.64621443044277,0.168018466343039));
#23914=CARTESIAN_POINT('Ctrl Pts',(5.82450213616912,3.68918929540468,0.162203603881687));
#23915=CARTESIAN_POINT('Ctrl Pts',(5.71618462699839,3.72757506957501,0.156388741420336));
#23916=CARTESIAN_POINT('Ctrl Pts',(5.6062707198183,3.76117604604766,0.150573878958984));
#23917=CARTESIAN_POINT('Ctrl Pts',(5.49646629703298,3.79474355284694,0.144764808637259));
#23918=CARTESIAN_POINT('Ctrl Pts',(5.38506903844422,3.82353561660776,0.138955738315534));
#23919=CARTESIAN_POINT('Ctrl Pts',(5.27253590588312,3.84740483683284,0.133146667993808));
#23920=CARTESIAN_POINT('Ctrl Pts',(5.16008059026756,3.87125755143182,0.12734161465889));
#23921=CARTESIAN_POINT('Ctrl Pts',(5.04649137320448,3.89019410488495,0.121536561323971));
#23922=CARTESIAN_POINT('Ctrl Pts',(4.93223904889052,3.90411730889962,0.115731507989053));
#23923=CARTESIAN_POINT('Ctrl Pts',(4.81802731698202,3.91803556617605,0.109928517116146));
#23924=CARTESIAN_POINT('Ctrl Pts',(4.70315336348797,3.92694396305522,0.10412552624324));
#23925=CARTESIAN_POINT('Ctrl Pts',(4.58809612746815,3.93079678020588,0.0983225353703337));
#23926=CARTESIAN_POINT('Ctrl Pts',(4.47305074147543,3.93464920054544,0.0925201421616984));
#23927=CARTESIAN_POINT('Ctrl Pts',(4.35782253127168,3.93344706257557,0.0867177489530631));
#23928=CARTESIAN_POINT('Ctrl Pts',(4.24289266529862,3.92719672334912,0.0809153557444278));
#23929=CARTESIAN_POINT('Ctrl Pts',(4.12794563917741,3.92094545088617,0.0751120961819844));
#23930=CARTESIAN_POINT('Ctrl Pts',(4.013297466179,3.909644502795,0.069308836619541));
#23931=CARTESIAN_POINT('Ctrl Pts',(3.89942559792773,3.89335222268309,0.0635055770570976));
#23932=CARTESIAN_POINT('Ctrl Pts',(3.78544212541581,3.87704397473027,0.0576966297993286));
#23933=CARTESIAN_POINT('Ctrl Pts',(3.67223689416757,3.85573468718041,0.0518876825415597));
#23934=CARTESIAN_POINT('Ctrl Pts',(3.56027855345575,3.82953410914947,0.0460787352837907));
#23935=CARTESIAN_POINT('Ctrl Pts',(3.44826087686546,3.80331964529008,0.0402667093899295));
#23936=CARTESIAN_POINT('Ctrl Pts',(3.33749181154649,3.77220884343344,0.0344546834960684));
#23937=CARTESIAN_POINT('Ctrl Pts',(3.22842443136256,3.73636123475214,0.0286426576022072));
#23938=CARTESIAN_POINT('Ctrl Pts',(3.11919320000295,3.7004597724547,0.0228219003417894));
#23939=CARTESIAN_POINT('Ctrl Pts',(3.01166915181536,3.65980744271886,0.0170011430813716));
#23940=CARTESIAN_POINT('Ctrl Pts',(2.90628516992032,3.61461184135224,0.0111803858209537));
#23941=CARTESIAN_POINT('Ctrl Pts',(2.8392122478765,3.58584654901203,0.00747569378955098));
#23942=CARTESIAN_POINT('Ctrl Pts',(2.77300576585457,3.5552417956376,0.00377100175814821));
#23943=CARTESIAN_POINT('Ctrl Pts',(2.70777160956256,3.52286049471024,6.63097267454378E-5));
#23944=CARTESIAN_POINT('Origin',(4.45646910621825,-5.13094777615093E-16,
-2.31077344927308));
#23945=CARTESIAN_POINT('Ctrl Pts',(2.58488257447924,-2.62360084935057,-3.5527136788005E-15));
#23946=CARTESIAN_POINT('Ctrl Pts',(2.50157068764126,-2.56416901718817,0.00631741419995904));
#23947=CARTESIAN_POINT('Ctrl Pts',(2.4210367769768,-2.50072579486678,0.0126348283999217));
#23948=CARTESIAN_POINT('Ctrl Pts',(2.34367228340277,-2.4335585359717,0.0189522425998843));
#23949=CARTESIAN_POINT('Ctrl Pts',(2.26635227642181,-2.36642989999491,0.02526602412261));
#23950=CARTESIAN_POINT('Ctrl Pts',(2.19219836315962,-2.29558175594025,0.0315798056453355));
#23951=CARTESIAN_POINT('Ctrl Pts',(2.12156918716279,-2.22134192111315,0.0378935871680612));
#23952=CARTESIAN_POINT('Ctrl Pts',(2.05096424093384,-2.14712755471238,0.0442052027096813));
#23953=CARTESIAN_POINT('Ctrl Pts',(1.98388190260799,-2.06952410786498,0.0505168182513019));
#23954=CARTESIAN_POINT('Ctrl Pts',(1.92064376403118,-1.98889602453766,0.0568284337929219));
#23955=CARTESIAN_POINT('Ctrl Pts',(1.85739487416585,-1.90825423340985,0.0631411223895259));
#23956=CARTESIAN_POINT('Ctrl Pts',(1.79799174587117,-1.82458709234475,0.0694538109861296));
#23957=CARTESIAN_POINT('Ctrl Pts',(1.74271535062685,-1.73829172365097,0.0757664995827336));
#23958=CARTESIAN_POINT('Ctrl Pts',(1.68743061602759,-1.65198333587902,0.0820801405524201));
#23959=CARTESIAN_POINT('Ctrl Pts',(1.63627407288981,-1.56304627215329,0.0883937815221068));
#23960=CARTESIAN_POINT('Ctrl Pts',(1.58948251426926,-1.47190537878104,0.0947074224917932));
#23961=CARTESIAN_POINT('Ctrl Pts',(1.54267402606718,-1.38073150986299,0.101023347790164));
#23962=CARTESIAN_POINT('Ctrl Pts',(1.50023385155733,-1.2873525843142,0.107339273088534));
#23963=CARTESIAN_POINT('Ctrl Pts',(1.46235182621787,-1.19221611971277,0.113655198386905));
#23964=CARTESIAN_POINT('Ctrl Pts',(1.42444809981949,-1.09702515533197,0.119974741819887));
#23965=CARTESIAN_POINT('Ctrl Pts',(1.39110787082884,-1.00007502359117,0.126294285252868));
#23966=CARTESIAN_POINT('Ctrl Pts',(1.36247182640407,-0.901830579988466,
0.13261382868585));
#23967=CARTESIAN_POINT('Ctrl Pts',(1.33379348022257,-0.803441007662954,
0.138942707479016));
#23968=CARTESIAN_POINT('Ctrl Pts',(1.3098333100831,-0.703753694545378,0.145271586272182));
#23969=CARTESIAN_POINT('Ctrl Pts',(1.2906814498789,-0.603246282598787,0.151600465065348));
#23970=CARTESIAN_POINT('Ctrl Pts',(1.27151389667214,-0.502656515045226,
0.15793452973132));
#23971=CARTESIAN_POINT('Ctrl Pts',(1.25716256324945,-0.401245709925989,
0.164268594397292));
#23972=CARTESIAN_POINT('Ctrl Pts',(1.24766576452444,-0.299497373668809,
0.170602659063265));
#23973=CARTESIAN_POINT('Ctrl Pts',(1.23815230744814,-0.197570560476596,
0.176947834323174));
#23974=CARTESIAN_POINT('Ctrl Pts',(1.23351041447289,-0.0953054378363929,
0.183293009583083));
#23975=CARTESIAN_POINT('Ctrl Pts',(1.23372630841194,0.00681334627341558,
0.189638184842992));
#23976=CARTESIAN_POINT('Ctrl Pts',(1.23382699866106,0.0544402776128069,
0.192597495699212));
#23977=CARTESIAN_POINT('Ctrl Pts',(1.23498360239768,0.102035435663407,0.195556806555432));
#23978=CARTESIAN_POINT('Ctrl Pts',(1.23719087673066,0.149550137569756,0.198516117411651));
#23979=CARTESIAN_POINT('Ctrl Pts',(1.24174932668504,0.247677220144283,0.204627668765258));
#23980=CARTESIAN_POINT('Ctrl Pts',(1.25080826090224,0.345803872861143,0.210739220118864));
#23981=CARTESIAN_POINT('Ctrl Pts',(1.26437801075032,0.443477170476924,0.21685077147247));
#23982=CARTESIAN_POINT('Ctrl Pts',(1.27792738297975,0.541003792639323,0.22295314514305));
#23983=CARTESIAN_POINT('Ctrl Pts',(1.29597405496826,0.638077977311205,0.229055518813629));
#23984=CARTESIAN_POINT('Ctrl Pts',(1.3184763837669,0.734247394508317,0.235157892484209));
#23985=CARTESIAN_POINT('Ctrl Pts',(1.34095191103269,0.830302268547761,0.241252997886249));
#23986=CARTESIAN_POINT('Ctrl Pts',(1.36787245042669,0.925454087006087,0.24734810328829));
#23987=CARTESIAN_POINT('Ctrl Pts',(1.3991447764821,1.01925733026713,0.25344320869033));
#23988=CARTESIAN_POINT('Ctrl Pts',(1.43038946774705,1.11297768129407,0.259532927957667));
#23989=CARTESIAN_POINT('Ctrl Pts',(1.46597816254694,1.20535140612818,0.265622647225003));
#23990=CARTESIAN_POINT('Ctrl Pts',(1.50576720162495,1.29594592199264,0.27171236649234));
#23991=CARTESIAN_POINT('Ctrl Pts',(1.54553752828296,1.38649783208751,0.27779922182058));
#23992=CARTESIAN_POINT('Ctrl Pts',(1.58950409832805,1.4752717888499,0.28388607714882));
#23993=CARTESIAN_POINT('Ctrl Pts',(1.6374746434305,1.56185395644788,0.28997293247706));
#23994=CARTESIAN_POINT('Ctrl Pts',(1.68543609785703,1.6484197162601,0.296058634313524));
#23995=CARTESIAN_POINT('Ctrl Pts',(1.73739980467476,1.73279412366717,0.302144336149989));
#23996=CARTESIAN_POINT('Ctrl Pts',(1.79312747173125,1.8145878045738,0.308230037986454));
#23997=CARTESIAN_POINT('Ctrl Pts',(1.84886022590844,1.89638895204685,0.314316295358462));
#23998=CARTESIAN_POINT('Ctrl Pts',(1.90835737172213,1.97560853862661,0.32040255273047));
#23999=CARTESIAN_POINT('Ctrl Pts',(1.97133786527822,2.051887004151,0.326488810102477));
#24000=CARTESIAN_POINT('Ctrl Pts',(2.03438354345234,2.12824441765368,0.332581366732233));
#24001=CARTESIAN_POINT('Ctrl Pts',(2.10091948534764,2.20165428819934,0.338673923361988));
#24002=CARTESIAN_POINT('Ctrl Pts',(2.17062515492173,2.27179114198929,0.344766479991743));
#24003=CARTESIAN_POINT('Ctrl Pts',(2.24036729840072,2.34196469530383,0.350862224587877));
#24004=CARTESIAN_POINT('Ctrl Pts',(2.31328214346588,2.40886152281209,0.356957969184011));
#24005=CARTESIAN_POINT('Ctrl Pts',(2.38901484496053,2.47219546963972,0.363053713780146));
#24006=CARTESIAN_POINT('Ctrl Pts',(2.46487788184523,2.53563841369709,0.369159949105304));
#24007=CARTESIAN_POINT('Ctrl Pts',(2.54356810737106,2.59550596129862,0.375266184430463));
#24008=CARTESIAN_POINT('Ctrl Pts',(2.62470032786385,2.65155439415183,0.381372419755621));
#24009=CARTESIAN_POINT('Ctrl Pts',(2.69405651331979,2.69946760890019,0.386592358111516));
#24010=CARTESIAN_POINT('Ctrl Pts',(2.76519663464012,2.74459057588682,0.391812296467411));
#24011=CARTESIAN_POINT('Ctrl Pts',(2.8378668229934,2.78679820066671,0.397032234823306));
#24012=CARTESIAN_POINT('Ctrl Pts',(2.92393480676644,2.8367874087171,0.403214543963986));
#24013=CARTESIAN_POINT('Ctrl Pts',(3.01246905677606,2.8828718115725,0.409396853104666));
#24014=CARTESIAN_POINT('Ctrl Pts',(3.10308063531525,2.92480037085041,0.415579162245345));
#24015=CARTESIAN_POINT('Ctrl Pts',(3.19357013044255,2.966672438655,0.42175314179498));
#24016=CARTESIAN_POINT('Ctrl Pts',(3.28613100122957,3.00439961290741,0.427927121344614));
#24017=CARTESIAN_POINT('Ctrl Pts',(3.38034775723902,3.03777556853218,0.434101100894248));
#24018=CARTESIAN_POINT('Ctrl Pts',(3.47446514659151,3.07111632386696,0.440268568993754));
#24019=CARTESIAN_POINT('Ctrl Pts',(3.57023454316161,3.10011484114296,0.44643603709326));
#24020=CARTESIAN_POINT('Ctrl Pts',(3.66721927955844,3.1246123397339,0.452603505192766));
#24021=CARTESIAN_POINT('Ctrl Pts',(3.76413288446316,3.14909187113027,0.458766449887613));
#24022=CARTESIAN_POINT('Ctrl Pts',(3.86225963847881,3.16907684231919,0.464929394582459));
#24023=CARTESIAN_POINT('Ctrl Pts',(3.96114733242027,3.18445818042905,0.471092339277305));
#24024=CARTESIAN_POINT('Ctrl Pts',(4.05999734800456,3.19983365791532,0.477252935756492));
#24025=CARTESIAN_POINT('Ctrl Pts',(4.15960730024591,3.21060892165472,0.48341353223568));
#24026=CARTESIAN_POINT('Ctrl Pts',(4.25951524489438,3.21672609014344,0.489574128714867));
#24027=CARTESIAN_POINT('Ctrl Pts',(4.35941159768095,3.22284254888507,0.495734010408219));
#24028=CARTESIAN_POINT('Ctrl Pts',(4.45960544222506,3.22430196059119,0.501893892101572));
#24029=CARTESIAN_POINT('Ctrl Pts',(4.55963116203887,3.2210984388464,0.508053773794924));
#24030=CARTESIAN_POINT('Ctrl Pts',(4.65967178229589,3.21789443988542,0.514214573101942));
#24031=CARTESIAN_POINT('Ctrl Pts',(4.75954379554351,3.21002614160735,0.520375372408959));
#24032=CARTESIAN_POINT('Ctrl Pts',(4.85878402884389,3.19753972071225,0.526536171715977));
#24033=CARTESIAN_POINT('Ctrl Pts',(4.95812767066414,3.18504028894183,0.532703390588088));
#24034=CARTESIAN_POINT('Ctrl Pts',(5.05683778779378,3.16791317936909,0.538870609460199));
#24035=CARTESIAN_POINT('Ctrl Pts',(5.15445887658851,3.14625616295914,0.54503782833231));
#24036=CARTESIAN_POINT('Ctrl Pts',(5.2521334743872,3.12458727569841,0.551208427639357));
#24037=CARTESIAN_POINT('Ctrl Pts',(5.34871743723497,3.09838364936585,0.557379026946404));
#24038=CARTESIAN_POINT('Ctrl Pts',(5.44376994753617,3.06779311741076,0.563549626253451));
#24039=CARTESIAN_POINT('Ctrl Pts',(5.53897697405659,3.0371528578543,0.569730256412626));
#24040=CARTESIAN_POINT('Ctrl Pts',(5.63264716982046,3.00211159976873,0.575910886571802));
#24041=CARTESIAN_POINT('Ctrl Pts',(5.72435912365468,2.96286558354997,0.582091516730978));
#24042=CARTESIAN_POINT('Ctrl Pts',(5.79091936345287,2.93438266347866,0.586577128565639));
#24043=CARTESIAN_POINT('Ctrl Pts',(5.85644859621518,2.90368603370804,0.5910627404003));
#24044=CARTESIAN_POINT('Ctrl Pts',(5.92079455746785,2.87086546799437,0.595548352234962));
#24045=CARTESIAN_POINT('Ctrl Pts',(6.00948985732504,2.82562517845972,0.601731377229428));
#24046=CARTESIAN_POINT('Ctrl Pts',(6.09623580561817,2.77619461905173,0.607914402223895));
#24047=CARTESIAN_POINT('Ctrl Pts',(6.18061096190255,2.72276558373602,0.614097427218362));
#24048=CARTESIAN_POINT('Ctrl Pts',(6.24884961276234,2.6795546974131,0.619097966505455));
#24049=CARTESIAN_POINT('Ctrl Pts',(6.31553778122664,2.63372945712145,0.62409850579255));
#24050=CARTESIAN_POINT('Ctrl Pts',(6.38046276496377,2.58541407971855,0.629099045079643));
#24051=CARTESIAN_POINT('Ctrl Pts',(5.88688308661327,2.88166464694226,-0.413294290592403));
#24052=CARTESIAN_POINT('Ctrl Pts',(6.84537358445575,2.40588471549031,-0.347122251455184));
#24053=CARTESIAN_POINT('Ctrl Pts',(8.23365752427788,0.430873938343679,-0.214778173180747));
#24054=CARTESIAN_POINT('Ctrl Pts',(6.86376121760315,-2.94715670275194,-0.0162620557690901));
#24055=CARTESIAN_POINT('Ctrl Pts',(3.28608690294124,-3.61718018023642,0.182254061642566));
#24056=CARTESIAN_POINT('Ctrl Pts',(0.781880406995935,-0.979166244321737,
0.380770179054222));
#24057=CARTESIAN_POINT('Ctrl Pts',(1.64193314359211,2.55787552455616,0.579286296465875));
#24058=CARTESIAN_POINT('Ctrl Pts',(5.07993189931123,3.75125370222575,0.777802413877532));
#24059=CARTESIAN_POINT('Ctrl Pts',(7.94674205925474,1.50993542852403,0.976318531289188));
#24060=CARTESIAN_POINT('Ctrl Pts',(7.61734820438694,-2.11448150974993,1.17483464870084));
#24061=CARTESIAN_POINT('Ctrl Pts',(4.39321803491158,-3.80232526959411,1.3733507661125));
#24062=CARTESIAN_POINT('Ctrl Pts',(1.22704502026327,-2.0081611280352,1.57186688352415));
#24063=CARTESIAN_POINT('Ctrl Pts',(1.01829993859556,1.62508529687376,1.77038300093581));
#24064=CARTESIAN_POINT('Ctrl Pts',(3.95817375267475,3.77008527062174,1.96889911834747));
#24065=CARTESIAN_POINT('Ctrl Pts',(7.35437229592725,2.462525507432,2.16741523575912));
#24066=CARTESIAN_POINT('Ctrl Pts',(8.09672865983581,-1.10017486129741,2.36593135317078));
#24067=CARTESIAN_POINT('Ctrl Pts',(5.50540329893836,-3.65535258567839,2.56444747058243));
#24068=CARTESIAN_POINT('Ctrl Pts',(1.95348461951634,-2.8630297341532,2.76296358799409));
#24069=CARTESIAN_POINT('Ctrl Pts',(0.693751175975549,0.551202220257554,
2.96147970540574));
#24070=CARTESIAN_POINT('Ctrl Pts',(2.87984341841113,3.46065318004877,3.1599958228174));
#24071=CARTESIAN_POINT('Ctrl Pts',(6.50977938134639,3.20090403962421,3.35851194022905));
#24072=CARTESIAN_POINT('Ctrl Pts',(8.25933290131072,0.00982773524565914,
3.55702805764071));
#24073=CARTESIAN_POINT('Ctrl Pts',(6.52629607038668,-3.19024855326339,3.75554417505237));
#24074=CARTESIAN_POINT('Ctrl Pts',(2.89775109124319,-3.46875593755042,3.95406029246402));
#24075=CARTESIAN_POINT('Ctrl Pts',(0.69665041333009,-0.570642598253718,
4.15257640987568));
#24076=CARTESIAN_POINT('Ctrl Pts',(1.93872017863753,2.85005436799852,4.35109252728733));
#24077=CARTESIAN_POINT('Ctrl Pts',(5.48649651727959,3.66072576290342,4.54960864469899));
#24078=CARTESIAN_POINT('Ctrl Pts',(8.09099334705098,1.11897413587954,4.74812476211065));
#24079=CARTESIAN_POINT('Ctrl Pts',(7.36706201253862,-2.44751271825679,4.9466408795223));
#24080=CARTESIAN_POINT('Ctrl Pts',(3.97766506003213,-3.7726139823619,5.14515699693396));
#24081=CARTESIAN_POINT('Ctrl Pts',(1.02674774506536,-1.64282712377203,5.34367311434561));
#24082=CARTESIAN_POINT('Ctrl Pts',(1.21670401249677,1.99142956468722,5.54218923175727));
#24083=CARTESIAN_POINT('Ctrl Pts',(4.37357552585394,3.80197293891488,5.74070534916892));
#24084=CARTESIAN_POINT('Ctrl Pts',(7.60635940332531,2.13074181682499,5.93922146658058));
#24085=CARTESIAN_POINT('Ctrl Pts',(7.95453366396254,-1.49178213007847,6.13773758399224));
#24086=CARTESIAN_POINT('Ctrl Pts',(5.09924694286633,-3.74816037897555,6.33625370140389));
#24087=CARTESIAN_POINT('Ctrl Pts',(1.65531650589596,-2.57204465036969,6.53476981881556));
#24088=CARTESIAN_POINT('Ctrl Pts',(0.776628336729841,0.959500643563771,
6.7332859362272));
#24089=CARTESIAN_POINT('Ctrl Pts',(3.26786834626679,3.6123534997611,6.93180205363886));
#24090=CARTESIAN_POINT('Ctrl Pts',(6.84760632218384,2.95708173512582,7.1303181710505));
#24091=CARTESIAN_POINT('Ctrl Pts',(8.23758631997216,-0.406229232878139,
7.32883428846218));
#24092=CARTESIAN_POINT('Ctrl Pts',(6.16489109788061,-3.39752319671194,7.52735040587382));
#24093=CARTESIAN_POINT('Ctrl Pts',(2.52765551345678,-3.27743004474078,7.72586652328549));
#24094=CARTESIAN_POINT('Ctrl Pts',(0.656790727359,-0.155928801126063,7.92438264069713));
#24095=CARTESIAN_POINT('Ctrl Pts',(2.26559912307384,3.10836907247963,8.1228987581088));
#24096=CARTESIAN_POINT('Ctrl Pts',(5.88076457458627,3.52608167695778,8.32141487552045));
#24097=CARTESIAN_POINT('Ctrl Pts',(8.19158732913988,0.714675754863574,8.5199309929321));
#24098=CARTESIAN_POINT('Ctrl Pts',(7.08185986462416,-2.75121662896035,8.71844711034376));
#24099=CARTESIAN_POINT('Ctrl Pts',(3.56784948378791,-3.69759715767183,8.91696322775543));
#24100=CARTESIAN_POINT('Ctrl Pts',(0.867620049835816,-1.2577885451434,9.11547934516706));
#24101=CARTESIAN_POINT('Ctrl Pts',(1.45399031457103,2.33387889135228,9.31399546257875));
#24102=CARTESIAN_POINT('Ctrl Pts',(4.78997354349419,3.78822443423146,9.51251157999037));
#24103=CARTESIAN_POINT('Ctrl Pts',(7.8205397526871,1.77338609991104,9.71102769740205));
#24104=CARTESIAN_POINT('Ctrl Pts',(7.77035405525285,-1.8654854913274,9.90954381481369));
#24105=CARTESIAN_POINT('Ctrl Pts',(4.68537555826851,-3.79598095490491,10.1080599322253));
#24106=CARTESIAN_POINT('Ctrl Pts',(1.39076888675897,-2.25018926719472,10.306576049637));
#24107=CARTESIAN_POINT('Ctrl Pts',(0.903672160428571,1.35628294827392,10.5050921670486));
#24108=CARTESIAN_POINT('Ctrl Pts',(3.67015929568852,3.72069703895061,10.7036082844603));
#24109=CARTESIAN_POINT('Ctrl Pts',(7.156733998233,2.67776755651859,10.902124401872));
#24110=CARTESIAN_POINT('Ctrl Pts',(8.17045747715504,-0.817410517633158,
11.1006405192836));
#24111=CARTESIAN_POINT('Ctrl Pts',(5.78298105352307,-3.56401958853324,11.2991566366953));
#24112=CARTESIAN_POINT('Ctrl Pts',(2.18071022148213,-3.04676731509573,11.4976727541069));
#24113=CARTESIAN_POINT('Ctrl Pts',(0.662536086558379,0.260656509846819,
11.6961888715186));
#24114=CARTESIAN_POINT('Ctrl Pts',(2.61877364278075,3.32937606128419,11.8947049889302));
#24115=CARTESIAN_POINT('Ctrl Pts',(6.25793774774488,3.34911634724554,12.0932211063419));
#24116=CARTESIAN_POINT('Ctrl Pts',(8.24735113836601,0.301799589347462,12.2917372237535));
#24117=CARTESIAN_POINT('Ctrl Pts',(6.76514687416864,-3.02189949163811,12.4902533411652));
#24118=CARTESIAN_POINT('Ctrl Pts',(3.16869942579002,-3.57820050080496,12.6887694585768));
#24119=CARTESIAN_POINT('Ctrl Pts',(0.751566954770839,-0.857653555925328,
12.8872855759885));
#24120=CARTESIAN_POINT('Ctrl Pts',(1.72731339933552,2.64831620117018,13.0858016934002));
#24121=CARTESIAN_POINT('Ctrl Pts',(5.20236872621718,3.72900835754984,13.2843178108118));
#24122=CARTESIAN_POINT('Ctrl Pts',(7.99434336961907,1.39474559334568,13.4828339282235));
#24123=CARTESIAN_POINT('Ctrl Pts',(7.54640006010282,-2.21679865437008,13.6813500456351));
#24124=CARTESIAN_POINT('Ctrl Pts',(4.26875675973819,-3.79824086239538,13.8798661630468));
#24125=CARTESIAN_POINT('Ctrl Pts',(1.16301685561255,-1.9013263388412,14.0783822804584));
#24126=CARTESIAN_POINT('Ctrl Pts',(1.07335787448695,1.73678667876183,14.2768983978701));
#24127=CARTESIAN_POINT('Ctrl Pts',(4.08188780578152,3.78438349314049,14.4754145152818));
#24128=CARTESIAN_POINT('Ctrl Pts',(7.43345216672421,2.36631389110821,14.6739306326934));
#24129=CARTESIAN_POINT('Ctrl Pts',(8.05875206907788,-1.21878096033793,14.8724467501051));
#24130=CARTESIAN_POINT('Ctrl Pts',(5.38514975673243,-3.68773939197872,15.0709628675167));
#24131=CARTESIAN_POINT('Ctrl Pts',(1.86107937002522,-2.77953623668677,15.2694789849284));
#24132=CARTESIAN_POINT('Ctrl Pts',(0.713817534175901,0.674113331777405,
15.46799510234));
#24133=CARTESIAN_POINT('Ctrl Pts',(2.9940048152212,3.5104227339951,15.6665112197517));
#24134=CARTESIAN_POINT('Ctrl Pts',(6.61348907494099,3.13195377174095,15.8650273371633));
#24135=CARTESIAN_POINT('Ctrl Pts',(8.257615478175,-0.114698878595687,16.063543454575));
#24136=CARTESIAN_POINT('Ctrl Pts',(6.42072433944188,-3.25631247771842,16.2620595719866));
#24137=CARTESIAN_POINT('Ctrl Pts',(2.78500562221897,-3.41585705137789,16.4605756893983));
#24138=CARTESIAN_POINT('Ctrl Pts',(0.67998136903583,-0.447224713876356,
16.65909180681));
#24139=CARTESIAN_POINT('Ctrl Pts',(2.03339274915041,2.93096750947701,16.8576079242216));
#24140=CARTESIAN_POINT('Ctrl Pts',(5.60581136526813,3.62503544056518,17.0561240416333));
#24141=CARTESIAN_POINT('Ctrl Pts',(8.12568420335589,0.999364870669326,17.2546401590449));
#24142=CARTESIAN_POINT('Ctrl Pts',(7.28535965135699,-2.54150503784963,17.4531562764566));
#24143=CARTESIAN_POINT('Ctrl Pts',(3.85439094932391,-3.75491297725849,17.6516723938682));
#24144=CARTESIAN_POINT('Ctrl Pts',(0.974793970633971,-1.52964303811135,
17.8501885112799));
#24145=CARTESIAN_POINT('Ctrl Pts',(1.2836488526281,2.09644489844015,18.0487046286916));
#24146=CARTESIAN_POINT('Ctrl Pts',(4.49811216942012,3.80264847561477,18.2472207461032));
#24147=CARTESIAN_POINT('Ctrl Pts',(7.67443956106538,2.02645891285741,18.4457368635149));
#24148=CARTESIAN_POINT('Ctrl Pts',(7.90381082245328,-1.60552317494378,18.6442529809265));
#24149=CARTESIAN_POINT('Ctrl Pts',(4.9761721155001,-3.76719767944954,18.8427690983382));
#24150=CARTESIAN_POINT('Ctrl Pts',(1.57259927845708,-2.47894420875808,19.0412852157498));
#24151=CARTESIAN_POINT('Ctrl Pts',(0.810019572635768,1.07947921368855,19.2398013331615));
#24152=CARTESIAN_POINT('Ctrl Pts',(3.38678898688482,3.6493361063157,19.4383174505731));
#24153=CARTESIAN_POINT('Ctrl Pts',(6.94315110686829,2.87720041011993,19.6368335679848));
#24154=CARTESIAN_POINT('Ctrl Pts',(8.22225715251285,-0.529820690755693,
19.8353496853965));
#24155=CARTESIAN_POINT('Ctrl Pts',(6.05272613795891,-3.45164208273989,20.0338658028081));
#24156=CARTESIAN_POINT('Ctrl Pts',(2.42137329831411,-3.212515309774,20.2323819202198));
#24157=CARTESIAN_POINT('Ctrl Pts',(0.65372248686789,-0.0314281299545405,
20.4308980376314));
#24158=CARTESIAN_POINT('Ctrl Pts',(2.36855469553213,3.178440343651,20.6294141550431));
#24159=CARTESIAN_POINT('Ctrl Pts',(5.99545920128352,3.47755359131801,20.8279302724548));
#24160=CARTESIAN_POINT('Ctrl Pts',(8.21298586010566,0.591989447683331,21.0264463898664));
#24161=CARTESIAN_POINT('Ctrl Pts',(6.99036591797756,-2.83570744333498,21.2249625072781));
#24162=CARTESIAN_POINT('Ctrl Pts',(3.44725150283742,-3.6665172604341,21.4234786246897));
#24163=CARTESIAN_POINT('Ctrl Pts',(0.828359319011244,-1.13960058009792,
21.6219947421014));
#24164=CARTESIAN_POINT('Ctrl Pts',(1.53202116508044,2.43094114262164,21.820510859513));
#24165=CARTESIAN_POINT('Ctrl Pts',(4.91383661347899,3.77527223251319,22.0190269769247));
#24166=CARTESIAN_POINT('Ctrl Pts',(7.87680396956558,1.66228269728872,22.2175430943363));
#24167=CARTESIAN_POINT('Ctrl Pts',(7.7074930081086,-1.97299730385434,22.416059211748));
#24168=CARTESIAN_POINT('Ctrl Pts',(4.56095756308617,-3.80143701374933,22.6145753291597));
#24169=CARTESIAN_POINT('Ctrl Pts',(1.31873095853907,-2.14860623751896,22.8130914465713));
#24170=CARTESIAN_POINT('Ctrl Pts',(0.949990286798536,1.47190262315773,23.011607563983));
#24171=CARTESIAN_POINT('Ctrl Pts',(3.7924065803434,3.74442240079083,23.2101236813946));
#24172=CARTESIAN_POINT('Ctrl Pts',(7.24297719250067,2.58796472414074,23.4086397988063));
#24173=CARTESIAN_POINT('Ctrl Pts',(8.14168123233833,-0.938680920498277,
23.6071559162179));
#24174=CARTESIAN_POINT('Ctrl Pts',(5.66560616055497,-3.60535681683013,23.8056720336296));
#24175=CARTESIAN_POINT('Ctrl Pts',(2.08209581503262,-2.97097481614092,24.0041881510412));
#24176=CARTESIAN_POINT('Ctrl Pts',(0.673241827254791,0.385434817028999,
24.2027042684529));
#24177=CARTESIAN_POINT('Ctrl Pts',(2.72851506381635,3.38643791990783,24.4012203858645));
#24178=CARTESIAN_POINT('Ctrl Pts',(6.36713580394013,3.29091791303403,24.5997365032762));
#24179=CARTESIAN_POINT('Ctrl Pts',(8.25465969525897,0.17151120336101,24.7982954766299));
#24180=CARTESIAN_POINT('Ctrl Pts',(7.19525837483205,-1.99900958588141,24.9306824108463));
#24181=CARTESIAN_POINT('Ctrl Pts',(6.32311239899223,-2.62025147071356,24.9968973059255));
#24182=CARTESIAN_POINT('Ctrl Pts',(5.99341579333084,3.0962819108244,-0.27495920519366));
#24183=CARTESIAN_POINT('Ctrl Pts',(7.02329163031133,2.58506739568259,-0.208787166056442));
#24184=CARTESIAN_POINT('Ctrl Pts',(8.51497056474962,0.462964065771816,-0.0764430877820045));
#24185=CARTESIAN_POINT('Ctrl Pts',(7.04304871618797,-3.16665160770128,0.122073029629653));
#24186=CARTESIAN_POINT('Ctrl Pts',(3.19892054011338,-3.88657631350085,0.320589147041309));
#24187=CARTESIAN_POINT('Ctrl Pts',(0.508208668906595,-1.05209144762919,
0.519105264452963));
#24188=CARTESIAN_POINT('Ctrl Pts',(1.43231541168923,2.74837799923302,0.717621381864618));
#24189=CARTESIAN_POINT('Ctrl Pts',(5.12636543519397,4.03063520713254,0.916137499276276));
#24190=CARTESIAN_POINT('Ctrl Pts',(8.20668654383497,1.62239064105283,1.11465361668793));
#24191=CARTESIAN_POINT('Ctrl Pts',(7.85276047702285,-2.27196140132349,1.31316973409959));
#24192=CARTESIAN_POINT('Ctrl Pts',(4.38850729527858,-4.08551042322263,1.51168585151124));
#24193=CARTESIAN_POINT('Ctrl Pts',(0.986527733847538,-2.15772261402933,
1.7102019689229));
#24194=CARTESIAN_POINT('Ctrl Pts',(0.7622359790706,1.74611650720567,1.90871808633455));
#24195=CARTESIAN_POINT('Ctrl Pts',(3.92106229159746,4.0508692911502,2.10723420374621));
#24196=CARTESIAN_POINT('Ctrl Pts',(7.57019895508782,2.64592661456843,2.30575032115786));
#24197=CARTESIAN_POINT('Ctrl Pts',(8.36784367179503,-1.18211240346562,2.50426643856952));
#24198=CARTESIAN_POINT('Ctrl Pts',(5.58352459826198,-3.92759167890361,2.70278255598118));
#24199=CARTESIAN_POINT('Ctrl Pts',(1.7670702556363,-3.07625912870098,2.90129867339283));
#24200=CARTESIAN_POINT('Ctrl Pts',(0.413515851644582,0.592254017343965,
3.09981479080449));
#24201=CARTESIAN_POINT('Ctrl Pts',(2.76242132641212,3.7183916776686,3.29833090821614));
#24202=CARTESIAN_POINT('Ctrl Pts',(6.66270343294158,3.43929724324088,3.4968470256278));
#24203=CARTESIAN_POINT('Ctrl Pts',(8.54255816261418,0.0105596738669375,
3.69536314303945));
#24204=CARTESIAN_POINT('Ctrl Pts',(6.6804502327146,-3.42784816997514,3.89387926045112));
#24205=CARTESIAN_POINT('Ctrl Pts',(2.78166270604797,-3.72709790290783,4.09239537786277));
#24206=CARTESIAN_POINT('Ctrl Pts',(0.416631015022661,-0.613142253174304,
4.29091149527442));
#24207=CARTESIAN_POINT('Ctrl Pts',(1.75120620592284,3.06231739833558,4.48942761268608));
#24208=CARTESIAN_POINT('Ctrl Pts',(5.56320969933569,3.93336503336498,4.68794373009773));
#24209=CARTESIAN_POINT('Ctrl Pts',(8.36168121106336,1.20231178852842,4.88645984750939));
#24210=CARTESIAN_POINT('Ctrl Pts',(7.58383376163584,-2.62979572036334,5.08497596492104));
#24211=CARTESIAN_POINT('Ctrl Pts',(3.94200524984668,-4.05358633333867,5.2834920823327));
#24212=CARTESIAN_POINT('Ctrl Pts',(0.771312951433223,-1.76517968922739,
5.48200819974436));
#24213=CARTESIAN_POINT('Ctrl Pts',(0.97541656054666,2.13974493679014,5.68052431715601));
#24214=CARTESIAN_POINT('Ctrl Pts',(4.36740187430494,4.08513185206935,5.87904043456767));
#24215=CARTESIAN_POINT('Ctrl Pts',(7.84095326483218,2.28943272461384,6.07755655197932));
#24216=CARTESIAN_POINT('Ctrl Pts',(8.21505844260491,-1.60288534238506,6.27607266939098));
#24217=CARTESIAN_POINT('Ctrl Pts',(5.14711900207072,-4.02731150295548,6.47458878680263));
#24218=CARTESIAN_POINT('Ctrl Pts',(1.44669552446588,-2.76360239669899,6.6731049042143));
#24219=CARTESIAN_POINT('Ctrl Pts',(0.502565441067234,1.03096121515846,6.87162102162594));
#24220=CARTESIAN_POINT('Ctrl Pts',(3.17934512299035,3.88139015713774,7.07013713903761));
#24221=CARTESIAN_POINT('Ctrl Pts',(7.0256906552799,3.17731582507866,7.26865325644925));
#24222=CARTESIAN_POINT('Ctrl Pts',(8.51919196471455,-0.436483900631263,
7.46716937386092));
#24223=CARTESIAN_POINT('Ctrl Pts',(6.2921289615216,-3.65055997294754,7.66568549127257));
#24224=CARTESIAN_POINT('Ctrl Pts',(2.38400358079477,-3.52152266305215,7.86420160868423));
#24225=CARTESIAN_POINT('Ctrl Pts',(0.373802705776339,-0.16754188479758,
8.06271772609589));
#24226=CARTESIAN_POINT('Ctrl Pts',(2.10243005973299,3.33987056457006,8.26123384350753));
#24227=CARTESIAN_POINT('Ctrl Pts',(5.98684159389007,3.78869308197905,8.4597499609192));
#24228=CARTESIAN_POINT('Ctrl Pts',(8.4697671146088,0.767902543495819,8.65826607833084));
#24229=CARTESIAN_POINT('Ctrl Pts',(7.27739066026635,-2.95611853726567,8.85678219574251));
#24230=CARTESIAN_POINT('Ctrl Pts',(3.50166790634439,-3.97298249293629,9.05529831315416));
#24231=CARTESIAN_POINT('Ctrl Pts',(0.600333929022254,-1.35146465571633,
9.25381443056581));
#24232=CARTESIAN_POINT('Ctrl Pts',(1.23037519550738,2.50769880562501,9.45233054797748));
#24233=CARTESIAN_POINT('Ctrl Pts',(4.81481189860833,4.07035940226423,9.65084666538912));
#24234=CARTESIAN_POINT('Ctrl Pts',(8.07108508884113,1.90546228475562,9.84936278280079));
#24235=CARTESIAN_POINT('Ctrl Pts',(8.01716171947454,-2.00442094739626,10.0478789002124));
#24236=CARTESIAN_POINT('Ctrl Pts',(4.70242378644322,-4.07869360405195,10.2463950176241));
#24237=CARTESIAN_POINT('Ctrl Pts',(1.16244523581599,-2.41777624309588,10.4449111350357));
#24238=CARTESIAN_POINT('Ctrl Pts',(0.639071086725107,1.45729461030662,10.6434272524474));
#24239=CARTESIAN_POINT('Ctrl Pts',(3.61159742927608,3.99780278027315,10.841943369859));
#24240=CARTESIAN_POINT('Ctrl Pts',(7.35784118240728,2.87719921033794,11.0404594872707));
#24241=CARTESIAN_POINT('Ctrl Pts',(8.44706357811351,-0.878288666292467,
11.2389756046823));
#24242=CARTESIAN_POINT('Ctrl Pts',(5.88177546561389,-3.82945648915419,11.437491722094));
#24243=CARTESIAN_POINT('Ctrl Pts',(2.01121890138154,-3.27368090323489,11.6360078395057));
#24244=CARTESIAN_POINT('Ctrl Pts',(0.379975961147697,0.280069381853164,
11.8345239569173));
#24245=CARTESIAN_POINT('Ctrl Pts',(2.4819079000476,3.57733745452462,12.033040074329));
#24246=CARTESIAN_POINT('Ctrl Pts',(6.39210543142176,3.59854793451629,12.2315561917406));
#24247=CARTESIAN_POINT('Ctrl Pts',(8.52968403588164,0.324276667717884,12.4300723091523));
#24248=CARTESIAN_POINT('Ctrl Pts',(6.93708988851933,-3.24696100298028,12.6285884265639));
#24249=CARTESIAN_POINT('Ctrl Pts',(3.07279041513639,-3.84469355089646,12.8271045439756));
#24250=CARTESIAN_POINT('Ctrl Pts',(0.475637566686629,-0.921528878727684,
13.0256206613872));
#24251=CARTESIAN_POINT('Ctrl Pts',(1.52405451869475,2.84555441124189,13.2241367787989));
#24252=CARTESIAN_POINT('Ctrl Pts',(5.25792096951678,4.00673309958052,13.4226528962106));
#24253=CARTESIAN_POINT('Ctrl Pts',(8.257833049161,1.4986218314684,13.6211690136222));
#24254=CARTESIAN_POINT('Ctrl Pts',(7.77652833946771,-2.38189880309254,13.8196851310339));
#24255=CARTESIAN_POINT('Ctrl Pts',(4.25477653818775,-4.08112182230083,14.0182012484455));
#24256=CARTESIAN_POINT('Ctrl Pts',(0.917730954110628,-2.04293110781465,
14.2167173658572));
#24257=CARTESIAN_POINT('Ctrl Pts',(0.821394455796449,1.86613705453794,14.4152334832688));
#24258=CARTESIAN_POINT('Ctrl Pts',(4.05399017588675,4.06623240003544,14.6137496006805));
#24259=CARTESIAN_POINT('Ctrl Pts',(7.65516844441363,2.54254946152231,14.8122657180922));
#24260=CARTESIAN_POINT('Ctrl Pts',(8.32703870473431,-1.30955190943392,15.0107818355038));
#24261=CARTESIAN_POINT('Ctrl Pts',(5.45431495277465,-3.96239055204922,15.2092979529155));
#24262=CARTESIAN_POINT('Ctrl Pts',(1.66778295557931,-2.98654729975826,15.4078140703271));
#24263=CARTESIAN_POINT('Ctrl Pts',(0.435076688703739,0.724319159497842,
15.6063301877388));
#24264=CARTESIAN_POINT('Ctrl Pts',(2.88508510279309,3.77186791049719,15.8048463051504));
#24265=CARTESIAN_POINT('Ctrl Pts',(6.77413709632598,3.36521177759866,16.0033624225621));
#24266=CARTESIAN_POINT('Ctrl Pts',(8.54071283123811,-0.123241288109086,
16.2018785399737));
#24267=CARTESIAN_POINT('Ctrl Pts',(6.56701585333057,-3.49883232646441,16.4003946573854));
#24268=CARTESIAN_POINT('Ctrl Pts',(2.66052031127365,-3.67025927509159,16.598910774797));
#24269=CARTESIAN_POINT('Ctrl Pts',(0.398720513058523,-0.480532595324168,
16.7974268922087));
#24270=CARTESIAN_POINT('Ctrl Pts',(1.85292968989636,3.14925669454191,16.9959430096203));
#24271=CARTESIAN_POINT('Ctrl Pts',(5.69141073963082,3.89501660876095,17.194459127032));
#24272=CARTESIAN_POINT('Ctrl Pts',(8.39895573256671,1.07379440374864,17.3929752444437));
#24273=CARTESIAN_POINT('Ctrl Pts',(7.49604646714037,-2.73078829048094,17.5914913618553));
#24274=CARTESIAN_POINT('Ctrl Pts',(3.80955007347359,-4.03456701338995,17.790007479267));
#24275=CARTESIAN_POINT('Ctrl Pts',(0.715489824289806,-1.64356601103751,
17.9885235966786));
#24276=CARTESIAN_POINT('Ctrl Pts',(1.04734724052415,2.25258148028018,18.1870397140903));
#24277=CARTESIAN_POINT('Ctrl Pts',(4.50121361298798,4.08585770060491,18.3855558315019));
#24278=CARTESIAN_POINT('Ctrl Pts',(7.91410381728119,2.1773831599618,18.5840719489136));
#24279=CARTESIAN_POINT('Ctrl Pts',(8.16055792437237,-1.72509746033864,18.7825880663253));
#24280=CARTESIAN_POINT('Ctrl Pts',(5.0148779510323,-4.04776664132528,18.9811041837369));
#24281=CARTESIAN_POINT('Ctrl Pts',(1.35781777968586,-2.66356812881232,19.1796203011486));
#24282=CARTESIAN_POINT('Ctrl Pts',(0.538443550556935,1.1598754095142,19.3781364185603));
#24283=CARTESIAN_POINT('Ctrl Pts',(3.30712259659747,3.92112711119714,19.5766525359719));
#24284=CARTESIAN_POINT('Ctrl Pts',(7.12835131317638,3.09148519177063,19.7751686533836));
#24285=CARTESIAN_POINT('Ctrl Pts',(8.50272112937199,-0.569280059186615,
19.9736847707952));
#24286=CARTESIAN_POINT('Ctrl Pts',(6.17161031033075,-3.70870946234774,20.1722008882069));
#24287=CARTESIAN_POINT('Ctrl Pts',(2.26980580259814,-3.45177328404759,20.3707170056185));
#24288=CARTESIAN_POINT('Ctrl Pts',(0.370505952442893,-0.0337687976193256,
20.5692331230302));
#24289=CARTESIAN_POINT('Ctrl Pts',(2.21305343742525,3.41516052227788,20.7677492404418));
#24290=CARTESIAN_POINT('Ctrl Pts',(6.11007831343283,3.73655077808788,20.9662653578534));
#24291=CARTESIAN_POINT('Ctrl Pts',(8.49275934044528,0.636078948397367,21.1647814752652));
#24292=CARTESIAN_POINT('Ctrl Pts',(7.17908253400595,-3.04690196012391,21.3632975926768));
#24293=CARTESIAN_POINT('Ctrl Pts',(3.37208816940477,-3.93958786330456,21.5618137100885));
#24294=CARTESIAN_POINT('Ctrl Pts',(0.558149183206385,-1.22447442503984,
21.7603298275001));
#24295=CARTESIAN_POINT('Ctrl Pts',(1.31421753683424,2.61198994621562,21.9588459449118));
#24296=CARTESIAN_POINT('Ctrl Pts',(4.94789989808116,4.05644256154919,22.1573620623234));
#24297=CARTESIAN_POINT('Ctrl Pts',(8.13153968654471,1.78608425229248,22.3558781797351));
#24298=CARTESIAN_POINT('Ctrl Pts',(7.94961898046267,-2.11993989949929,22.5543942971467));
#24299=CARTESIAN_POINT('Ctrl Pts',(4.56873953270021,-4.0845560128934,22.7529104145584));
#24300=CARTESIAN_POINT('Ctrl Pts',(1.08504215066615,-2.30862763082918,22.95142653197));
#24301=CARTESIAN_POINT('Ctrl Pts',(0.688838840573486,1.58152527269752,23.1499426493817));
#24302=CARTESIAN_POINT('Ctrl Pts',(3.74294930484078,4.02329513198439,23.3484587667933));
#24303=CARTESIAN_POINT('Ctrl Pts',(7.45050749686758,2.78070814718547,23.546974884205));
#24304=CARTESIAN_POINT('Ctrl Pts',(8.41614416964521,-1.00859090500303,23.7454910016166));
#24305=CARTESIAN_POINT('Ctrl Pts',(5.75565886205016,-3.87387238340306,23.9440071190283));
#24306=CARTESIAN_POINT('Ctrl Pts',(1.90526000600476,-3.19224361880315,24.14252323644));
#24307=CARTESIAN_POINT('Ctrl Pts',(0.391479031532891,0.414140782493564,
24.3410393538516));
#24308=CARTESIAN_POINT('Ctrl Pts',(2.59982251484541,3.6386490998064,24.5395554712633));
#24309=CARTESIAN_POINT('Ctrl Pts',(6.50943621328541,3.53601506509354,24.7380715886749));
#24310=CARTESIAN_POINT('Ctrl Pts',(8.53753691096405,0.184284815040506,24.9366305620286));
#24311=CARTESIAN_POINT('Ctrl Pts',(7.39923473266516,-2.14788949397592,25.069017496245));
#24312=CARTESIAN_POINT('Ctrl Pts',(6.46213408444902,-2.81539950847165,25.1352323913243));
#24313=CARTESIAN_POINT('Ctrl Pts',(6.0999485000484,3.31089917470656,-0.136624119794918));
#24314=CARTESIAN_POINT('Ctrl Pts',(7.2012096761669,2.76425007587486,-0.0704520806576993));
#24315=CARTESIAN_POINT('Ctrl Pts',(8.79628360522135,0.495054193199949,0.061891997616738));
#24316=CARTESIAN_POINT('Ctrl Pts',(7.22233621477278,-3.38614651265062,0.260408115028396));
#24317=CARTESIAN_POINT('Ctrl Pts',(3.11175417728552,-4.15597244676529,0.458924232440051));
#24318=CARTESIAN_POINT('Ctrl Pts',(0.234536930817258,-1.12501665093665,
0.657440349851707));
#24319=CARTESIAN_POINT('Ctrl Pts',(1.22269767978634,2.93888047390986,0.855956467263361));
#24320=CARTESIAN_POINT('Ctrl Pts',(5.17279897107673,4.31001671203934,1.05447258467502));
#24321=CARTESIAN_POINT('Ctrl Pts',(8.46663102841521,1.73484585358162,1.25298870208667));
#24322=CARTESIAN_POINT('Ctrl Pts',(8.08817274965877,-2.42944129289705,1.45150481949833));
#24323=CARTESIAN_POINT('Ctrl Pts',(4.38379655564558,-4.36869557685114,1.65002093690999));
#24324=CARTESIAN_POINT('Ctrl Pts',(0.746010447431816,-2.30728410002347,
1.84853705432164));
#24325=CARTESIAN_POINT('Ctrl Pts',(0.506172019545635,1.86714771753756,2.04705317173329));
#24326=CARTESIAN_POINT('Ctrl Pts',(3.88395083052018,4.33165331167866,2.24556928914495));
#24327=CARTESIAN_POINT('Ctrl Pts',(7.78602561424836,2.82932772170484,2.4440854065566));
#24328=CARTESIAN_POINT('Ctrl Pts',(8.63895868375428,-1.26404994563383,2.64260152396827));
#24329=CARTESIAN_POINT('Ctrl Pts',(5.66164589758561,-4.19983077212884,2.84111764137992));
#24330=CARTESIAN_POINT('Ctrl Pts',(1.58065589175627,-3.28948852324876,3.03963375879158));
#24331=CARTESIAN_POINT('Ctrl Pts',(0.133280527313607,0.633305814430374,
3.23814987620323));
#24332=CARTESIAN_POINT('Ctrl Pts',(2.6449992344131,3.97613017528841,3.43666599361489));
#24333=CARTESIAN_POINT('Ctrl Pts',(6.81562748453676,3.67769044685756,3.63518211102655));
#24334=CARTESIAN_POINT('Ctrl Pts',(8.82578342391765,0.0112916124882134,
3.8336982284382));
#24335=CARTESIAN_POINT('Ctrl Pts',(6.83460439504253,-3.66544778668689,4.03221434584986));
#24336=CARTESIAN_POINT('Ctrl Pts',(2.66557432085276,-3.98543986826524,4.23073046326151));
#24337=CARTESIAN_POINT('Ctrl Pts',(0.13661161671523,-0.655641908094887,
4.42924658067317));
#24338=CARTESIAN_POINT('Ctrl Pts',(1.56369223320815,3.27458042867263,4.62776269808482));
#24339=CARTESIAN_POINT('Ctrl Pts',(5.63992288139177,4.20600430382654,4.82627881549648));
#24340=CARTESIAN_POINT('Ctrl Pts',(8.63236907507575,1.28564944117731,5.02479493290813));
#24341=CARTESIAN_POINT('Ctrl Pts',(7.80060551073305,-2.81207872246989,5.22331105031979));
#24342=CARTESIAN_POINT('Ctrl Pts',(3.90634543966123,-4.33455868431544,5.42182716773146));
#24343=CARTESIAN_POINT('Ctrl Pts',(0.515878157801087,-1.88753225468275,
5.62034328514309));
#24344=CARTESIAN_POINT('Ctrl Pts',(0.734129108596551,2.28806030889307,5.81885940255477));
#24345=CARTESIAN_POINT('Ctrl Pts',(4.36122822275595,4.36829076522382,6.0173755199664));
#24346=CARTESIAN_POINT('Ctrl Pts',(8.07554712633902,2.44812363240269,6.21589163737808));
#24347=CARTESIAN_POINT('Ctrl Pts',(8.47558322124728,-1.71398855469165,6.41440775478972));
#24348=CARTESIAN_POINT('Ctrl Pts',(5.19499106127511,-4.3064626269354,6.61292387220138));
#24349=CARTESIAN_POINT('Ctrl Pts',(1.2380745430358,-2.9551601430283,6.81143998961304));
#24350=CARTESIAN_POINT('Ctrl Pts',(0.228502545404632,1.10242178675316,7.00995610702469));
#24351=CARTESIAN_POINT('Ctrl Pts',(3.09082189971391,4.15042681451437,7.20847222443635));
#24352=CARTESIAN_POINT('Ctrl Pts',(7.20377498837598,3.39754991503151,7.406988341848));
#24353=CARTESIAN_POINT('Ctrl Pts',(8.80079760945692,-0.466738568384383,
7.60550445925966));
#24354=CARTESIAN_POINT('Ctrl Pts',(6.41936682516261,-3.90359674918315,7.80402057667131));
#24355=CARTESIAN_POINT('Ctrl Pts',(2.24035164813274,-3.7656152813635,8.00253669408298));
#24356=CARTESIAN_POINT('Ctrl Pts',(0.0908146841936848,-0.179154968469096,
8.20105281149462));
#24357=CARTESIAN_POINT('Ctrl Pts',(1.93926099639212,3.57137205666049,8.39956892890629));
#24358=CARTESIAN_POINT('Ctrl Pts',(6.09291861319388,4.05130448700034,8.59808504631793));
#24359=CARTESIAN_POINT('Ctrl Pts',(8.7479469000777,0.821129332128062,8.7966011637296));
#24360=CARTESIAN_POINT('Ctrl Pts',(7.47292145590854,-3.16102044557099,8.99511728114126));
#24361=CARTESIAN_POINT('Ctrl Pts',(3.43548632890085,-4.24836782820074,9.19363339855291));
#24362=CARTESIAN_POINT('Ctrl Pts',(0.333047808208697,-1.44514076628925,
9.39214951596456));
#24363=CARTESIAN_POINT('Ctrl Pts',(1.00676007644372,2.68151871989772,9.59066563337622));
#24364=CARTESIAN_POINT('Ctrl Pts',(4.83965025372247,4.352494370297,9.78918175078787));
#24365=CARTESIAN_POINT('Ctrl Pts',(8.32163042499515,2.03753846960017,9.98769786819953));
#24366=CARTESIAN_POINT('Ctrl Pts',(8.26396938369623,-2.14335640346512,10.1862139856111));
#24367=CARTESIAN_POINT('Ctrl Pts',(4.71947201461794,-4.36140625319899,10.3847301030228));
#24368=CARTESIAN_POINT('Ctrl Pts',(0.934121584873003,-2.58536321899705,
10.5832462204345));
#24369=CARTESIAN_POINT('Ctrl Pts',(0.37447001302165,1.5583062723393,10.7817623378461));
#24370=CARTESIAN_POINT('Ctrl Pts',(3.55303556286365,4.27490852159572,10.9802784552578));
#24371=CARTESIAN_POINT('Ctrl Pts',(7.55894836658157,3.07663086415728,11.1787945726694));
#24372=CARTESIAN_POINT('Ctrl Pts',(8.72366967907197,-0.939166814951776,
11.3773106900811));
#24373=CARTESIAN_POINT('Ctrl Pts',(5.98056987770475,-4.09489338977514,11.5758268074927));
#24374=CARTESIAN_POINT('Ctrl Pts',(1.84172758128094,-3.50059449137405,11.7743429249044));
#24375=CARTESIAN_POINT('Ctrl Pts',(0.0974158357370281,0.299482253859507,
11.9728590423161));
#24376=CARTESIAN_POINT('Ctrl Pts',(2.34504215731444,3.82529884776504,12.1713751597277));
#24377=CARTESIAN_POINT('Ctrl Pts',(6.52627311509865,3.84797952178704,12.3698912771394));
#24378=CARTESIAN_POINT('Ctrl Pts',(8.81201693339725,0.346753746088307,12.568407394551));
#24379=CARTESIAN_POINT('Ctrl Pts',(7.10903290287004,-3.47202251432246,12.7669235119627));
#24380=CARTESIAN_POINT('Ctrl Pts',(2.97688140448274,-4.11118660098796,12.9654396293744));
#24381=CARTESIAN_POINT('Ctrl Pts',(0.199708178602426,-0.985404201530036,
13.163955746786));
#24382=CARTESIAN_POINT('Ctrl Pts',(1.32079563805398,3.0427926213136,13.3624718641977));
#24383=CARTESIAN_POINT('Ctrl Pts',(5.3134732128164,4.28445784161121,13.5609879816093));
#24384=CARTESIAN_POINT('Ctrl Pts',(8.52132272870291,1.60249806959112,13.759504099021));
#24385=CARTESIAN_POINT('Ctrl Pts',(8.00665661883263,-2.546998951815,13.9580202164326));
#24386=CARTESIAN_POINT('Ctrl Pts',(4.24079631663729,-4.36400278220629,14.1565363338443));
#24387=CARTESIAN_POINT('Ctrl Pts',(0.672445052608722,-2.18453587678811,
14.3550524512559));
#24388=CARTESIAN_POINT('Ctrl Pts',(0.569431037105937,1.99548743031406,14.5535685686676));
#24389=CARTESIAN_POINT('Ctrl Pts',(4.02609254599198,4.3480813069304,14.7520846860792));
#24390=CARTESIAN_POINT('Ctrl Pts',(7.87688472210303,2.7187850319364,14.9506008034909));
#24391=CARTESIAN_POINT('Ctrl Pts',(8.59532534039074,-1.40032285852991,15.1491169209026));
#24392=CARTESIAN_POINT('Ctrl Pts',(5.52348014881688,-4.2370417121197,15.3476330383142));
#24393=CARTESIAN_POINT('Ctrl Pts',(1.47448654113341,-3.19355836282975,15.5461491557259));
#24394=CARTESIAN_POINT('Ctrl Pts',(0.156335843231577,0.774524987218279,
15.7446652731375));
#24395=CARTESIAN_POINT('Ctrl Pts',(2.77616539036498,4.03331308699926,15.9431813905492));
#24396=CARTESIAN_POINT('Ctrl Pts',(6.93478511771097,3.59846978345639,16.1416975079608));
#24397=CARTESIAN_POINT('Ctrl Pts',(8.82381018430121,-0.131783697622486,
16.3402136253725));
#24398=CARTESIAN_POINT('Ctrl Pts',(6.71330736721926,-3.74135217521042,16.5387297427841));
#24399=CARTESIAN_POINT('Ctrl Pts',(2.53603500032833,-3.92466149880528,16.7372458601958));
#24400=CARTESIAN_POINT('Ctrl Pts',(0.117459657081213,-0.513840476771981,
16.9357619776075));
#24401=CARTESIAN_POINT('Ctrl Pts',(1.6724666306423,3.3675458796068,17.1342780950191));
#24402=CARTESIAN_POINT('Ctrl Pts',(5.77701011399349,4.16499777695671,17.3327942124308));
#24403=CARTESIAN_POINT('Ctrl Pts',(8.67222726177754,1.14822393682795,17.5313103298424));
#24404=CARTESIAN_POINT('Ctrl Pts',(7.70673328292373,-2.92007154311226,17.7298264472541));
#24405=CARTESIAN_POINT('Ctrl Pts',(3.76470919762329,-4.31422104952143,17.9283425646657));
#24406=CARTESIAN_POINT('Ctrl Pts',(0.456185677945633,-1.75748898396369,
18.1268586820774));
#24407=CARTESIAN_POINT('Ctrl Pts',(0.811045628420214,2.40871806212022,18.3253747994891));
#24408=CARTESIAN_POINT('Ctrl Pts',(4.50431505655582,4.36906692559506,18.5238909169007));
#24409=CARTESIAN_POINT('Ctrl Pts',(8.153768073497,2.32830740706619,18.7224070343124));
#24410=CARTESIAN_POINT('Ctrl Pts',(8.41730502629147,-1.84467174573349,18.920923151724));
#24411=CARTESIAN_POINT('Ctrl Pts',(5.05358378656449,-4.328335603201,19.1194392691357));
#24412=CARTESIAN_POINT('Ctrl Pts',(1.14303628091464,-2.84819204886657,19.3179553865473));
#24413=CARTESIAN_POINT('Ctrl Pts',(0.266867528478102,1.24027160533984,19.516471503959));
#24414=CARTESIAN_POINT('Ctrl Pts',(3.22745620631011,4.19291811607857,19.7149876213706));
#24415=CARTESIAN_POINT('Ctrl Pts',(7.31355151948446,3.30576997342133,19.9135037387823));
#24416=CARTESIAN_POINT('Ctrl Pts',(8.78318510623113,-0.60873942761753,20.112019856194));
#24417=CARTESIAN_POINT('Ctrl Pts',(6.29049448270258,-3.96577684195559,20.3105359736056));
#24418=CARTESIAN_POINT('Ctrl Pts',(2.11823830688215,-3.69103125832118,20.5090520910173));
#24419=CARTESIAN_POINT('Ctrl Pts',(0.0872894180178925,-0.0361094652841183,
20.7075682084289));
#24420=CARTESIAN_POINT('Ctrl Pts',(2.05755217931839,3.65188070090475,20.9060843258406));
#24421=CARTESIAN_POINT('Ctrl Pts',(6.2246974255821,3.99554796485774,21.1046004432522));
#24422=CARTESIAN_POINT('Ctrl Pts',(8.77253282078492,0.680168449111409,21.3031165606639));
#24423=CARTESIAN_POINT('Ctrl Pts',(7.36779915003431,-3.25809647691284,21.5016326780756));
#24424=CARTESIAN_POINT('Ctrl Pts',(3.29692483597213,-4.21265846617502,21.7001487954872));
#24425=CARTESIAN_POINT('Ctrl Pts',(0.287939047401517,-1.30934826998177,
21.8986649128989));
#24426=CARTESIAN_POINT('Ctrl Pts',(1.09641390858805,2.79303874980958,22.0971810303105));
#24427=CARTESIAN_POINT('Ctrl Pts',(4.98196318268333,4.33761289058522,22.2956971477222));
#24428=CARTESIAN_POINT('Ctrl Pts',(8.38627540352384,1.90988580729624,22.4942132651338));
#24429=CARTESIAN_POINT('Ctrl Pts',(8.19174495281671,-2.26688249514424,22.6927293825455));
#24430=CARTESIAN_POINT('Ctrl Pts',(4.57652150231426,-4.36767501203749,22.8912454999571));
#24431=CARTESIAN_POINT('Ctrl Pts',(0.851353342793238,-2.46864902413938,
23.0897616173688));
#24432=CARTESIAN_POINT('Ctrl Pts',(0.42768739434844,1.69114792223732,23.2882777347804));
#24433=CARTESIAN_POINT('Ctrl Pts',(3.69349202933814,4.30216786317793,23.4867938521921));
#24434=CARTESIAN_POINT('Ctrl Pts',(7.65803780123451,2.9734515702302,23.6853099696038));
#24435=CARTESIAN_POINT('Ctrl Pts',(8.6906071069521,-1.07850088950778,23.8838260870154));
#24436=CARTESIAN_POINT('Ctrl Pts',(5.84571156354535,-4.14238794997599,24.0823422044271));
#24437=CARTESIAN_POINT('Ctrl Pts',(1.7284241969769,-3.41351242146536,24.2808583218387));
#24438=CARTESIAN_POINT('Ctrl Pts',(0.109716235810993,0.442846747958131,
24.4793744392504));
#24439=CARTESIAN_POINT('Ctrl Pts',(2.47112996587446,3.89086027970496,24.677890556662));
#24440=CARTESIAN_POINT('Ctrl Pts',(6.6517366226307,3.78111221715306,24.8764066740737));
#24441=CARTESIAN_POINT('Ctrl Pts',(8.82041412666913,0.197058426719993,25.0749656474274));
#24442=CARTESIAN_POINT('Ctrl Pts',(7.60321109049825,-2.29676940207044,25.2073525816438));
#24443=CARTESIAN_POINT('Ctrl Pts',(6.60115576990582,-3.01054754622974,25.273567476723));
#24444=CARTESIAN_POINT('Ctrl Pts',(6.20648120676596,3.5255164385887,0.00171096560382468));
#24445=CARTESIAN_POINT('Ctrl Pts',(7.37912772202248,2.94343275606714,0.0678830047410433));
#24446=CARTESIAN_POINT('Ctrl Pts',(9.07759664569311,0.527144320628084,0.200227083015481));
#24447=CARTESIAN_POINT('Ctrl Pts',(7.40162371335757,-3.60564141759996,0.398743200427137));
#24448=CARTESIAN_POINT('Ctrl Pts',(3.02458781445768,-4.42536858002973,0.597259317838794));
#24449=CARTESIAN_POINT('Ctrl Pts',(-0.0391348072720899,-1.19794185424409,
0.795775435250448));
#24450=CARTESIAN_POINT('Ctrl Pts',(1.01307994788347,3.12938294858669,0.994291552662105));
#24451=CARTESIAN_POINT('Ctrl Pts',(5.21923250695947,4.58939821694615,1.19280767007376));
#24452=CARTESIAN_POINT('Ctrl Pts',(8.72657551299543,1.84730106611042,1.39132378748542));
#24453=CARTESIAN_POINT('Ctrl Pts',(8.32358502229467,-2.58692118447061,1.58983990489707));
#24454=CARTESIAN_POINT('Ctrl Pts',(4.37908581601258,-4.65188073047965,1.78835602230873));
#24455=CARTESIAN_POINT('Ctrl Pts',(0.505493161016087,-2.45684558601761,
1.98687213972038));
#24456=CARTESIAN_POINT('Ctrl Pts',(0.250108060020668,1.98817892786946,2.18538825713204));
#24457=CARTESIAN_POINT('Ctrl Pts',(3.8468393694429,4.61243733220712,2.38390437454369));
#24458=CARTESIAN_POINT('Ctrl Pts',(8.0018522734089,3.01272882884126,2.58242049195535));
#24459=CARTESIAN_POINT('Ctrl Pts',(8.91007369571349,-1.34598748780205,2.78093660936701));
#24460=CARTESIAN_POINT('Ctrl Pts',(5.73976719690925,-4.47206986535408,2.97945272677866));
#24461=CARTESIAN_POINT('Ctrl Pts',(1.39424152787623,-3.50271791779653,3.17796884419032));
#24462=CARTESIAN_POINT('Ctrl Pts',(-0.146954797017362,0.674357611516781,
3.37648496160198));
#24463=CARTESIAN_POINT('Ctrl Pts',(2.5275771424141,4.23386867290823,3.57500107901363));
#24464=CARTESIAN_POINT('Ctrl Pts',(6.96855153613195,3.91608365047424,3.77351719642529));
#24465=CARTESIAN_POINT('Ctrl Pts',(9.10900868522111,0.0120235511094912,
3.97203331383693));
#24466=CARTESIAN_POINT('Ctrl Pts',(6.98875855737045,-3.90304740339865,4.17054943124861));
#24467=CARTESIAN_POINT('Ctrl Pts',(2.54948593565754,-4.24378183362265,4.36906554866025));
#24468=CARTESIAN_POINT('Ctrl Pts',(-0.143407781592193,-0.698141563015474,
4.56758166607191));
#24469=CARTESIAN_POINT('Ctrl Pts',(1.37617826049345,3.48684345900968,4.76609778348356));
#24470=CARTESIAN_POINT('Ctrl Pts',(5.71663606344787,4.47864357428809,4.96461390089523));
#24471=CARTESIAN_POINT('Ctrl Pts',(8.90305693908813,1.36898709382619,5.16313001830687));
#24472=CARTESIAN_POINT('Ctrl Pts',(8.01737725983028,-2.99436172457643,5.36164613571854));
#24473=CARTESIAN_POINT('Ctrl Pts',(3.87068562947579,-4.61553103529222,5.56016225313019));
#24474=CARTESIAN_POINT('Ctrl Pts',(0.260443364168955,-2.00988482013811,
5.75867837054185));
#24475=CARTESIAN_POINT('Ctrl Pts',(0.492841656646439,2.436375680996,5.95719448795349));
#24476=CARTESIAN_POINT('Ctrl Pts',(4.35505457120696,4.6514496783783,6.15571060536516));
#24477=CARTESIAN_POINT('Ctrl Pts',(8.31014098784587,2.60681454019155,6.35422672277681));
#24478=CARTESIAN_POINT('Ctrl Pts',(8.73610799988966,-1.82509176699825,6.55274284018847));
#24479=CARTESIAN_POINT('Ctrl Pts',(5.24286312047947,-4.58561375091533,6.75125895760012));
#24480=CARTESIAN_POINT('Ctrl Pts',(1.02945356160573,-3.14671788935761,6.94977507501179));
#24481=CARTESIAN_POINT('Ctrl Pts',(-0.0455603502579819,1.17388235834786,
7.14829119242343));
#24482=CARTESIAN_POINT('Ctrl Pts',(3.00229867643747,4.41946347189101,7.34680730983509));
#24483=CARTESIAN_POINT('Ctrl Pts',(7.38185932147204,3.61778400498435,7.54532342724674));
#24484=CARTESIAN_POINT('Ctrl Pts',(9.08240325419932,-0.496993236137507,
7.7438395446584));
#24485=CARTESIAN_POINT('Ctrl Pts',(6.5466046888036,-4.15663352541875,7.94235566207006));
#24486=CARTESIAN_POINT('Ctrl Pts',(2.09669971547073,-4.00970789967487,8.1408717794817));
#24487=CARTESIAN_POINT('Ctrl Pts',(-0.192173337388976,-0.19076805214061,
8.33938789689338));
#24488=CARTESIAN_POINT('Ctrl Pts',(1.77609193305126,3.80287354875093,8.53790401430502));
#24489=CARTESIAN_POINT('Ctrl Pts',(6.1989956324977,4.3139158920216,8.73642013171668));
#24490=CARTESIAN_POINT('Ctrl Pts',(9.0261266855466,0.874356120760312,8.93493624912834));
#24491=CARTESIAN_POINT('Ctrl Pts',(7.66845225155073,-3.36592235387631,9.13345236653999));
#24492=CARTESIAN_POINT('Ctrl Pts',(3.36930475145732,-4.52375316346519,9.33196848395166));
#24493=CARTESIAN_POINT('Ctrl Pts',(0.0657616873951493,-1.53881687686219,
9.53048460136329));
#24494=CARTESIAN_POINT('Ctrl Pts',(0.783144957380055,2.85533863417045,9.72900071877498));
#24495=CARTESIAN_POINT('Ctrl Pts',(4.86448860883662,4.63462933832978,9.92751683618659));
#24496=CARTESIAN_POINT('Ctrl Pts',(8.57217576114917,2.16961465444475,10.1260329535983));
#24497=CARTESIAN_POINT('Ctrl Pts',(8.51077704791793,-2.28229185953398,10.3245490710099));
#24498=CARTESIAN_POINT('Ctrl Pts',(4.73652024279266,-4.644118902346,10.5230651884216));
#24499=CARTESIAN_POINT('Ctrl Pts',(0.705797933930029,-2.75295019489822,
10.7215813058332));
#24500=CARTESIAN_POINT('Ctrl Pts',(0.109868939318185,1.65931793437198,10.9200974232449));
#24501=CARTESIAN_POINT('Ctrl Pts',(3.49447369645122,4.55201426291826,11.1186135406565));
#24502=CARTESIAN_POINT('Ctrl Pts',(7.76005555075585,3.27606251797663,11.3171296580682));
#24503=CARTESIAN_POINT('Ctrl Pts',(9.00027578003045,-1.00004496361109,11.5156457754798));
#24504=CARTESIAN_POINT('Ctrl Pts',(6.07936428979557,-4.36033029039609,11.7141618928915));
#24505=CARTESIAN_POINT('Ctrl Pts',(1.67223626118035,-3.72750807951321,11.9126780103032));
#24506=CARTESIAN_POINT('Ctrl Pts',(-0.185144289673645,0.31889512586586,
12.1111941277148));
#24507=CARTESIAN_POINT('Ctrl Pts',(2.20817641458127,4.07326024100545,12.3097102451265));
#24508=CARTESIAN_POINT('Ctrl Pts',(6.66044079877556,4.09741110905781,12.5082263625381));
#24509=CARTESIAN_POINT('Ctrl Pts',(9.09434983091284,0.369230824458725,12.7067424799498));
#24510=CARTESIAN_POINT('Ctrl Pts',(7.28097591722075,-3.69708402566464,12.9052585973614));
#24511=CARTESIAN_POINT('Ctrl Pts',(2.8809723938291,-4.37767965107946,13.1037747147731));
#24512=CARTESIAN_POINT('Ctrl Pts',(-0.0762212094817758,-1.04927952433239,
13.3022908321848));
#24513=CARTESIAN_POINT('Ctrl Pts',(1.11753675741321,3.24003083138531,13.5008069495964));
#24514=CARTESIAN_POINT('Ctrl Pts',(5.369025456116,4.5621825836419,13.6993230670081));
#24515=CARTESIAN_POINT('Ctrl Pts',(8.78481240824481,1.70637430771384,13.8978391844197));
#24516=CARTESIAN_POINT('Ctrl Pts',(8.23678489819753,-2.71209910053747,14.0963553018314));
#24517=CARTESIAN_POINT('Ctrl Pts',(4.22681609508684,-4.64688374211174,14.294871419243));
#24518=CARTESIAN_POINT('Ctrl Pts',(0.427159151106815,-2.32614064576156,
14.4933875366547));
#24519=CARTESIAN_POINT('Ctrl Pts',(0.317467618415429,2.12483780609018,14.6919036540663));
#24520=CARTESIAN_POINT('Ctrl Pts',(3.99819491609722,4.62993021382537,14.890419771478));
#24521=CARTESIAN_POINT('Ctrl Pts',(8.09860099979244,2.8950206023505,15.0889358888896));
#24522=CARTESIAN_POINT('Ctrl Pts',(8.86361197604717,-1.49109380762589,15.2874520063013));
#24523=CARTESIAN_POINT('Ctrl Pts',(5.59264534485911,-4.5116928721902,15.485968123713));
#24524=CARTESIAN_POINT('Ctrl Pts',(1.2811901266875,-3.40056942590122,15.6844842411246));
#24525=CARTESIAN_POINT('Ctrl Pts',(-0.122405002240585,0.824730814938715,
15.8830003585363));
#24526=CARTESIAN_POINT('Ctrl Pts',(2.66724567793686,4.29475826350135,16.0815164759479));
#24527=CARTESIAN_POINT('Ctrl Pts',(7.09543313909595,3.83172778931411,16.2800325933596));
#24528=CARTESIAN_POINT('Ctrl Pts',(9.10690753736432,-0.140326107135887,
16.4785487107712));
#24529=CARTESIAN_POINT('Ctrl Pts',(6.85959888110794,-3.98387202395643,16.6770648281829));
#24530=CARTESIAN_POINT('Ctrl Pts',(2.41154968938301,-4.179063722519,16.8755809455945));
#24531=CARTESIAN_POINT('Ctrl Pts',(-0.163801198896094,-0.547148358219792,
17.0740970630062));
#24532=CARTESIAN_POINT('Ctrl Pts',(1.49200357138825,3.5858350646717,17.2726131804178));
#24533=CARTESIAN_POINT('Ctrl Pts',(5.86260948835618,4.43497894515246,17.4711292978295));
#24534=CARTESIAN_POINT('Ctrl Pts',(8.94549879098837,1.22265346990726,17.6696454152412));
#24535=CARTESIAN_POINT('Ctrl Pts',(7.91742009870712,-3.10935479574357,17.8681615326528));
#24536=CARTESIAN_POINT('Ctrl Pts',(3.71986832177296,-4.59387508565289,18.0666776500645));
#24537=CARTESIAN_POINT('Ctrl Pts',(0.196881531601468,-1.87141195688986,
18.2651937674761));
#24538=CARTESIAN_POINT('Ctrl Pts',(0.574744016316265,2.56485464396025,18.4637098848878));
#24539=CARTESIAN_POINT('Ctrl Pts',(4.50741650012369,4.6522761505852,18.6622260022994));
#24540=CARTESIAN_POINT('Ctrl Pts',(8.3934323297128,2.47923165417059,18.8607421197111));
#24541=CARTESIAN_POINT('Ctrl Pts',(8.67405212821057,-1.96424603112833,19.0592582371228));
#24542=CARTESIAN_POINT('Ctrl Pts',(5.09228962209667,-4.60890456507674,19.2577743545344));
#24543=CARTESIAN_POINT('Ctrl Pts',(0.928254782143413,-3.0328159689208,19.4562904719461));
#24544=CARTESIAN_POINT('Ctrl Pts',(-0.00470849360073685,1.32066780116548,
19.6548065893577));
#24545=CARTESIAN_POINT('Ctrl Pts',(3.14778981602278,4.46470912096001,19.8533227067694));
#24546=CARTESIAN_POINT('Ctrl Pts',(7.49875172579254,3.52005475507203,20.051838824181));
#24547=CARTESIAN_POINT('Ctrl Pts',(9.06364908309027,-0.648198796048447,
20.2503549415927));
#24548=CARTESIAN_POINT('Ctrl Pts',(6.4093786550744,-4.22284422156345,20.4488710590044));
#24549=CARTESIAN_POINT('Ctrl Pts',(1.96667081116617,-3.93028923259476,20.647387176416));
#24550=CARTESIAN_POINT('Ctrl Pts',(-0.195927116407106,-0.0384501329489085,
20.8459032938277));
#24551=CARTESIAN_POINT('Ctrl Pts',(1.90205092121151,3.88860087953163,21.0444194112393));
#24552=CARTESIAN_POINT('Ctrl Pts',(6.3393165377314,4.25454515162759,21.242935528651));
#24553=CARTESIAN_POINT('Ctrl Pts',(9.05230630112455,0.724257949825445,21.4414516460626));
#24554=CARTESIAN_POINT('Ctrl Pts',(7.55651576606266,-3.46929099370176,21.6399677634743));
#24555=CARTESIAN_POINT('Ctrl Pts',(3.22176150253947,-4.48572906904549,21.838483880886));
#24556=CARTESIAN_POINT('Ctrl Pts',(0.0177289115966501,-1.39422211492368,
22.0369999982976));
#24557=CARTESIAN_POINT('Ctrl Pts',(0.878610280341868,2.97408755340353,22.2355161157093));
#24558=CARTESIAN_POINT('Ctrl Pts',(5.01602646728549,4.61878321962123,22.4340322331209));
#24559=CARTESIAN_POINT('Ctrl Pts',(8.64101112050298,2.03368736229999,22.6325483505326));
#24560=CARTESIAN_POINT('Ctrl Pts',(8.43387092517075,-2.41382509078919,22.8310644679442));
#24561=CARTESIAN_POINT('Ctrl Pts',(4.58430347192829,-4.65079401118156,23.0295805853559));
#24562=CARTESIAN_POINT('Ctrl Pts',(0.617664534920323,-2.6286704174496,23.2280967027675));
#24563=CARTESIAN_POINT('Ctrl Pts',(0.166535948123391,1.80077057177711,23.4266128201792));
#24564=CARTESIAN_POINT('Ctrl Pts',(3.64403475383551,4.58104059437149,23.6251289375908));
#24565=CARTESIAN_POINT('Ctrl Pts',(7.86556810560143,3.16619499327494,23.8236450550025));
#24566=CARTESIAN_POINT('Ctrl Pts',(8.96507004425898,-1.14841087401253,24.0221611724142));
#24567=CARTESIAN_POINT('Ctrl Pts',(5.93576426504054,-4.41090351654891,24.2206772898258));
#24568=CARTESIAN_POINT('Ctrl Pts',(1.55158838794904,-3.63478122412758,24.4191934072375));
#24569=CARTESIAN_POINT('Ctrl Pts',(-0.172046559910909,0.471552713422697,
24.6177095246491));
#24570=CARTESIAN_POINT('Ctrl Pts',(2.34243741690352,4.14307145960353,24.8162256420608));
#24571=CARTESIAN_POINT('Ctrl Pts',(6.79403703197597,4.02620936921257,25.0147417594724));
#24572=CARTESIAN_POINT('Ctrl Pts',(9.10329134237422,0.209832038399488,25.2133007328261));
#24573=CARTESIAN_POINT('Ctrl Pts',(7.80718744833136,-2.44564931016495,25.3456876670425));
#24574=CARTESIAN_POINT('Ctrl Pts',(6.7401774553626,-3.20569558398784,25.4119025621217));
#24575=CARTESIAN_POINT('Ctrl Pts',(2.17296269996979,-3.20554048108048,-0.411765747138983));
#24576=CARTESIAN_POINT('Ctrl Pts',(1.10598262521586,-2.44554835076675,-0.345549597099719));
#24577=CARTESIAN_POINT('Ctrl Pts',(-0.190085171851759,0.209786400507346,
-0.213161407923235));
#24578=CARTESIAN_POINT('Ctrl Pts',(2.11904905146237,4.02596493684606,-0.0146011796095345));
#24579=CARTESIAN_POINT('Ctrl Pts',(6.57036830017086,4.14281137096193,0.183914937802122));
#24580=CARTESIAN_POINT('Ctrl Pts',(9.08469850437939,0.471525498888313,0.382431055213778));
#24581=CARTESIAN_POINT('Ctrl Pts',(7.36116941620609,-3.63455711911314,0.580947172625436));
#24582=CARTESIAN_POINT('Ctrl Pts',(2.97726580402431,-4.41062931823268,0.77946329003709));
#24583=CARTESIAN_POINT('Ctrl Pts',(-0.0518523842630756,-1.14834011450979,
0.977979407448747));
#24584=CARTESIAN_POINT('Ctrl Pts',(1.04758148582589,3.16599895701937,1.1764955248604));
#24585=CARTESIAN_POINT('Ctrl Pts',(5.26885307852876,4.58075644304919,1.37501164227206));
#24586=CARTESIAN_POINT('Ctrl Pts',(8.74613631193873,1.80065901519612,1.57352775968371));
#24587=CARTESIAN_POINT('Ctrl Pts',(8.2950356860829,-2.62850749839492,1.77204387709537));
#24588=CARTESIAN_POINT('Ctrl Pts',(4.32864266632258,-4.6505056552148,1.97055999450703));
#24589=CARTESIAN_POINT('Ctrl Pts',(0.479313869061077,-2.41367545883394,
2.16907611191868));
#24590=CARTESIAN_POINT('Ctrl Pts',(0.272186515624751,2.03356129066451,2.36759222933034));
#24591=CARTESIAN_POINT('Ctrl Pts',(3.89694643539194,4.61849687019083,2.56610834674199));
#24592=CARTESIAN_POINT('Ctrl Pts',(8.03410612006349,2.97390317522259,2.76462446415365));
#24593=CARTESIAN_POINT('Ctrl Pts',(8.89493411795877,-1.39413568050936,2.9631405815653));
#24594=CARTESIAN_POINT('Ctrl Pts',(5.69110016326603,-4.48545097223521,3.16165669897696));
#24595=CARTESIAN_POINT('Ctrl Pts',(1.35661463604595,-3.46907591290164,3.36017281638862));
#24596=CARTESIAN_POINT('Ctrl Pts',(-0.139083166427389,0.724213049156903,
3.55868893380027));
#24597=CARTESIAN_POINT('Ctrl Pts',(2.57373840321099,4.25428138787658,3.75720505121192));
#24598=CARTESIAN_POINT('Ctrl Pts',(7.01072892820446,3.88835980295648,3.95572116862359));
#24599=CARTESIAN_POINT('Ctrl Pts',(9.10857690015422,-0.0384477492421469,
4.15423728603523));
#24600=CARTESIAN_POINT('Ctrl Pts',(6.94611304441007,-3.93004557143118,4.3527534034469));
#24601=CARTESIAN_POINT('Ctrl Pts',(2.50368062941278,-4.22258242327136,4.55126952085854));
#24602=CARTESIAN_POINT('Ctrl Pts',(-0.15042524517621,-0.648158610486061,
4.74978563827021));
#24603=CARTESIAN_POINT('Ctrl Pts',(1.41437509517098,3.51983652671062,4.94830175568186));
#24604=CARTESIAN_POINT('Ctrl Pts',(5.76506726388787,4.46443232806813,5.14681787309352));
#24605=CARTESIAN_POINT('Ctrl Pts',(8.91737013208296,1.32058592540232,5.34533399050517));
#24606=CARTESIAN_POINT('Ctrl Pts',(7.98446469607637,-3.03262794728552,5.54385010791683));
#24607=CARTESIAN_POINT('Ctrl Pts',(3.82068800849579,-4.60861883268182,5.74236622532849));
#24608=CARTESIAN_POINT('Ctrl Pts',(0.239147556357015,-1.9641242562649,5.94088234274014));
#24609=CARTESIAN_POINT('Ctrl Pts',(0.519749957626067,2.47907795239849,6.13939846015179));
#24610=CARTESIAN_POINT('Ctrl Pts',(4.40552487083362,4.65198772933701,6.33791457756345));
#24611=CARTESIAN_POINT('Ctrl Pts',(8.33795354574623,2.56469563392857,6.53643069497511));
#24612=CARTESIAN_POINT('Ctrl Pts',(8.71579260460107,-1.87129593734266,6.73494681238676));
#24613=CARTESIAN_POINT('Ctrl Pts',(5.19302422456139,-4.59359028502123,6.93346292979842));
#24614=CARTESIAN_POINT('Ctrl Pts',(0.995732677906764,-3.10916202902842,
7.13197904721008));
#24615=CARTESIAN_POINT('Ctrl Pts',(-0.0322822778871914,1.22257767061497,
7.33049516462173));
#24616=CARTESIAN_POINT('Ctrl Pts',(3.05041589877745,4.43470399540276,7.52901128203338));
#24617=CARTESIAN_POINT('Ctrl Pts',(7.42075085684839,3.58561275821527,7.72752739944505));
#24618=CARTESIAN_POINT('Ctrl Pts',(9.07645297431008,-0.547114437358846,
7.9260435168567));
#24619=CARTESIAN_POINT('Ctrl Pts',(6.5012617467849,-4.17880463841992,8.12455963426836));
#24620=CARTESIAN_POINT('Ctrl Pts',(2.05348831510913,-3.98362504090881,8.32307575168001));
#24621=CARTESIAN_POINT('Ctrl Pts',(-0.193681017610346,-0.140317407516647,
8.52159186909167));
#24622=CARTESIAN_POINT('Ctrl Pts',(1.81766867783776,3.83149023855917,8.72010798650331));
#24623=CARTESIAN_POINT('Ctrl Pts',(6.24558161029013,4.2944920068349,8.91862410391498));
#24624=CARTESIAN_POINT('Ctrl Pts',(9.03505934404192,0.824679685151172,9.11714022132663));
#24625=CARTESIAN_POINT('Ctrl Pts',(7.6315512320161,-3.40035860512303,9.31565633873829));
#24626=CARTESIAN_POINT('Ctrl Pts',(3.32036330565075,-4.51141316650472,9.51417245614994));
#24627=CARTESIAN_POINT('Ctrl Pts',(0.0495994604212725,-1.49100136617927,
9.71268857356161));
#24628=CARTESIAN_POINT('Ctrl Pts',(0.814563009263402,2.89484112343983,9.91120469097325));
#24629=CARTESIAN_POINT('Ctrl Pts',(4.91471488529713,4.62964317792977,10.1097208083849));
#24630=CARTESIAN_POINT('Ctrl Pts',(8.59521399360942,2.1247060752228,10.3082369257966));
#24631=CARTESIAN_POINT('Ctrl Pts',(8.48552926132444,-2.32599643497811,10.5067530432082));
#24632=CARTESIAN_POINT('Ctrl Pts',(4.68610787984395,-4.64659565516981,10.7052691606199));
#24633=CARTESIAN_POINT('Ctrl Pts',(0.676387677669684,-2.71193096197848,
10.9037852780315));
#24634=CARTESIAN_POINT('Ctrl Pts',(0.128394142987057,1.70626851979591,11.1023013954432));
#24635=CARTESIAN_POINT('Ctrl Pts',(3.54396933091606,4.56189974780998,11.3008175128549));
#24636=CARTESIAN_POINT('Ctrl Pts',(7.79519445548059,3.23982996331418,11.4993336302665));
#24637=CARTESIAN_POINT('Ctrl Pts',(8.98887841448097,-1.04921447348414,11.6978497476782));
#24638=CARTESIAN_POINT('Ctrl Pts',(6.03186814454124,-4.3774082536412,11.8963658650898));
#24639=CARTESIAN_POINT('Ctrl Pts',(1.63213740257258,-3.69685482224785,12.0948819825015));
#24640=CARTESIAN_POINT('Ctrl Pts',(-0.181124089683036,0.369207933724872,
12.2933980999131));
#24641=CARTESIAN_POINT('Ctrl Pts',(2.2526340504912,4.09715708707193,12.4919142173248));
#24642=CARTESIAN_POINT('Ctrl Pts',(6.70462241331237,4.07300771627025,12.6904303347364));
#24643=CARTESIAN_POINT('Ctrl Pts',(9.09779474190718,0.318875355730261,12.8889464521481));
#24644=CARTESIAN_POINT('Ctrl Pts',(7.24052934071316,-3.72727698993507,13.0874625695597));
#24645=CARTESIAN_POINT('Ctrl Pts',(2.83367453520978,-4.36005996854408,13.2859786869714));
#24646=CARTESIAN_POINT('Ctrl Pts',(-0.0870558709899348,-0.999982965095223,
13.4844948043831));
#24647=CARTESIAN_POINT('Ctrl Pts',(1.1530874699283,3.2758594160949,13.6830109217947));
#24648=CARTESIAN_POINT('Ctrl Pts',(5.41840487637927,4.55173205747878,13.8815270392064));
#24649=CARTESIAN_POINT('Ctrl Pts',(8.80279980247531,1.65921506374814,14.080043156618));
#24650=CARTESIAN_POINT('Ctrl Pts',(8.20690775291552,-2.75277952374592,14.2785592740297));
#24651=CARTESIAN_POINT('Ctrl Pts',(4.17643533161801,-4.64383098681233,14.4770753914414));
#24652=CARTESIAN_POINT('Ctrl Pts',(0.402412514292184,-2.28215036718792,
14.675591508853));
#24653=CARTESIAN_POINT('Ctrl Pts',(0.341017607518878,2.16948014760412,14.8741076262646));
#24654=CARTESIAN_POINT('Ctrl Pts',(4.04847489906614,4.63434201110855,15.0726237436763));
#24655=CARTESIAN_POINT('Ctrl Pts',(8.12956552465056,2.85516161537223,15.271139861088));
#24656=CARTESIAN_POINT('Ctrl Pts',(8.84690431993714,-1.53872147678918,15.4696559784996));
#24657=CARTESIAN_POINT('Ctrl Pts',(5.54356606143321,-4.52347271009317,15.6681720959113));
#24658=CARTESIAN_POINT('Ctrl Pts',(1.24468509012015,-3.36571368106855,15.8666882133229));
#24659=CARTESIAN_POINT('Ctrl Pts',(-0.112905173860372,0.874301914415817,
16.0652043307346));
#24660=CARTESIAN_POINT('Ctrl Pts',(2.71405060913991,4.31364844766405,16.2637204481462));
#24661=CARTESIAN_POINT('Ctrl Pts',(7.1366801074503,3.80263778683562,16.4622365655579));
#24662=CARTESIAN_POINT('Ctrl Pts',(9.10482335385156,-0.190756225336315,
16.6607526829696));
#24663=CARTESIAN_POINT('Ctrl Pts',(6.81609220134375,-4.00945931491334,16.8592688003812));
#24664=CARTESIAN_POINT('Ctrl Pts',(2.36646310311057,-4.15637583189606,17.0577849177929));
#24665=CARTESIAN_POINT('Ctrl Pts',(-0.16917825360623,-0.496962424679848,
17.2563010352045));
#24666=CARTESIAN_POINT('Ctrl Pts',(1.53126025266144,3.61755971783011,17.4548171526162));
#24667=CARTESIAN_POINT('Ctrl Pts',(5.91054938364417,4.41918948403437,17.6533332700278));
#24668=CARTESIAN_POINT('Ctrl Pts',(8.95821945609951,1.17380958265607,17.8518493874395));
#24669=CARTESIAN_POINT('Ctrl Pts',(7.88327219050615,-3.14652280629029,18.0503655048511));
#24670=CARTESIAN_POINT('Ctrl Pts',(3.67012384502666,-4.58532946245115,18.2488816222628));
#24671=CARTESIAN_POINT('Ctrl Pts',(0.177095531876928,-1.82497861910485,
18.4473977396744));
#24672=CARTESIAN_POINT('Ctrl Pts',(0.603036135785551,2.60665292882547,18.6459138570862));
#24673=CARTESIAN_POINT('Ctrl Pts',(4.55787735396168,4.65116130836808,18.8444299744978));
#24674=CARTESIAN_POINT('Ctrl Pts',(8.41985082781949,2.43622463611074,19.0429460919094));
#24675=CARTESIAN_POINT('Ctrl Pts',(8.65223471259592,-2.00976021586402,19.2414622093211));
#24676=CARTESIAN_POINT('Ctrl Pts',(5.04221626688697,-4.61524489208584,19.4399783267328));
#24677=CARTESIAN_POINT('Ctrl Pts',(0.895781713701428,-2.99417608693739,
19.6384944441444));
#24678=CARTESIAN_POINT('Ctrl Pts',(0.0101569427980723,1.36890222246852,
19.8370105615561));
#24679=CARTESIAN_POINT('Ctrl Pts',(3.1963802739596,4.47836591752857,20.0355266789677));
#24680=CARTESIAN_POINT('Ctrl Pts',(7.53656898706393,3.48662728959027,20.2340427963793));
#24681=CARTESIAN_POINT('Ctrl Pts',(9.05606082131957,-0.698098281184544,
20.432558913791));
#24682=CARTESIAN_POINT('Ctrl Pts',(6.36333405195284,-4.24351873734398,20.6310750312027));
#24683=CARTESIAN_POINT('Ctrl Pts',(1.9243366462227,-3.90280543100934,20.8295911486144));
#24684=CARTESIAN_POINT('Ctrl Pts',(-0.195782035254683,0.0120228054752082,
21.028107266026));
#24685=CARTESIAN_POINT('Ctrl Pts',(1.94454241477252,3.91584087042925,21.2266233834376));
#24686=CARTESIAN_POINT('Ctrl Pts',(6.38524148680512,4.23360619038166,21.4251395008493));
#24687=CARTESIAN_POINT('Ctrl Pts',(9.05960761710739,0.674315805600993,21.623655618261));
#24688=CARTESIAN_POINT('Ctrl Pts',(7.5185068390623,-3.50250076674849,21.8221717356726));
#24689=CARTESIAN_POINT('Ctrl Pts',(3.17325057532877,-4.47179261159471,22.0206878530843));
#24690=CARTESIAN_POINT('Ctrl Pts',(0.0031406198327811,-1.34590405051051,
22.2192039704959));
#24691=CARTESIAN_POINT('Ctrl Pts',(0.911305739869395,3.01254206724522,22.4177200879076));
#24692=CARTESIAN_POINT('Ctrl Pts',(5.06606104496655,4.6121513544261,22.6162362053192));
#24693=CARTESIAN_POINT('Ctrl Pts',(8.66256938155685,1.98805571626367,22.8147523227309));
#24694=CARTESIAN_POINT('Ctrl Pts',(8.4072000996685,-2.45669335535235,23.0132684401425));
#24695=CARTESIAN_POINT('Ctrl Pts',(4.53384760969594,-4.65159218721967,23.2117845575542));
#24696=CARTESIAN_POINT('Ctrl Pts',(0.589592923617338,-2.58676106216746,
23.4103006749659));
#24697=CARTESIAN_POINT('Ctrl Pts',(0.186627431348294,1.84718698340797,23.6088167923775));
#24698=CARTESIAN_POINT('Ctrl Pts',(3.69375302108596,4.58911293885384,23.8073329097892));
#24699=CARTESIAN_POINT('Ctrl Pts',(7.89964467060016,3.12919021086655,24.0058490272008));
#24700=CARTESIAN_POINT('Ctrl Pts',(8.95179466357075,-1.19786968887199,24.2043651446125));
#24701=CARTESIAN_POINT('Ctrl Pts',(5.88826072308503,-4.42509080397621,24.4028812620241));
#24702=CARTESIAN_POINT('Ctrl Pts',(1.51149918181804,-3.60542346049212,24.6013973794358));
#24703=CARTESIAN_POINT('Ctrl Pts',(-0.164376056275096,0.527120914407128,
24.7999134968474));
#24704=CARTESIAN_POINT('Ctrl Pts',(1.53399129555416,2.94325066577138,24.9322575751219));
#24705=CARTESIAN_POINT('Ctrl Pts',(2.70656526709436,3.52529833870864,24.9984296142591));
#24706=CARTESIAN_POINT('Ctrl Pts',(2.31196529717974,-3.01041142380583,-0.273445981108207));
#24707=CARTESIAN_POINT('Ctrl Pts',(1.30993489857133,-2.29668186568531,-0.207229831068943));
#24708=CARTESIAN_POINT('Ctrl Pts',(0.0927619053280601,0.197016191301887,
-0.0748416418924601));
#24709=CARTESIAN_POINT('Ctrl Pts',(2.26133350378215,3.78089464452436,0.123718586421241));
#24710=CARTESIAN_POINT('Ctrl Pts',(6.44169010710979,3.89062835157607,0.322234703832897));
#24711=CARTESIAN_POINT('Ctrl Pts',(8.80296690727615,0.442822593209179,0.520750821244553));
#24712=CARTESIAN_POINT('Ctrl Pts',(7.18435323294509,-3.41331277406459,0.719266938656211));
#24713=CARTESIAN_POINT('Ctrl Pts',(3.06730851213489,-4.14214356803415,0.917783056067867));
#24714=CARTESIAN_POINT('Ctrl Pts',(0.222580126422941,-1.07843785456408,
1.11629917347952));
#24715=CARTESIAN_POINT('Ctrl Pts',(1.25508877879203,2.97327688863128,1.31481529089117));
#24716=CARTESIAN_POINT('Ctrl Pts',(5.21940128729496,4.30191464036023,1.51333140830283));
#24717=CARTESIAN_POINT('Ctrl Pts',(8.48501382017349,1.69104851481962,1.71184752571448));
#24718=CARTESIAN_POINT('Ctrl Pts',(8.06137278822348,-2.46850384433775,1.91036364312614));
#24719=CARTESIAN_POINT('Ctrl Pts',(4.33642377308406,-4.36741804808325,2.1088797605378));
#24720=CARTESIAN_POINT('Ctrl Pts',(0.721412996069988,-2.26674915432179,
2.30739587794946));
#24721=CARTESIAN_POINT('Ctrl Pts',(0.526893989166935,1.90977346146706,2.50591199536111));
#24722=CARTESIAN_POINT('Ctrl Pts',(3.93100594327419,4.33735771577206,2.70442811277276));
#24723=CARTESIAN_POINT('Ctrl Pts',(7.81632664047099,2.79287444498747,2.90294423018442));
#24724=CARTESIAN_POINT('Ctrl Pts',(8.62475394129306,-1.30927124574203,3.10146034759608));
#24725=CARTESIAN_POINT('Ctrl Pts',(5.61594516345689,-4.21241064570382,3.29997646500774));
#24726=CARTESIAN_POINT('Ctrl Pts',(1.54531032840212,-3.25790481196126,3.49849258241939));
#24727=CARTESIAN_POINT('Ctrl Pts',(0.140659294449413,0.680128436785933,
3.69700869983105));
#24728=CARTESIAN_POINT('Ctrl Pts',(2.68834480713824,3.99531291703776,3.8955248172427));
#24729=CARTESIAN_POINT('Ctrl Pts',(6.85524491106594,3.65166587031902,4.09404093465435));
#24730=CARTESIAN_POINT('Ctrl Pts',(8.82539176693615,-0.0361073410931478,
4.29255705206602));
#24731=CARTESIAN_POINT('Ctrl Pts',(6.79456235351217,-3.69081412452673,4.49107316947766));
#24732=CARTESIAN_POINT('Ctrl Pts',(2.62255162068078,-3.96554354562172,4.68958928688933));
#24733=CARTESIAN_POINT('Ctrl Pts',(0.130007635661538,-0.608703617053558,
4.88810540430098));
#24734=CARTESIAN_POINT('Ctrl Pts',(1.59955476768487,3.30557550356288,5.08662152171263));
#24735=CARTESIAN_POINT('Ctrl Pts',(5.68540970649173,4.19267145760527,5.28513763912429));
#24736=CARTESIAN_POINT('Ctrl Pts',(8.64582422058695,1.24019864338394,5.48365375653594));
#24737=CARTESIAN_POINT('Ctrl Pts',(7.76970701088062,-2.84802449713069,5.68216987394761));
#24738=CARTESIAN_POINT('Ctrl Pts',(3.85938955257665,-4.32808097846753,5.88068599135924));
#24739=CARTESIAN_POINT('Ctrl Pts',(0.495866191827503,-1.844563228489,6.07920210877092));
#24740=CARTESIAN_POINT('Ctrl Pts',(0.759387641428115,2.32817043879295,6.27771822618256));
#24741=CARTESIAN_POINT('Ctrl Pts',(4.40862597053364,4.36880990474354,6.47623434359423));
#24742=CARTESIAN_POINT('Ctrl Pts',(8.10167813322798,2.40857636349708,6.67475046100588));
#24743=CARTESIAN_POINT('Ctrl Pts',(8.45651720821394,-1.75738559545474,6.87326657841754));
#24744=CARTESIAN_POINT('Ctrl Pts',(5.14818832037566,-4.31396725511023,7.0717826958292));
#24745=CARTESIAN_POINT('Ctrl Pts',(1.20639613410644,-2.9198997628929,7.27029881324085));
#24746=CARTESIAN_POINT('Ctrl Pts',(0.240958952754043,1.14815638979818,7.4688149306525));
#24747=CARTESIAN_POINT('Ctrl Pts',(3.13600578243834,4.16475276096279,7.66733104806417));
#24748=CARTESIAN_POINT('Ctrl Pts',(7.24030780616454,3.36734777563528,7.86584716547581));
#24749=CARTESIAN_POINT('Ctrl Pts',(8.79522330270695,-0.513810248872322,
8.06436328288747));
#24750=CARTESIAN_POINT('Ctrl Pts',(6.37679023796107,-3.92443062116999,8.26287940029913));
#24751=CARTESIAN_POINT('Ctrl Pts',(2.1997636091463,-3.74113208118609,8.46139551771078));
#24752=CARTESIAN_POINT('Ctrl Pts',(0.089384947459713,-0.131775945129999,
8.65991163512245));
#24753=CARTESIAN_POINT('Ctrl Pts',(1.97829888761515,3.5982580948319,8.8584277525341));
#24754=CARTESIAN_POINT('Ctrl Pts',(6.13667397417128,4.03307581767334,9.05694386994575));
#24755=CARTESIAN_POINT('Ctrl Pts',(8.75634940354159,0.774479423926291,9.2554599873574));
#24756=CARTESIAN_POINT('Ctrl Pts',(7.43827624901926,-3.19337049409171,9.45397610476906));
#24757=CARTESIAN_POINT('Ctrl Pts',(3.38952083310589,-4.23679245796831,9.65249222218073));
#24758=CARTESIAN_POINT('Ctrl Pts',(0.317856350200649,-1.40024048117564,
9.85100833959237));
#24759=CARTESIAN_POINT('Ctrl Pts',(1.03625470449417,2.71862509287945,10.049524457004));
#24760=CARTESIAN_POINT('Ctrl Pts',(4.88682034851015,4.34782552060827,10.2480405744157));
#24761=CARTESIAN_POINT('Ctrl Pts',(8.34327851098385,1.99537004097493,10.4465566918273));
#24762=CARTESIAN_POINT('Ctrl Pts',(8.24027055552775,-2.18440736622039,10.645072809239));
#24763=CARTESIAN_POINT('Ctrl Pts',(4.67212920832948,-4.36374605926514,10.8435889266506));
#24764=CARTESIAN_POINT('Ctrl Pts',(0.906490441907856,-2.54684911848653,
11.0421050440623));
#24765=CARTESIAN_POINT('Ctrl Pts',(0.391854608507251,1.60240379879482,11.2406211614739));
#24766=CARTESIAN_POINT('Ctrl Pts',(3.59951541494433,4.28420579809219,11.4391372788856));
#24767=CARTESIAN_POINT('Ctrl Pts',(7.59195811086242,3.04261362173219,11.6376533962972));
#24768=CARTESIAN_POINT('Ctrl Pts',(8.71297961965247,-0.98534623276214,11.8361695137089));
#24769=CARTESIAN_POINT('Ctrl Pts',(5.93596976765481,-4.11094475056566,12.0346856311206));
#24770=CARTESIAN_POINT('Ctrl Pts',(1.80406135300024,-3.47181826426207,12.2332017485322));
#24771=CARTESIAN_POINT('Ctrl Pts',(0.101177504597399,0.346733347466743,
12.4317178659439));
#24772=CARTESIAN_POINT('Ctrl Pts',(2.38678685852808,3.84775315515312,12.6302339833555));
#24773=CARTESIAN_POINT('Ctrl Pts',(6.56777184536255,3.82507381537617,12.8287501007672));
#24774=CARTESIAN_POINT('Ctrl Pts',(8.81526594492522,0.29946463609684,13.0272662181788));
#24775=CARTESIAN_POINT('Ctrl Pts',(7.07105681270762,-3.5003885604986,13.2257823355905));
#24776=CARTESIAN_POINT('Ctrl Pts',(2.93245799361878,-4.09465249784007,13.4242984530022));
#24777=CARTESIAN_POINT('Ctrl Pts',(0.189519561683291,-0.939111566208993,
13.6228145704138));
#24778=CARTESIAN_POINT('Ctrl Pts',(1.35417235664619,3.07644987396012,13.8213306878255));
#24779=CARTESIAN_POINT('Ctrl Pts',(5.3598495029257,4.27465703983832,14.0198468052371));
#24780=CARTESIAN_POINT('Ctrl Pts',(8.53822806601778,1.55821460123144,14.2183629226488));
#24781=CARTESIAN_POINT('Ctrl Pts',(7.97860941701375,-2.58521112879858,14.4168790400604));
#24782=CARTESIAN_POINT('Ctrl Pts',(4.19348166959603,-4.36114968300486,14.6153951574721));
#24783=CARTESIAN_POINT('Ctrl Pts',(0.649192814085452,-2.14323031537866,
14.8139112748837));
#24784=CARTESIAN_POINT('Ctrl Pts',(0.59153516483578,2.03741860650786,15.0124273922954));
#24785=CARTESIAN_POINT('Ctrl Pts',(4.07331050026509,4.35223832436584,15.2109435097071));
#24786=CARTESIAN_POINT('Ctrl Pts',(7.9059751985768,2.68136097312093,15.4094596271187));
#24787=CARTESIAN_POINT('Ctrl Pts',(8.57964783407003,-1.44505575241412,15.6079757445304));
#24788=CARTESIAN_POINT('Ctrl Pts',(5.47739182177246,-4.24811790776339,15.806491861942));
#24789=CARTESIAN_POINT('Ctrl Pts',(1.44019420657955,-3.16083449095397,16.0050079793537));
#24790=CARTESIAN_POINT('Ctrl Pts',(0.165243768843413,0.821081027223728,
16.2035240967653));
#24791=CARTESIAN_POINT('Ctrl Pts',(2.82011586731386,4.05106615928717,16.402040214177));
#24792=CARTESIAN_POINT('Ctrl Pts',(6.97352913523386,3.57116196212476,16.6005563315886));
#24793=CARTESIAN_POINT('Ctrl Pts',(8.82186670813997,-0.17914442924803,16.7990724490003));
#24794=CARTESIAN_POINT('Ctrl Pts',(6.67245619587356,-3.76539376000376,16.997588566412));
#24795=CARTESIAN_POINT('Ctrl Pts',(2.49368685944485,-3.90336711073225,17.1961046838236));
#24796=CARTESIAN_POINT('Ctrl Pts',(0.112396168534027,-0.466711111367439,
17.3946208012353));
#24797=CARTESIAN_POINT('Ctrl Pts',(1.70932484092508,3.39735004600064,17.5931369186469));
#24798=CARTESIAN_POINT('Ctrl Pts',(5.82203597524696,4.15018265569229,17.7916530360586));
#24799=CARTESIAN_POINT('Ctrl Pts',(8.68418694674809,1.10235693414467,17.9901691534703));
#24800=CARTESIAN_POINT('Ctrl Pts',(7.67467433961344,-2.9549862986379,18.1886852708819));
#24801=CARTESIAN_POINT('Ctrl Pts',(3.71799059648846,-4.30620928893205,18.3872013882936));
#24802=CARTESIAN_POINT('Ctrl Pts',(0.437591425226463,-1.7138877251997,18.5857175057052));
#24803=CARTESIAN_POINT('Ctrl Pts',(0.837603987051035,2.44797961565228,18.7842336231169));
#24804=CARTESIAN_POINT('Ctrl Pts',(4.55170438690705,4.36803379003202,18.9827497405285));
#24805=CARTESIAN_POINT('Ctrl Pts',(8.17859012825258,2.28792570825151,19.1812658579402));
#24806=CARTESIAN_POINT('Ctrl Pts',(8.39682823991214,-1.88742121606535,19.3797819753518));
#24807=CARTESIAN_POINT('Ctrl Pts',(5.0065604104293,-4.33430369349561,19.5782980927635));
#24808=CARTESIAN_POINT('Ctrl Pts',(1.11252942855707,-2.81191329518458,19.7768142101752));
#24809=CARTESIAN_POINT('Ctrl Pts',(0.280814794700937,1.28557380975688,19.9753303275868));
#24810=CARTESIAN_POINT('Ctrl Pts',(3.27308495055695,4.20575687553525,20.1738464449984));
#24811=CARTESIAN_POINT('Ctrl Pts',(7.34907580467911,3.27438779359847,20.3723625624101));
#24812=CARTESIAN_POINT('Ctrl Pts',(8.77607246974106,-0.65560333835151,20.5708786798217));
#24813=CARTESIAN_POINT('Ctrl Pts',(6.24725853788356,-3.98520541525919,20.7693947972334));
#24814=CARTESIAN_POINT('Ctrl Pts',(2.07847371693811,-3.66523215780504,20.9679109146451));
#24815=CARTESIAN_POINT('Ctrl Pts',(0.0874118238771355,0.0112909480203034,
21.1664270320568));
#24816=CARTESIAN_POINT('Ctrl Pts',(2.09744951113826,3.6774740982752,21.3649431494684));
#24817=CARTESIAN_POINT('Ctrl Pts',(6.26783241381338,3.97589626917586,21.56345926688));
#24818=CARTESIAN_POINT('Ctrl Pts',(8.77940336342984,0.633268559987037,21.7619753842917));
#24819=CARTESIAN_POINT('Ctrl Pts',(7.33211314362288,-3.28929501353682,21.9604915017033));
#24820=CARTESIAN_POINT('Ctrl Pts',(3.25136321302202,-4.1995837027451,22.159007619115));
#24821=CARTESIAN_POINT('Ctrl Pts',(0.274225572405194,-1.26397559254583,
22.3575237365266));
#24822=CARTESIAN_POINT('Ctrl Pts',(1.12710846943813,2.82916129353447,22.5560398539383));
#24823=CARTESIAN_POINT('Ctrl Pts',(5.0289536987851,4.33139846700858,22.75455597135));
#24824=CARTESIAN_POINT('Ctrl Pts',(8.40653381239982,1.86703792222437,22.9530720887616));
#24825=CARTESIAN_POINT('Ctrl Pts',(8.1667094807393,-2.30714844669435,23.1515882061733));
#24826=CARTESIAN_POINT('Ctrl Pts',(4.52913739170739,-4.36843844023836,23.3501043235849));
#24827=CARTESIAN_POINT('Ctrl Pts',(0.824979095953012,-2.42929861537115,
23.5486204409966));
#24828=CARTESIAN_POINT('Ctrl Pts',(0.44654309475883,1.73474421227166,23.7471365584082));
#24829=CARTESIAN_POINT('Ctrl Pts',(3.74018140704413,4.30976245591016,23.9456526758199));
#24830=CARTESIAN_POINT('Ctrl Pts',(7.69005018696339,2.93870878051704,24.1441687932315));
#24831=CARTESIAN_POINT('Ctrl Pts',(8.67815324699032,-1.12495244308866,24.3426849106432));
#24832=CARTESIAN_POINT('Ctrl Pts',(5.80110407974766,-4.15572474791461,24.5412010280549));
#24833=CARTESIAN_POINT('Ctrl Pts',(1.69076667459873,-3.38595255220879,24.7397171454665));
#24834=CARTESIAN_POINT('Ctrl Pts',(0.116906044416222,0.495033780363739,
24.9382332628782));
#24835=CARTESIAN_POINT('Ctrl Pts',(1.71188963858453,2.76408782845127,25.0705773411526));
#24836=CARTESIAN_POINT('Ctrl Pts',(2.81308617627174,3.31070484176046,25.1367493802898));
#24837=CARTESIAN_POINT('Ctrl Pts',(2.45096789438968,-2.81528236653118,-0.135126215077433));
#24838=CARTESIAN_POINT('Ctrl Pts',(1.5138871719268,-2.14781538060387,-0.0689100650381678));
#24839=CARTESIAN_POINT('Ctrl Pts',(0.375608982507884,0.184245982096433,
0.0634781241383155));
#24840=CARTESIAN_POINT('Ctrl Pts',(2.40361795610193,3.53582435220265,0.262038352452016));
#24841=CARTESIAN_POINT('Ctrl Pts',(6.31301191404873,3.63844533219021,0.460554469863673));
#24842=CARTESIAN_POINT('Ctrl Pts',(8.52123531017291,0.41411968753004,0.659070587275328));
#24843=CARTESIAN_POINT('Ctrl Pts',(7.00753704968407,-3.19206842901602,0.857586704686986));
#24844=CARTESIAN_POINT('Ctrl Pts',(3.15735122024546,-3.87365781783563,1.05610282209864));
#24845=CARTESIAN_POINT('Ctrl Pts',(0.497012637108953,-1.00853559461836,
1.25461893951029));
#24846=CARTESIAN_POINT('Ctrl Pts',(1.46259607175817,2.78055482024318,1.45313505692195));
#24847=CARTESIAN_POINT('Ctrl Pts',(5.16994949606116,4.02307283767128,1.6516511743336));
#24848=CARTESIAN_POINT('Ctrl Pts',(8.22389132840824,1.58143801444312,1.85016729174526));
#24849=CARTESIAN_POINT('Ctrl Pts',(7.82770989036406,-2.30850019028058,2.04868340915692));
#24850=CARTESIAN_POINT('Ctrl Pts',(4.34420487984554,-4.08433044095169,2.24719952656857));
#24851=CARTESIAN_POINT('Ctrl Pts',(0.963512123078899,-2.11982284980964,
2.44571564398023));
#24852=CARTESIAN_POINT('Ctrl Pts',(0.781601462709117,1.78598563226962,2.64423176139188));
#24853=CARTESIAN_POINT('Ctrl Pts',(3.96506545115642,4.05621856135326,2.84274787880354));
#24854=CARTESIAN_POINT('Ctrl Pts',(7.59854716087849,2.61184571475234,3.0412639962152));
#24855=CARTESIAN_POINT('Ctrl Pts',(8.35457376462735,-1.22440681097471,3.23978011362686));
#24856=CARTESIAN_POINT('Ctrl Pts',(5.54079016364776,-3.93937031917242,3.43829623103851));
#24857=CARTESIAN_POINT('Ctrl Pts',(1.7340060207583,-3.04673371102089,3.63681234845017));
#24858=CARTESIAN_POINT('Ctrl Pts',(0.420401755326215,0.636043824414959,
3.83532846586182));
#24859=CARTESIAN_POINT('Ctrl Pts',(2.8029512110655,3.73634444619894,4.03384458327349));
#24860=CARTESIAN_POINT('Ctrl Pts',(6.6997608939274,3.41497193768155,4.23236070068513));
#24861=CARTESIAN_POINT('Ctrl Pts',(8.54220663371807,-0.0337669329441494,
4.4308768180968));
#24862=CARTESIAN_POINT('Ctrl Pts',(6.64301166261426,-3.45158267762228,4.62939293550844));
#24863=CARTESIAN_POINT('Ctrl Pts',(2.74142261194879,-3.70850466797209,4.82790905292011));
#24864=CARTESIAN_POINT('Ctrl Pts',(0.410440516499291,-0.569248623621048,
5.02642517033176));
#24865=CARTESIAN_POINT('Ctrl Pts',(1.78473444019877,3.09131448041513,5.22494128774342));
#24866=CARTESIAN_POINT('Ctrl Pts',(5.60575214909559,3.92091058714242,5.42345740515506));
#24867=CARTESIAN_POINT('Ctrl Pts',(8.37427830909092,1.15981136136555,5.62197352256674));
#24868=CARTESIAN_POINT('Ctrl Pts',(7.55494932568486,-2.66342104697584,5.82048963997839));
#24869=CARTESIAN_POINT('Ctrl Pts',(3.89809109665752,-4.04754312425325,6.01900575739004));
#24870=CARTESIAN_POINT('Ctrl Pts',(0.752584827297987,-1.72500220071308,
6.21752187480171));
#24871=CARTESIAN_POINT('Ctrl Pts',(0.999025325230166,2.17726292518741,6.41603799221334));
#24872=CARTESIAN_POINT('Ctrl Pts',(4.41172707023364,4.08563208015006,6.61455410962502));
#24873=CARTESIAN_POINT('Ctrl Pts',(7.86540272070975,2.25245709306557,6.81307022703666));
#24874=CARTESIAN_POINT('Ctrl Pts',(8.1972418118268,-1.64347525356681,7.01158634444832));
#24875=CARTESIAN_POINT('Ctrl Pts',(5.10335241618994,-4.03434422519923,7.21010246185998));
#24876=CARTESIAN_POINT('Ctrl Pts',(1.4170595903061,-2.73063749675737,7.40861857927163));
#24877=CARTESIAN_POINT('Ctrl Pts',(0.514200183395272,1.07373510898141,7.60713469668328));
#24878=CARTESIAN_POINT('Ctrl Pts',(3.22159566609925,3.89480152652282,7.80565081409495));
#24879=CARTESIAN_POINT('Ctrl Pts',(7.05986475548066,3.14908279305528,8.0041669315066));
#24880=CARTESIAN_POINT('Ctrl Pts',(8.51399363110384,-0.480506060385796,
8.20268304891826));
#24881=CARTESIAN_POINT('Ctrl Pts',(6.25231872913724,-3.67005660392007,8.40119916632992));
#24882=CARTESIAN_POINT('Ctrl Pts',(2.34603890318347,-3.49863912146337,8.59971528374156));
#24883=CARTESIAN_POINT('Ctrl Pts',(0.372450912529775,-0.123234482743352,
8.79823140115322));
#24884=CARTESIAN_POINT('Ctrl Pts',(2.13892909739252,3.36502595110463,8.99674751856487));
#24885=CARTESIAN_POINT('Ctrl Pts',(6.02776633805246,3.77165962851178,9.19526363597655));
#24886=CARTESIAN_POINT('Ctrl Pts',(8.47763946304124,0.72427916270141,9.39377975338818));
#24887=CARTESIAN_POINT('Ctrl Pts',(7.24500126602242,-2.98638238306039,9.59229587079984));
#24888=CARTESIAN_POINT('Ctrl Pts',(3.45867836056103,-3.9621717494319,9.79081198821151));
#24889=CARTESIAN_POINT('Ctrl Pts',(0.586113239980029,-1.30947959617202,
9.98932810562315));
#24890=CARTESIAN_POINT('Ctrl Pts',(1.25794639972494,2.54240906231909,10.1878442230349));
#24891=CARTESIAN_POINT('Ctrl Pts',(4.85892581172318,4.06600786328675,10.3863603404465));
#24892=CARTESIAN_POINT('Ctrl Pts',(8.09134302835829,1.86603400672705,10.5848764578582));
#24893=CARTESIAN_POINT('Ctrl Pts',(7.99501184973105,-2.04281829746266,10.7833925752698));
#24894=CARTESIAN_POINT('Ctrl Pts',(4.658150536815,-4.08089646336047,10.9819086926815));
#24895=CARTESIAN_POINT('Ctrl Pts',(1.13659320614603,-2.38176727499459,11.1804248100931));
#24896=CARTESIAN_POINT('Ctrl Pts',(0.655315074027438,1.49853907779376,11.3789409275048));
#24897=CARTESIAN_POINT('Ctrl Pts',(3.6550614989726,4.00651184837438,11.5774570449165));
#24898=CARTESIAN_POINT('Ctrl Pts',(7.38872176624422,2.84539728015019,11.7759731623281));
#24899=CARTESIAN_POINT('Ctrl Pts',(8.43708082482397,-0.921477992040132,
11.9744892797398));
#24900=CARTESIAN_POINT('Ctrl Pts',(5.84007139076835,-3.84448124749012,12.1730053971514));
#24901=CARTESIAN_POINT('Ctrl Pts',(1.97598530342792,-3.24678170627628,12.3715215145631));
#24902=CARTESIAN_POINT('Ctrl Pts',(0.383479098877827,0.324258761208613,
12.5700376319747));
#24903=CARTESIAN_POINT('Ctrl Pts',(2.52093966656498,3.59834922323431,12.7685537493864));
#24904=CARTESIAN_POINT('Ctrl Pts',(6.43092127741269,3.5771399144821,12.967069866798));
#24905=CARTESIAN_POINT('Ctrl Pts',(8.53273714794332,0.280053916463419,13.1655859842097));
#24906=CARTESIAN_POINT('Ctrl Pts',(6.90158428470204,-3.27350013106212,13.3641021016213));
#24907=CARTESIAN_POINT('Ctrl Pts',(3.0312414520278,-3.82924502713605,13.562618219033));
#24908=CARTESIAN_POINT('Ctrl Pts',(0.466094994356506,-0.878240167322765,
13.7611343364446));
#24909=CARTESIAN_POINT('Ctrl Pts',(1.55525724336407,2.87704033182534,13.9596504538563));
#24910=CARTESIAN_POINT('Ctrl Pts',(5.30129412947213,3.99758202219787,14.1581665712679));
#24911=CARTESIAN_POINT('Ctrl Pts',(8.27365632956023,1.45721413871475,14.3566826886797));
#24912=CARTESIAN_POINT('Ctrl Pts',(7.75031108111198,-2.41764273385123,14.5551988060912));
#24913=CARTESIAN_POINT('Ctrl Pts',(4.21052800757405,-4.07846837919741,14.753714923503));
#24914=CARTESIAN_POINT('Ctrl Pts',(0.895973113878727,-2.00431026356939,
14.9522310409146));
#24915=CARTESIAN_POINT('Ctrl Pts',(0.842052722152676,1.9053570654116,15.1507471583263));
#24916=CARTESIAN_POINT('Ctrl Pts',(4.09814610146403,4.07013463762311,15.3492632757379));
#24917=CARTESIAN_POINT('Ctrl Pts',(7.682384872503,2.50756033086961,15.5477793931496));
#24918=CARTESIAN_POINT('Ctrl Pts',(8.31239134820293,-1.35139002803904,15.7462955105612));
#24919=CARTESIAN_POINT('Ctrl Pts',(5.41121758211169,-3.97276310543362,15.9448116279729));
#24920=CARTESIAN_POINT('Ctrl Pts',(1.63570332303896,-2.95595530083938,16.1433277453845));
#24921=CARTESIAN_POINT('Ctrl Pts',(0.443392711547191,0.767860140031627,
16.3418438627962));
#24922=CARTESIAN_POINT('Ctrl Pts',(2.92618112548781,3.7884838709103,16.5403599802078));
#24923=CARTESIAN_POINT('Ctrl Pts',(6.8103781630174,3.33968613741389,16.7388760976195));
#24924=CARTESIAN_POINT('Ctrl Pts',(8.5389100624284,-0.167532633159739,16.9373922150311));
#24925=CARTESIAN_POINT('Ctrl Pts',(6.52882019040339,-3.5213282050942,17.1359083324428));
#24926=CARTESIAN_POINT('Ctrl Pts',(2.62091061577914,-3.65035838956845,17.3344244498544));
#24927=CARTESIAN_POINT('Ctrl Pts',(0.393970590674286,-0.43645979805503,
17.5329405672661));
#24928=CARTESIAN_POINT('Ctrl Pts',(1.88738942918871,3.17714037417117,17.7314566846778));
#24929=CARTESIAN_POINT('Ctrl Pts',(5.73352256684974,3.8811758273502,17.9299728020894));
#24930=CARTESIAN_POINT('Ctrl Pts',(8.41015443739666,1.03090428563328,18.1284889195011));
#24931=CARTESIAN_POINT('Ctrl Pts',(7.46607648872073,-2.76344979098553,18.3270050369127));
#24932=CARTESIAN_POINT('Ctrl Pts',(3.76585734795025,-4.02708911541293,18.5255211543244));
#24933=CARTESIAN_POINT('Ctrl Pts',(0.698087318576006,-1.60279683129456,
18.724037271736));
#24934=CARTESIAN_POINT('Ctrl Pts',(1.07217183831651,2.28930630247911,18.9225533891477));
#24935=CARTESIAN_POINT('Ctrl Pts',(4.54553141985243,4.08490627169594,19.1210695065593));
#24936=CARTESIAN_POINT('Ctrl Pts',(7.93732942868568,2.13962678039228,19.319585623971));
#24937=CARTESIAN_POINT('Ctrl Pts',(8.14142176722837,-1.76508221626667,19.5181017413827));
#24938=CARTESIAN_POINT('Ctrl Pts',(4.97090455397163,-4.05336249490537,19.7166178587943));
#24939=CARTESIAN_POINT('Ctrl Pts',(1.3292771434127,-2.62965050343175,19.915133976206));
#24940=CARTESIAN_POINT('Ctrl Pts',(0.551472646603815,1.20224539704524,20.1136500936177));
#24941=CARTESIAN_POINT('Ctrl Pts',(3.3497896271543,3.93314783354192,20.3121662110293));
#24942=CARTESIAN_POINT('Ctrl Pts',(7.16158262229433,3.06214829760668,20.510682328441));
#24943=CARTESIAN_POINT('Ctrl Pts',(8.49608411816253,-0.613108395518473,
20.7091984458526));
#24944=CARTESIAN_POINT('Ctrl Pts',(6.13118302381429,-3.72689209317441,20.9077145632643));
#24945=CARTESIAN_POINT('Ctrl Pts',(2.23261078765349,-3.42765888460072,21.1062306806759));
#24946=CARTESIAN_POINT('Ctrl Pts',(0.370605683008962,0.0105590905653954,
21.3047467980876));
#24947=CARTESIAN_POINT('Ctrl Pts',(2.250356607504,3.43910732612115,21.5032629154992));
#24948=CARTESIAN_POINT('Ctrl Pts',(6.15042334082164,3.71818634797007,21.7017790329109));
#24949=CARTESIAN_POINT('Ctrl Pts',(8.49919910975228,0.592221314373082,21.9002951503225));
#24950=CARTESIAN_POINT('Ctrl Pts',(7.14571944818345,-3.07608926032515,22.0988112677342));
#24951=CARTESIAN_POINT('Ctrl Pts',(3.32947585071529,-3.92737479389549,22.2973273851459));
#24952=CARTESIAN_POINT('Ctrl Pts',(0.545310524977601,-1.18204713458114,
22.4958435025575));
#24953=CARTESIAN_POINT('Ctrl Pts',(1.34291119900688,2.64578051982372,22.6943596199692));
#24954=CARTESIAN_POINT('Ctrl Pts',(4.99184635260365,4.05064557959106,22.8928757373808));
#24955=CARTESIAN_POINT('Ctrl Pts',(8.15049824324278,1.74602012818506,23.0913918547925));
#24956=CARTESIAN_POINT('Ctrl Pts',(7.92621886181009,-2.15760353803636,23.2899079722041));
#24957=CARTESIAN_POINT('Ctrl Pts',(4.52442717371885,-4.08528469325705,23.4884240896158));
#24958=CARTESIAN_POINT('Ctrl Pts',(1.06036526828869,-2.27183616857484,23.6869402070274));
#24959=CARTESIAN_POINT('Ctrl Pts',(0.706458758169362,1.62230144113535,23.8854563244391));
#24960=CARTESIAN_POINT('Ctrl Pts',(3.78660979300229,4.03041197296648,24.0839724418507));
#24961=CARTESIAN_POINT('Ctrl Pts',(7.48045570332662,2.74822735016753,24.2824885592624));
#24962=CARTESIAN_POINT('Ctrl Pts',(8.40451183040988,-1.05203519730533,24.481004676674));
#24963=CARTESIAN_POINT('Ctrl Pts',(5.71394743641032,-3.88635869185298,24.6795207940858));
#24964=CARTESIAN_POINT('Ctrl Pts',(1.87003416737941,-3.16648164392546,24.8780369114974));
#24965=CARTESIAN_POINT('Ctrl Pts',(0.398188145107553,0.462946646320358,
25.076553028909));
#24966=CARTESIAN_POINT('Ctrl Pts',(1.88978798161488,2.58492499113116,25.2088971071835));
#24967=CARTESIAN_POINT('Ctrl Pts',(2.91960708544911,3.09611134481228,25.2750691463207));
#24968=CARTESIAN_POINT('Ctrl Pts',(2.58997049159961,-2.62015330925654,0.00319355095334283));
#24969=CARTESIAN_POINT('Ctrl Pts',(1.71783944528228,-1.99894889552244,0.0694097009926075));
#24970=CARTESIAN_POINT('Ctrl Pts',(0.65845605968771,0.171475772890977,0.20179789016909));
#24971=CARTESIAN_POINT('Ctrl Pts',(2.5459024084217,3.29075405988094,0.400358118482792));
#24972=CARTESIAN_POINT('Ctrl Pts',(6.18433372098768,3.38626231280436,0.598874235894448));
#24973=CARTESIAN_POINT('Ctrl Pts',(8.23950371306965,0.385416781850904,0.797390353306103));
#24974=CARTESIAN_POINT('Ctrl Pts',(6.83072086642306,-2.97082408396747,0.995906470717762));
#24975=CARTESIAN_POINT('Ctrl Pts',(3.24739392835603,-3.60517206763711,1.19442258812942));
#24976=CARTESIAN_POINT('Ctrl Pts',(0.771445147794971,-0.938633334672633,
1.39293870554108));
#24977=CARTESIAN_POINT('Ctrl Pts',(1.6701033647243,2.58783275185508,1.59145482295273));
#24978=CARTESIAN_POINT('Ctrl Pts',(5.12049770482736,3.74423103498232,1.78997094036439));
#24979=CARTESIAN_POINT('Ctrl Pts',(7.96276883664299,1.47182751406662,1.98848705777604));
#24980=CARTESIAN_POINT('Ctrl Pts',(7.59404699250464,-2.14849653622342,2.1870031751877));
#24981=CARTESIAN_POINT('Ctrl Pts',(4.35198598660702,-3.80124283382013,2.38551929259936));
#24982=CARTESIAN_POINT('Ctrl Pts',(1.20561125008781,-1.97289654529749,2.58403541001101));
#24983=CARTESIAN_POINT('Ctrl Pts',(1.0363089362513,1.66219780307218,2.78255152742267));
#24984=CARTESIAN_POINT('Ctrl Pts',(3.99912495903867,3.77507940693446,2.98106764483432));
#24985=CARTESIAN_POINT('Ctrl Pts',(7.38076768128599,2.43081698451723,3.17958376224598));
#24986=CARTESIAN_POINT('Ctrl Pts',(8.08439358796167,-1.13954237620741,3.37809987965763));
#24987=CARTESIAN_POINT('Ctrl Pts',(5.4656351638386,-3.66632999264102,3.5766159970693));
#24988=CARTESIAN_POINT('Ctrl Pts',(1.92270171311447,-2.83556261008053,3.77513211448094));
#24989=CARTESIAN_POINT('Ctrl Pts',(0.700144216203009,0.591959212043988,
3.97364823189261));
#24990=CARTESIAN_POINT('Ctrl Pts',(2.91755761499276,3.47737597536012,4.17216434930425));
#24991=CARTESIAN_POINT('Ctrl Pts',(6.54427687678886,3.1782780050441,4.37068046671592));
#24992=CARTESIAN_POINT('Ctrl Pts',(8.2590215005,-0.0314265247951463,4.56919658412757));
#24993=CARTESIAN_POINT('Ctrl Pts',(6.49146097171637,-3.21235123071783,4.76771270153922));
#24994=CARTESIAN_POINT('Ctrl Pts',(2.86029360321679,-3.45146579032245,4.96622881895089));
#24995=CARTESIAN_POINT('Ctrl Pts',(0.690873397337037,-0.529793630188544,
5.16474493636253));
#24996=CARTESIAN_POINT('Ctrl Pts',(1.96991411271267,2.8770534572674,5.36326105377419));
#24997=CARTESIAN_POINT('Ctrl Pts',(5.52609459169944,3.64914971667956,5.56177717118585));
#24998=CARTESIAN_POINT('Ctrl Pts',(8.1027323975949,1.07942407934716,5.7602932885975));
#24999=CARTESIAN_POINT('Ctrl Pts',(7.34019164048911,-2.47881759682101,5.95880940600916));
#25000=CARTESIAN_POINT('Ctrl Pts',(3.93679264073839,-3.76700527003896,6.15732552342081));
#25001=CARTESIAN_POINT('Ctrl Pts',(1.00930346276847,-1.60544117293717,6.35584164083248));
#25002=CARTESIAN_POINT('Ctrl Pts',(1.23866300903221,2.02635541158186,6.55435775824412));
#25003=CARTESIAN_POINT('Ctrl Pts',(4.41482816993367,3.80245425555658,6.75287387565579));
#25004=CARTESIAN_POINT('Ctrl Pts',(7.6291273081915,2.09633782263408,6.95138999306744));
#25005=CARTESIAN_POINT('Ctrl Pts',(7.93796641543966,-1.5295649116789,7.14990611047909));
#25006=CARTESIAN_POINT('Ctrl Pts',(5.05851651200422,-3.75472119528823,7.34842222789076));
#25007=CARTESIAN_POINT('Ctrl Pts',(1.62772304650576,-2.54137523062185,7.5469383453024));
#25008=CARTESIAN_POINT('Ctrl Pts',(0.787441414036509,0.999313828164636,
7.74545446271406));
#25009=CARTESIAN_POINT('Ctrl Pts',(3.30718554976015,3.62485029208286,7.94397058012572));
#25010=CARTESIAN_POINT('Ctrl Pts',(6.8794217047968,2.93081781047529,8.14248669753737));
#25011=CARTESIAN_POINT('Ctrl Pts',(8.23276395950072,-0.447201871899268,
8.34100281494903));
#25012=CARTESIAN_POINT('Ctrl Pts',(6.12784722031342,-3.41568258667014,8.53951893236069));
#25013=CARTESIAN_POINT('Ctrl Pts',(2.49231419722064,-3.25614616174064,8.73803504977233));
#25014=CARTESIAN_POINT('Ctrl Pts',(0.655516877599837,-0.114693020356707,
8.93655116718401));
#25015=CARTESIAN_POINT('Ctrl Pts',(2.29955930716991,3.13179380737736,9.13506728459565));
#25016=CARTESIAN_POINT('Ctrl Pts',(5.9188587019336,3.51024343935022,9.33358340200731));
#25017=CARTESIAN_POINT('Ctrl Pts',(8.19892952254092,0.674078901476532,9.53209951941897));
#25018=CARTESIAN_POINT('Ctrl Pts',(7.05172628302556,-2.77939427202906,9.73061563683061));
#25019=CARTESIAN_POINT('Ctrl Pts',(3.52783588801619,-3.68755104089551,9.92913175424228));
#25020=CARTESIAN_POINT('Ctrl Pts',(0.854370129759403,-1.21871871116838,
10.1276478716539));
#25021=CARTESIAN_POINT('Ctrl Pts',(1.47963809495571,2.36619303175871,10.3261639890656));
#25022=CARTESIAN_POINT('Ctrl Pts',(4.83103127493619,3.78419020596524,10.5246801064772));
#25023=CARTESIAN_POINT('Ctrl Pts',(7.83940754573271,1.73669797247918,10.7231962238889));
#25024=CARTESIAN_POINT('Ctrl Pts',(7.74975314393437,-1.90122922870495,10.9217123413006));
#25025=CARTESIAN_POINT('Ctrl Pts',(4.64417186530054,-3.79804686745578,11.1202284587122));
#25026=CARTESIAN_POINT('Ctrl Pts',(1.36669597038421,-2.21668543150265,11.3187445761239));
#25027=CARTESIAN_POINT('Ctrl Pts',(0.91877553954763,1.39467435679268,11.5172606935355));
#25028=CARTESIAN_POINT('Ctrl Pts',(3.71060758300086,3.72881789865659,11.7157768109472));
#25029=CARTESIAN_POINT('Ctrl Pts',(7.18548542162604,2.64818093856821,11.9142929283589));
#25030=CARTESIAN_POINT('Ctrl Pts',(8.16118202999545,-0.857609751318129,
12.1128090457705));
#25031=CARTESIAN_POINT('Ctrl Pts',(5.74417301388192,-3.57801774441457,12.3113251631822));
#25032=CARTESIAN_POINT('Ctrl Pts',(2.14790925385559,-3.02174514829049,12.5098412805938));
#25033=CARTESIAN_POINT('Ctrl Pts',(0.665780693158256,0.301784174950485,
12.7083573980055));
#25034=CARTESIAN_POINT('Ctrl Pts',(2.65509247460188,3.34894529131551,12.9068735154171));
#25035=CARTESIAN_POINT('Ctrl Pts',(6.29407070946287,3.32920601358802,13.1053896328288));
#25036=CARTESIAN_POINT('Ctrl Pts',(8.25020835096136,0.260643196829997,13.3039057502404));
#25037=CARTESIAN_POINT('Ctrl Pts',(6.7321117566965,-3.04661170162563,13.5024218676521));
#25038=CARTESIAN_POINT('Ctrl Pts',(3.1300249104368,-3.56383755643203,13.7009379850637));
#25039=CARTESIAN_POINT('Ctrl Pts',(0.742670427029733,-0.817368768436538,
13.8994541024754));
#25040=CARTESIAN_POINT('Ctrl Pts',(1.75634213008195,2.67763078969056,14.0979702198871));
#25041=CARTESIAN_POINT('Ctrl Pts',(5.24273875601857,3.7205070045574,14.2964863372987));
#25042=CARTESIAN_POINT('Ctrl Pts',(8.0090845931027,1.35621367619806,14.4950024547104));
#25043=CARTESIAN_POINT('Ctrl Pts',(7.52201274521021,-2.25007433890389,14.693518572122));
#25044=CARTESIAN_POINT('Ctrl Pts',(4.22757434555207,-3.79578707538995,14.8920346895337));
#25045=CARTESIAN_POINT('Ctrl Pts',(1.14275341367199,-1.86539021176013,15.0905508069453));
#25046=CARTESIAN_POINT('Ctrl Pts',(1.09257027946957,1.77329552431533,15.289066924357));
#25047=CARTESIAN_POINT('Ctrl Pts',(4.12298170266298,3.78803095088039,15.4875830417686));
#25048=CARTESIAN_POINT('Ctrl Pts',(7.45879454642923,2.3337596886183,15.6860991591803));
#25049=CARTESIAN_POINT('Ctrl Pts',(8.04513486233581,-1.25772430366396,15.8846152765919));
#25050=CARTESIAN_POINT('Ctrl Pts',(5.34504334245093,-3.69740830310385,16.0831313940036));
#25051=CARTESIAN_POINT('Ctrl Pts',(1.83121243949837,-2.75107611072479,16.2816475114153));
#25052=CARTESIAN_POINT('Ctrl Pts',(0.721541654250978,0.714639252839528,
16.4801636288269));
#25053=CARTESIAN_POINT('Ctrl Pts',(3.03224638366176,3.52590158253341,16.6786797462386));
#25054=CARTESIAN_POINT('Ctrl Pts',(6.64722719080097,3.10821031270302,16.8771958636502));
#25055=CARTESIAN_POINT('Ctrl Pts',(8.25595341671681,-0.155920837071448,
17.0757119810619));
#25056=CARTESIAN_POINT('Ctrl Pts',(6.38518418493321,-3.27726265018464,17.2742280984735));
#25057=CARTESIAN_POINT('Ctrl Pts',(2.74813437211341,-3.39734966840464,17.4727442158852));
#25058=CARTESIAN_POINT('Ctrl Pts',(0.675545012814546,-0.406208484742623,
17.6712603332969));
#25059=CARTESIAN_POINT('Ctrl Pts',(2.06545401745235,2.9569307023417,17.8697764507085));
#25060=CARTESIAN_POINT('Ctrl Pts',(5.64500915845253,3.61216899900811,18.0682925681202));
#25061=CARTESIAN_POINT('Ctrl Pts',(8.13612192804524,0.959451637121888,18.2668086855318));
#25062=CARTESIAN_POINT('Ctrl Pts',(7.25747863782803,-2.57191328333314,18.4653248029435));
#25063=CARTESIAN_POINT('Ctrl Pts',(3.81372409941205,-3.74796894189382,18.6638409203551));
#25064=CARTESIAN_POINT('Ctrl Pts',(0.958583211925542,-1.49170593738941,
18.8623570377668));
#25065=CARTESIAN_POINT('Ctrl Pts',(1.306739689582,2.13063298930591,19.0608731551785));
#25066=CARTESIAN_POINT('Ctrl Pts',(4.53935845279781,3.80177875335989,19.2593892725901));
#25067=CARTESIAN_POINT('Ctrl Pts',(7.69606872911877,1.99132785253305,19.4579053900018));
#25068=CARTESIAN_POINT('Ctrl Pts',(7.88601529454458,-1.64274321646801,19.6564215074134));
#25069=CARTESIAN_POINT('Ctrl Pts',(4.93524869751396,-3.77242129631514,19.8549376248251));
#25070=CARTESIAN_POINT('Ctrl Pts',(1.54602485826833,-2.44738771167893,20.0534537422367));
#25071=CARTESIAN_POINT('Ctrl Pts',(0.822130498506685,1.11891698433359,20.2519698596484));
#25072=CARTESIAN_POINT('Ctrl Pts',(3.42649430375165,3.66053879154859,20.45048597706));
#25073=CARTESIAN_POINT('Ctrl Pts',(6.97408943990954,2.84990880161489,20.6490020944717));
#25074=CARTESIAN_POINT('Ctrl Pts',(8.21609576658401,-0.570613452685432,
20.8475182118833));
#25075=CARTESIAN_POINT('Ctrl Pts',(6.015107509745,-3.46857877108964,21.046034329295));
#25076=CARTESIAN_POINT('Ctrl Pts',(2.38674785836889,-3.19008561139642,21.2445504467067));
#25077=CARTESIAN_POINT('Ctrl Pts',(0.653799542140776,0.00982723311048271,
21.4430665641183));
#25078=CARTESIAN_POINT('Ctrl Pts',(2.40326370386975,3.2007405539671,21.64158268153));
#25079=CARTESIAN_POINT('Ctrl Pts',(6.03301426782987,3.46047642676426,21.8400987989417));
#25080=CARTESIAN_POINT('Ctrl Pts',(8.21899485607472,0.551174068759129,22.0386149163533));
#25081=CARTESIAN_POINT('Ctrl Pts',(6.95932575274402,-2.86288350711349,22.2371310337649));
#25082=CARTESIAN_POINT('Ctrl Pts',(3.40758848840856,-3.65516588504588,22.4356471511766));
#25083=CARTESIAN_POINT('Ctrl Pts',(0.816395477550012,-1.10011867661645,
22.6341632685882));
#25084=CARTESIAN_POINT('Ctrl Pts',(1.55871392857562,2.46239974611297,22.8326793859999));
#25085=CARTESIAN_POINT('Ctrl Pts',(4.95473900642221,3.76989269217354,23.0311955034116));
#25086=CARTESIAN_POINT('Ctrl Pts',(7.89446267408575,1.62500233414576,23.2297116208232));
#25087=CARTESIAN_POINT('Ctrl Pts',(7.68572824288089,-2.00805862937836,23.4282277382349));
#25088=CARTESIAN_POINT('Ctrl Pts',(4.5197169557303,-3.80213094627573,23.6267438556465));
#25089=CARTESIAN_POINT('Ctrl Pts',(1.29575144062437,-2.11437372177854,23.8252599730582));
#25090=CARTESIAN_POINT('Ctrl Pts',(0.966374421579891,1.50985866999905,24.0237760904698));
#25091=CARTESIAN_POINT('Ctrl Pts',(3.83303817896047,3.7510614900228,24.2222922078815));
#25092=CARTESIAN_POINT('Ctrl Pts',(7.27086121968984,2.55774591981802,24.4208083252931));
#25093=CARTESIAN_POINT('Ctrl Pts',(8.13087041382945,-0.979117951521988,
24.6193244427048));
#25094=CARTESIAN_POINT('Ctrl Pts',(5.62679079307294,-3.61699263579137,24.8178405601165));
#25095=CARTESIAN_POINT('Ctrl Pts',(2.04930166016011,-2.94701073564213,25.0163566775281));
#25096=CARTESIAN_POINT('Ctrl Pts',(0.679470245798868,0.430859512276974,
25.2148727949398));
#25097=CARTESIAN_POINT('Ctrl Pts',(2.06768632464525,2.40576215381105,25.3472168732142));
#25098=CARTESIAN_POINT('Ctrl Pts',(3.02612799462649,2.8815178478641,25.4133889123514));
#25099=CARTESIAN_POINT('Origin',(4.45646910621825,5.55111512312578E-15,
25.));
#25100=CARTESIAN_POINT('',(0.,0.,0.));
#25101=CARTESIAN_POINT('Origin',(4.45646910621825,2.93978508838399E-15,
8.23961502859548));
#25102=CARTESIAN_POINT('',(7.69556181015728,2.48510987823924,11.2345514513157));
#25103=CARTESIAN_POINT('',(7.69439310869886,2.48413784397184,11.129953879674));
#25104=CARTESIAN_POINT('',(7.69749241145744,2.48656247355586,8.23961502859548));
#25105=CARTESIAN_POINT('',(3.39564331816006,3.95074861019264,11.));
#25106=CARTESIAN_POINT('Ctrl Pts',(3.39564331816006,3.95074861019264,11.));
#25107=CARTESIAN_POINT('Ctrl Pts',(4.5655900814632,4.25812260114716,11.0591063170672));
#25108=CARTESIAN_POINT('Ctrl Pts',(6.31389358558768,3.94134188869289,11.1372901341725));
#25109=CARTESIAN_POINT('Ctrl Pts',(7.45937911124849,2.79816356646418,11.2154739512777));
#25110=CARTESIAN_POINT('Ctrl Pts',(7.69556181015739,2.48510987823911,11.2345514513157));
#25111=CARTESIAN_POINT('',(5.51437352919123,3.94563850749837,11.));
#25112=CARTESIAN_POINT('Origin',(4.45646910621825,3.5527136788005E-15,11.));
#25113=CARTESIAN_POINT('Ctrl Pts',(5.5143735291912,3.94563850749838,11.));
#25114=CARTESIAN_POINT('Ctrl Pts',(6.37349612905838,3.71529059383414,11.0433179598914));
#25115=CARTESIAN_POINT('Ctrl Pts',(7.14733598556437,3.18456765028079,11.0866359197827));
#25116=CARTESIAN_POINT('Ctrl Pts',(7.69439310869878,2.48413784397194,11.129953879674));
#25117=CARTESIAN_POINT('Origin',(4.45646910621825,2.93978508838399E-15,
8.23961502859548));
#25118=CARTESIAN_POINT('',(7.69775011106544,2.48676061171584,12.4842647253843));
#25119=CARTESIAN_POINT('',(7.69749241145744,2.48656247355586,12.3802773657823));
#25120=CARTESIAN_POINT('',(7.69749241145744,2.48656247355586,8.23961502859548));
#25121=CARTESIAN_POINT('',(8.54727164081007,-0.00047517376629813,11.3646150285955));
#25122=CARTESIAN_POINT('Ctrl Pts',(8.54727164081007,-0.000475173766298197,
11.3646150285955));
#25123=CARTESIAN_POINT('Ctrl Pts',(8.54735745749987,-0.0387234396568994,
11.3664854167815));
#25124=CARTESIAN_POINT('Ctrl Pts',(8.52991518830434,-1.39184926051541,11.4326582189516));
#25125=CARTESIAN_POINT('Ctrl Pts',(7.04969563431661,-4.0201072215765,11.5631334351056));
#25126=CARTESIAN_POINT('Ctrl Pts',(2.60806863526002,-4.41194201582685,11.7560406770575));
#25127=CARTESIAN_POINT('Ctrl Pts',(-0.227582196371091,-0.971141764274265,
11.9489479190094));
#25128=CARTESIAN_POINT('Ctrl Pts',(1.00642988914386,3.31373500369963,12.1418551609614));
#25129=CARTESIAN_POINT('Ctrl Pts',(4.92059444400304,4.61393675418963,12.3202940964197));
#25130=CARTESIAN_POINT('Ctrl Pts',(7.06770587424214,3.29253755255905,12.434430617894));
#25131=CARTESIAN_POINT('Ctrl Pts',(7.69775011106531,2.486760611716,12.4842647253843));
#25132=CARTESIAN_POINT('Ctrl Pts',(7.69556181015739,2.48510987823911,11.2345514513157));
#25133=CARTESIAN_POINT('Ctrl Pts',(8.23229822129631,1.77368048951597,11.2779059770756));
#25134=CARTESIAN_POINT('Ctrl Pts',(8.54528245914361,0.886097699817623,11.3212605028356));
#25135=CARTESIAN_POINT('Ctrl Pts',(8.54727164081007,-0.000475173766298063,
11.3646150285955));
#25136=CARTESIAN_POINT('',(8.54040281351477,0.00367837158999622,11.2603846386009));
#25137=CARTESIAN_POINT('Ctrl Pts',(7.69439310869878,2.48413784397194,11.129953879674));
#25138=CARTESIAN_POINT('Ctrl Pts',(7.95940316723485,2.14482968743651,11.1509383337667));
#25139=CARTESIAN_POINT('Ctrl Pts',(8.39820086233578,1.3593237731873,11.1944148818445));
#25140=CARTESIAN_POINT('Ctrl Pts',(8.53950282154932,0.466629832326752,11.2378914299223));
#25141=CARTESIAN_POINT('Ctrl Pts',(8.53683689913243,0.00369810825016921,
11.2603835239075));
#25142=CARTESIAN_POINT('Ctrl Pts',(8.54146745540981,0.00367247899891429,
11.2603849714045));
#25143=CARTESIAN_POINT('Ctrl Pts',(8.54157476677189,-0.115692869881448,
11.2661779401166));
#25144=CARTESIAN_POINT('Ctrl Pts',(8.53644591819133,-0.235111513907259,
11.2719709088288));
#25145=CARTESIAN_POINT('Ctrl Pts',(8.52609375567047,-0.354090684105999,
11.2777638775409));
#25146=CARTESIAN_POINT('Ctrl Pts',(8.51574265793688,-0.473057616522975,
11.2835562504085));
#25147=CARTESIAN_POINT('Ctrl Pts',(8.50016935000466,-0.591584757457358,
11.2893486232761));
#25148=CARTESIAN_POINT('Ctrl Pts',(8.47943865605452,-0.709183333905947,
11.2951409961437));
#25149=CARTESIAN_POINT('Ctrl Pts',(8.45870517893015,-0.82679769840907,11.3009341466594));
#25150=CARTESIAN_POINT('Ctrl Pts',(8.43281300991758,-0.943482847585876,
11.306727297175));
#25151=CARTESIAN_POINT('Ctrl Pts',(8.401878187897,-1.0587597358261,11.3125204476906));
#25152=CARTESIAN_POINT('Ctrl Pts',(8.37093187778747,-1.17407943378888,11.3183157495756));
#25153=CARTESIAN_POINT('Ctrl Pts',(8.33493929621817,-1.28798943581637,11.3241110514606));
#25154=CARTESIAN_POINT('Ctrl Pts',(8.29406628598849,-1.40002603040773,11.3299063533456));
#25155=CARTESIAN_POINT('Ctrl Pts',(8.25314563799088,-1.51219320440253,11.3357084096938));
#25156=CARTESIAN_POINT('Ctrl Pts',(8.20733334848537,-1.62248222845368,11.3415104660421));
#25157=CARTESIAN_POINT('Ctrl Pts',(8.15684339460683,-1.73044939996305,11.3473125223903));
#25158=CARTESIAN_POINT('Ctrl Pts',(8.10631811955717,-1.83849210188286,11.3531186376733));
#25159=CARTESIAN_POINT('Ctrl Pts',(8.05110885291911,-1.94420935528272,11.3589247529562));
#25160=CARTESIAN_POINT('Ctrl Pts',(7.99147467780075,-2.04718357967243,11.3647308682392));
#25161=CARTESIAN_POINT('Ctrl Pts',(7.93175327035386,-2.15030843382024,11.3705454766547));
#25162=CARTESIAN_POINT('Ctrl Pts',(7.86759425665247,-2.25068190833779,11.3763600850702));
#25163=CARTESIAN_POINT('Ctrl Pts',(7.79929905286146,-2.34791672506183,11.3821746934858));
#25164=CARTESIAN_POINT('Ctrl Pts',(7.78504872503205,-2.36820552922135,11.3833879569585));
#25165=CARTESIAN_POINT('Ctrl Pts',(7.7706184501971,-2.3883578030232,11.3846012204312));
#25166=CARTESIAN_POINT('Ctrl Pts',(7.75601117534001,-2.40837022363578,11.3858144839039));
#25167=CARTESIAN_POINT('Ctrl Pts',(7.68563116797709,-2.5047930214432,11.3916601664818));
#25168=CARTESIAN_POINT('Ctrl Pts',(7.61091634050207,-2.59827161053316,11.3975058490597));
#25169=CARTESIAN_POINT('Ctrl Pts',(7.53214114961318,-2.68839477783279,11.4033515316375));
#25170=CARTESIAN_POINT('Ctrl Pts',(7.45346095414875,-2.77840926512243,11.4091901648755));
#25171=CARTESIAN_POINT('Ctrl Pts',(7.37073040048886,-2.86507607822447,11.4150287981135));
#25172=CARTESIAN_POINT('Ctrl Pts',(7.28426616769128,-2.94801437905656,11.4208674313514));
#25173=CARTESIAN_POINT('Ctrl Pts',(7.19788420965286,-3.03087376021857,11.426700508857));
#25174=CARTESIAN_POINT('Ctrl Pts',(7.10777593234305,-3.11001141007274,11.4325335863625));
#25175=CARTESIAN_POINT('Ctrl Pts',(7.01429670284446,-3.18508131543562,11.438366663868));
#25176=CARTESIAN_POINT('Ctrl Pts',(6.92057628511734,-3.2603449106437,11.4442147914508));
#25177=CARTESIAN_POINT('Ctrl Pts',(6.82346777502968,-3.33151944144697,11.4500629190336));
#25178=CARTESIAN_POINT('Ctrl Pts',(6.72336512514716,-3.3982947840592,11.4559110466165));
#25179=CARTESIAN_POINT('Ctrl Pts',(6.62362386471074,-3.46482905509033,11.4617380613557));
#25180=CARTESIAN_POINT('Ctrl Pts',(6.52091038708962,-3.52699562482708,11.467565076095));
#25181=CARTESIAN_POINT('Ctrl Pts',(6.41564521302468,-3.58452981331144,11.4733920908342));
#25182=CARTESIAN_POINT('Ctrl Pts',(6.31039381885568,-3.64205647019631,11.4792183427794));
#25183=CARTESIAN_POINT('Ctrl Pts',(6.20259174768293,-3.69495175831188,11.4850445947245));
#25184=CARTESIAN_POINT('Ctrl Pts',(6.09268504542169,-3.7429964467384,11.4908708466696));
#25185=CARTESIAN_POINT('Ctrl Pts',(5.9827674125012,-3.79104591340053,11.4966976780587));
#25186=CARTESIAN_POINT('Ctrl Pts',(5.87074510297772,-3.83424365919276,11.5025245094478));
#25187=CARTESIAN_POINT('Ctrl Pts',(5.75708455421943,-3.87241842475996,11.5083513408369));
#25188=CARTESIAN_POINT('Ctrl Pts',(5.64269510245319,-3.91083800439637,11.5142155395885));
#25189=CARTESIAN_POINT('Ctrl Pts',(5.52664671484859,-3.94416980886718,11.52007973834));
#25190=CARTESIAN_POINT('Ctrl Pts',(5.40942970654366,-3.97229040909991,11.5259439370916));
#25191=CARTESIAN_POINT('Ctrl Pts',(5.29279910486616,-4.00027032918237,11.5317787987609));
#25192=CARTESIAN_POINT('Ctrl Pts',(5.17501195806892,-4.02309104079298,11.5376136604303));
#25193=CARTESIAN_POINT('Ctrl Pts',(5.05655990529035,-4.04068261966573,11.5434485220996));
#25194=CARTESIAN_POINT('Ctrl Pts',(4.93721450546845,-4.05840687150282,11.5493273893923));
#25195=CARTESIAN_POINT('Ctrl Pts',(4.81719454464012,-4.07082274578235,11.555206256685));
#25196=CARTESIAN_POINT('Ctrl Pts',(4.6970054840309,-4.0779121190811,11.5610851239777));
#25197=CARTESIAN_POINT('Ctrl Pts',(4.57681642342169,-4.08500149237984,11.5669639912704));
#25198=CARTESIAN_POINT('Ctrl Pts',(4.45645867845014,-4.08676441141684,11.5728428585631));
#25199=CARTESIAN_POINT('Ctrl Pts',(4.33643407615524,-4.08323604406572,11.5787217258558));
#25200=CARTESIAN_POINT('Ctrl Pts',(4.21705838925101,-4.07972675290261,11.584568808936));
#25201=CARTESIAN_POINT('Ctrl Pts',(4.09766291769109,-4.07097301841782,11.5904158920162));
#25202=CARTESIAN_POINT('Ctrl Pts',(3.9787423507795,-4.05696957680702,11.5962629750963));
#25203=CARTESIAN_POINT('Ctrl Pts',(3.85996204158473,-4.04298265118499,11.6021031619891));
#25204=CARTESIAN_POINT('Ctrl Pts',(3.74165592123341,-4.02375838344357,11.6079433488818));
#25205=CARTESIAN_POINT('Ctrl Pts',(3.62431738646312,-3.99934351054124,11.6137835357745));
#25206=CARTESIAN_POINT('Ctrl Pts',(3.5070874522047,-3.97495123437321,11.6196183173902));
#25207=CARTESIAN_POINT('Ctrl Pts',(3.39082371543823,-3.94537799450139,11.6254530990059));
#25208=CARTESIAN_POINT('Ctrl Pts',(3.27601261611103,-3.91072211681723,11.6312878806216));
#25209=CARTESIAN_POINT('Ctrl Pts',(3.16095036555719,-3.87599042881298,11.637135425921));
#25210=CARTESIAN_POINT('Ctrl Pts',(3.04734751891907,-3.83615390439813,11.6429829712204));
#25211=CARTESIAN_POINT('Ctrl Pts',(2.93568203361168,-3.79136277343549,11.6488305165199));
#25212=CARTESIAN_POINT('Ctrl Pts',(2.82436919903747,-3.74671309732912,11.6546595946884));
#25213=CARTESIAN_POINT('Ctrl Pts',(2.71498188359263,-3.6971402155858,11.6604886728568));
#25214=CARTESIAN_POINT('Ctrl Pts',(2.6079761081951,-3.64284210970763,11.6663177510253));
#25215=CARTESIAN_POINT('Ctrl Pts',(2.5009819057502,-3.58854987631068,11.6721461987639));
#25216=CARTESIAN_POINT('Ctrl Pts',(2.39636909137021,-3.52953361839601,11.6779746465024));
#25217=CARTESIAN_POINT('Ctrl Pts',(2.29457054318916,-3.46603802679262,11.683803094241));
#25218=CARTESIAN_POINT('Ctrl Pts',(2.19275959622875,-3.40253470160319,11.6896322518682));
#25219=CARTESIAN_POINT('Ctrl Pts',(2.09376394011757,-3.33455117173568,11.6954614094954));
#25220=CARTESIAN_POINT('Ctrl Pts',(1.99798833561155,-3.26237602071815,11.7012905671227));
#25221=CARTESIAN_POINT('Ctrl Pts',(1.90168078318288,-3.18980000121383,11.7071521005131));
#25222=CARTESIAN_POINT('Ctrl Pts',(1.8086294954468,-3.11298589896686,11.7130136339035));
#25223=CARTESIAN_POINT('Ctrl Pts',(1.7192122295977,-3.03226809358824,11.7188751672939));
#25224=CARTESIAN_POINT('Ctrl Pts',(1.63016174687966,-2.95188138678558,11.7247126571));
#25225=CARTESIAN_POINT('Ctrl Pts',(1.54471578341265,-2.86762326311697,11.7305501469062));
#25226=CARTESIAN_POINT('Ctrl Pts',(1.46320967827899,-2.77986024775571,11.7363876367123));
#25227=CARTESIAN_POINT('Ctrl Pts',(1.38120000937685,-2.69155501197212,11.7422611918948));
#25228=CARTESIAN_POINT('Ctrl Pts',(1.30317931297184,-2.59970174770958,11.7481347470774));
#25229=CARTESIAN_POINT('Ctrl Pts',(1.22944675547593,-2.50470592042444,11.75400830226));
#25230=CARTESIAN_POINT('Ctrl Pts',(1.15571419798002,-2.40971009313931,11.7598818574426));
#25231=CARTESIAN_POINT('Ctrl Pts',(1.08626997328914,-2.3115720696642,11.7657554126251));
#25232=CARTESIAN_POINT('Ctrl Pts',(1.02136744071989,-2.21072421339481,11.7716289678077));
#25233=CARTESIAN_POINT('Ctrl Pts',(0.956917641603606,-2.11057983041662,
11.7774615514779));
#25234=CARTESIAN_POINT('Ctrl Pts',(0.896751387672808,-2.00746031269782,
11.783294135148));
#25235=CARTESIAN_POINT('Ctrl Pts',(0.841153576985724,-1.90176723709551,
11.7891267188182));
#25236=CARTESIAN_POINT('Ctrl Pts',(0.785623809914929,-1.7962035144118,11.7949521642561));
#25237=CARTESIAN_POINT('Ctrl Pts',(0.734651552095715,-1.68807285619862,
11.800777609694));
#25238=CARTESIAN_POINT('Ctrl Pts',(0.688478265853558,-1.57780544647543,
11.8066030551319));
#25239=CARTESIAN_POINT('Ctrl Pts',(0.642349573470072,-1.46764453229729,
11.8124228743926));
#25240=CARTESIAN_POINT('Ctrl Pts',(0.601010787499888,-1.35535134568636,
11.8182426936533));
#25241=CARTESIAN_POINT('Ctrl Pts',(0.564657024109714,-1.24137976363148,
11.824062512914));
#25242=CARTESIAN_POINT('Ctrl Pts',(0.528095554092989,-1.12675700682539,
11.8299155836159));
#25243=CARTESIAN_POINT('Ctrl Pts',(0.496576444740284,-1.01043698359192,
11.8357686543178));
#25244=CARTESIAN_POINT('Ctrl Pts',(0.470248801469663,-0.892901272263529,
11.8416217250197));
#25245=CARTESIAN_POINT('Ctrl Pts',(0.444098362661862,-0.776156662986079,
11.8474354002376));
#25246=CARTESIAN_POINT('Ctrl Pts',(0.423069797110182,-0.658213085408489,
11.8532490754555));
#25247=CARTESIAN_POINT('Ctrl Pts',(0.407258794977066,-0.539556165137435,
11.8590627506734));
#25248=CARTESIAN_POINT('Ctrl Pts',(0.391449880829969,-0.420914914587281,
11.8648756581428));
#25249=CARTESIAN_POINT('Ctrl Pts',(0.380857213193959,-0.301560911811138,
11.8706885656122));
#25250=CARTESIAN_POINT('Ctrl Pts',(0.375524898252689,-0.181987283819745,
11.8765014730816));
#25251=CARTESIAN_POINT('Ctrl Pts',(0.370192041379855,-0.0624015033722743,
11.882314971326));
#25252=CARTESIAN_POINT('Ctrl Pts',(0.37012061818985,0.0574035403353615,
11.8881284695704));
#25253=CARTESIAN_POINT('Ctrl Pts',(0.375302639045832,0.176932945567398,
11.8939419678147));
#25254=CARTESIAN_POINT('Ctrl Pts',(0.380546481604044,0.297888341065266,
11.8998248213101));
#25255=CARTESIAN_POINT('Ctrl Pts',(0.391169927108912,0.418561051469162,
11.9057076748055));
#25256=CARTESIAN_POINT('Ctrl Pts',(0.407110612018016,0.538442926825278,
11.9115905283009));
#25257=CARTESIAN_POINT('Ctrl Pts',(0.422885536900894,0.65707820437732,11.9174122086438));
#25258=CARTESIAN_POINT('Ctrl Pts',(0.443867509038086,0.774938623117823,
11.9232338889867));
#25259=CARTESIAN_POINT('Ctrl Pts',(0.469944651035495,0.891542353581472,
11.9290555693295));
#25260=CARTESIAN_POINT('Ctrl Pts',(0.496432813792764,1.00998396006323,11.9349690094012));
#25261=CARTESIAN_POINT('Ctrl Pts',(0.528178014589218,1.12712850324347,11.9408824494729));
#25262=CARTESIAN_POINT('Ctrl Pts',(0.565010824631404,1.24248840745856,11.9467958895446));
#25263=CARTESIAN_POINT('Ctrl Pts',(0.60184363467359,1.35784831167365,11.9527093296163));
#25264=CARTESIAN_POINT('Ctrl Pts',(0.643763850064308,1.47142318964377,11.9586227696879));
#25265=CARTESIAN_POINT('Ctrl Pts',(0.690552128350566,1.58274897435054,11.9645362097596));
#25266=CARTESIAN_POINT('Ctrl Pts',(0.736762100003609,1.69269876399826,11.9703765592679));
#25267=CARTESIAN_POINT('Ctrl Pts',(0.78786060021798,1.80078831191609,11.9762169087763));
#25268=CARTESIAN_POINT('Ctrl Pts',(0.843676036575304,1.90655480800833,11.9820572582846));
#25269=CARTESIAN_POINT('Ctrl Pts',(0.899424151962499,2.01219373539217,11.987890563541));
#25270=CARTESIAN_POINT('Ctrl Pts',(0.959877697870534,2.11551482912866,11.9937238687974));
#25271=CARTESIAN_POINT('Ctrl Pts',(1.02481697593313,2.21607505665069,11.9995571740538));
#25272=CARTESIAN_POINT('Ctrl Pts',(1.08969454519933,2.31653972643338,12.0053849361897));
#25273=CARTESIAN_POINT('Ctrl Pts',(1.15904914634169,2.41424841125923,12.0112126983255));
#25274=CARTESIAN_POINT('Ctrl Pts',(1.23261538883901,2.50878301352266,12.0170404604614));
#25275=CARTESIAN_POINT('Ctrl Pts',(1.30646392238179,2.60368036737973,12.0228905850968));
#25276=CARTESIAN_POINT('Ctrl Pts',(1.38455628918227,2.69537886602613,12.0287407097322));
#25277=CARTESIAN_POINT('Ctrl Pts',(1.4665800744481,2.78348496990739,12.0345908343676));
#25278=CARTESIAN_POINT('Ctrl Pts',(1.54820628545173,2.8711640181592,12.0404126030941));
#25279=CARTESIAN_POINT('Ctrl Pts',(1.6337256032797,2.95528512548764,12.0462343718206));
#25280=CARTESIAN_POINT('Ctrl Pts',(1.72279041348928,3.03549432628681,12.0520561405471));
#25281=CARTESIAN_POINT('Ctrl Pts',(1.81184411660245,3.11569352435511,12.0578771832523));
#25282=CARTESIAN_POINT('Ctrl Pts',(1.90444213129456,3.19198151514502,12.0636982259575));
#25283=CARTESIAN_POINT('Ctrl Pts',(2.00020153116519,3.26404267737766,12.0695192686628));
#25284=CARTESIAN_POINT('Ctrl Pts',(2.09597117978909,3.33611155203407,12.0753409343714));
#25285=CARTESIAN_POINT('Ctrl Pts',(2.19490256238751,3.4039524548848,12.08116260008));
#25286=CARTESIAN_POINT('Ctrl Pts',(2.29658186477975,3.46729175355507,12.0869842657886));
#25287=CARTESIAN_POINT('Ctrl Pts',(2.39913328262664,3.53117432091382,12.0928558646155));
#25288=CARTESIAN_POINT('Ctrl Pts',(2.50447963195213,3.59047746520519,12.0987274634424));
#25289=CARTESIAN_POINT('Ctrl Pts',(2.61216996471223,3.64496717085901,12.1045990622693));
#25290=CARTESIAN_POINT('Ctrl Pts',(2.71909463828269,3.69906946435795,12.1104289150687));
#25291=CARTESIAN_POINT('Ctrl Pts',(2.82832967587111,3.74842642925111,12.116258767868));
#25292=CARTESIAN_POINT('Ctrl Pts',(2.93941339388369,3.79285736163026,12.1220886206674));
#25293=CARTESIAN_POINT('Ctrl Pts',(3.05169027339974,3.83776553116915,12.1279810925081));
#25294=CARTESIAN_POINT('Ctrl Pts',(3.16585537848582,3.87764108359278,12.1338735643488));
#25295=CARTESIAN_POINT('Ctrl Pts',(3.28141705662326,3.91234938122126,12.1397660361895));
#25296=CARTESIAN_POINT('Ctrl Pts',(3.39697873476069,3.94705767884974,12.1456585080302));
#25297=CARTESIAN_POINT('Ctrl Pts',(3.51393656328173,3.97659867159665,12.1515509798709));
#25298=CARTESIAN_POINT('Ctrl Pts',(3.63179014717668,4.00089110255627,12.1574434517116));
#25299=CARTESIAN_POINT('Ctrl Pts',(3.74858646128753,4.0249656050288,12.1632830619232));
#25300=CARTESIAN_POINT('Ctrl Pts',(3.86661337411199,4.04395768876275,12.1691226721349));
#25301=CARTESIAN_POINT('Ctrl Pts',(3.9853922655829,4.05774711018526,12.1749622823466));
#25302=CARTESIAN_POINT('Ctrl Pts',(4.10402801852705,4.07151991419836,12.1807948553382));
#25303=CARTESIAN_POINT('Ctrl Pts',(4.22341354767919,4.0801024818754,12.1866274283297));
#25304=CARTESIAN_POINT('Ctrl Pts',(4.34305933324282,4.08342542767631,12.1924600013213));
#25305=CARTESIAN_POINT('Ctrl Pts',(4.46259157484755,4.08674521999865,12.1982870391958));
#25306=CARTESIAN_POINT('Ctrl Pts',(4.58238317807265,4.08481531076132,12.2041140770704));
#25307=CARTESIAN_POINT('Ctrl Pts',(4.70193934339502,4.07761809916772,12.2099411149449));
#25308=CARTESIAN_POINT('Ctrl Pts',(4.82197482259569,4.07039203315751,12.2157915140582));
#25309=CARTESIAN_POINT('Ctrl Pts',(4.941772560987,4.05785629549922,12.2216419131714));
#25310=CARTESIAN_POINT('Ctrl Pts',(5.06083116304306,4.04004597798964,12.2274923122847));
#25311=CARTESIAN_POINT('Ctrl Pts',(5.17929288770721,4.0223249490798,12.2333133815478));
#25312=CARTESIAN_POINT('Ctrl Pts',(5.29702246650312,3.99938217433906,12.2391344508108));
#25313=CARTESIAN_POINT('Ctrl Pts',(5.41353148792556,3.97130414316513,12.2449555200739));
#25314=CARTESIAN_POINT('Ctrl Pts',(5.53002619308032,3.9432295621327,12.250775874062));
#25315=CARTESIAN_POINT('Ctrl Pts',(5.64530024504123,3.91002107494793,12.2565962280501));
#25316=CARTESIAN_POINT('Ctrl Pts',(5.75887688775485,3.87181597839989,12.2624165820382));
#25317=CARTESIAN_POINT('Ctrl Pts',(5.87246591477913,3.8336067159972,12.2682375706733));
#25318=CARTESIAN_POINT('Ctrl Pts',(5.9843567801658,3.79039989023818,12.2740585593084));
#25319=CARTESIAN_POINT('Ctrl Pts',(6.09408989255814,3.74238201686403,12.2798795479434));
#25320=CARTESIAN_POINT('Ctrl Pts',(6.20479586019967,3.69393843388274,12.2857521434201));
#25321=CARTESIAN_POINT('Ctrl Pts',(6.31330523837912,3.64059823779966,12.2916247388968));
#25322=CARTESIAN_POINT('Ctrl Pts',(6.41916973806856,3.58260118206509,12.2974973343735));
#25323=CARTESIAN_POINT('Ctrl Pts',(6.52425214971013,3.52503258728045,12.3033265452713));
#25324=CARTESIAN_POINT('Ctrl Pts',(6.62672831222032,3.46287597121902,12.3091557561691));
#25325=CARTESIAN_POINT('Ctrl Pts',(6.72618822050804,3.3964098901969,12.314984967067));
#25326=CARTESIAN_POINT('Ctrl Pts',(6.82675849166665,3.32920178688851,12.3208792548331));
#25327=CARTESIAN_POINT('Ctrl Pts',(6.92424440711328,3.25758766316226,12.3267735425991));
#25328=CARTESIAN_POINT('Ctrl Pts',(7.01825653981374,3.1818972555807,12.3326678303652));
#25329=CARTESIAN_POINT('Ctrl Pts',(7.11226867251421,3.10620684799914,12.3385621181313));
#25330=CARTESIAN_POINT('Ctrl Pts',(7.20280674160711,3.02644047770949,12.3444564058974));
#25331=CARTESIAN_POINT('Ctrl Pts',(7.28952047817893,2.94296532834342,12.3503506936635));
#25332=CARTESIAN_POINT('Ctrl Pts',(7.37417408452558,2.86147336739775,12.356104945942));
#25333=CARTESIAN_POINT('Ctrl Pts',(7.45545512726984,2.77618466306006,12.3618591982205));
#25334=CARTESIAN_POINT('Ctrl Pts',(7.53299895384682,2.6874130863435,12.3676134504989));
#25335=CARTESIAN_POINT('Ctrl Pts',(7.58988491127993,2.62229047946061,12.3718347555934));
#25336=CARTESIAN_POINT('Ctrl Pts',(7.64476020971441,2.55529442644394,12.3760560606879));
#25337=CARTESIAN_POINT('Ctrl Pts',(7.69749241145744,2.48656247355586,12.3802773657823));
#25338=CARTESIAN_POINT('Origin',(4.45646910621825,2.93978508838399E-15,
8.23961502859548));
#25339=CARTESIAN_POINT('',(7.69749241145743,2.48656247355587,13.7345026286438));
#25340=CARTESIAN_POINT('',(7.69749241145744,2.48656247355586,13.6301247167396));
#25341=CARTESIAN_POINT('',(7.69749241145744,2.48656247355586,8.23961502859548));
#25342=CARTESIAN_POINT('',(8.53966035999323,0.000944551248266404,12.6146148317601));
#25343=CARTESIAN_POINT('Ctrl Pts',(8.54146899785629,0.000940912841063322,
12.6146150285955));
#25344=CARTESIAN_POINT('Ctrl Pts',(8.54149739908273,-0.122363820490929,
12.6205921772503));
#25345=CARTESIAN_POINT('Ctrl Pts',(8.53593857126231,-0.245616423183125,
12.6265693259052));
#25346=CARTESIAN_POINT('Ctrl Pts',(8.52483281598515,-0.368295703275901,
12.63254647456));
#25347=CARTESIAN_POINT('Ctrl Pts',(8.51371936793932,-0.491059961229144,
12.6385277634846));
#25348=CARTESIAN_POINT('Ctrl Pts',(8.497051368911,-0.613249733963977,12.6445090524091));
#25349=CARTESIAN_POINT('Ctrl Pts',(8.47492076633568,-0.734350907468087,
12.6504903413336));
#25350=CARTESIAN_POINT('Ctrl Pts',(8.45275362077154,-0.855652048361935,
12.6564815068159));
#25351=CARTESIAN_POINT('Ctrl Pts',(8.42510591433828,-0.975860630413129,
12.6624726722982));
#25352=CARTESIAN_POINT('Ctrl Pts',(8.39212056454292,-1.09447366281089,12.6684638377805));
#25353=CARTESIAN_POINT('Ctrl Pts',(8.35910742797959,-1.21318661450097,12.6744600502041));
#25354=CARTESIAN_POINT('Ctrl Pts',(8.32074779667736,-1.33030098168081,12.6804562626277));
#25355=CARTESIAN_POINT('Ctrl Pts',(8.27723367032645,-1.44533150026379,12.6864524750513));
#25356=CARTESIAN_POINT('Ctrl Pts',(8.23363451074585,-1.56058680599821,12.6924604049872));
#25357=CARTESIAN_POINT('Ctrl Pts',(8.18486086695445,-1.6737497790333,12.698468334923));
#25358=CARTESIAN_POINT('Ctrl Pts',(8.13115235600658,-1.78435647047467,12.7044762648589));
#25359=CARTESIAN_POINT('Ctrl Pts',(8.08317463101388,-1.88316124704867,12.709843138845));
#25360=CARTESIAN_POINT('Ctrl Pts',(8.03125970788008,-1.97992633993934,12.7152100128311));
#25361=CARTESIAN_POINT('Ctrl Pts',(7.97560775666991,-2.07434041538437,12.7205768868172));
#25362=CARTESIAN_POINT('Ctrl Pts',(7.91506111829492,-2.17705837511755,12.7264157868265));
#25363=CARTESIAN_POINT('Ctrl Pts',(7.84992221231509,-2.27727814488456,12.7322546868358));
#25364=CARTESIAN_POINT('Ctrl Pts',(7.78042299958556,-2.37456427892951,12.7380935868451));
#25365=CARTESIAN_POINT('Ctrl Pts',(7.71100774001232,-2.47173289397395,12.7439254336223));
#25366=CARTESIAN_POINT('Ctrl Pts',(7.63724288563745,-2.56597459541495,12.7497572803994));
#25367=CARTESIAN_POINT('Ctrl Pts',(7.55940542000314,-2.65687998084121,12.7555891271765));
#25368=CARTESIAN_POINT('Ctrl Pts',(7.48164203103285,-2.74769885307438,12.7614154238789));
#25369=CARTESIAN_POINT('Ctrl Pts',(7.39981400514475,-2.83518742029049,12.7672417205812));
#25370=CARTESIAN_POINT('Ctrl Pts',(7.31424026387788,-2.91896711362915,12.7730680172836));
#25371=CARTESIAN_POINT('Ctrl Pts',(7.22830852049806,-3.00309730358971,12.7789186885955));
#25372=CARTESIAN_POINT('Ctrl Pts',(7.13859989320791,-3.08348718220274,12.7847693599074));
#25373=CARTESIAN_POINT('Ctrl Pts',(7.04547699114638,-3.15978846946749,12.7906200312193));
#25374=CARTESIAN_POINT('Ctrl Pts',(6.9528375560705,-3.23569362267136,12.7964403275497));
#25375=CARTESIAN_POINT('Ctrl Pts',(6.85681953659431,-3.30755228477065,12.8022606238802));
#25376=CARTESIAN_POINT('Ctrl Pts',(6.7578147457841,-3.37506048053231,12.8080809202106));
#25377=CARTESIAN_POINT('Ctrl Pts',(6.65882230146167,-3.4425602576194,12.8139004907154));
#25378=CARTESIAN_POINT('Ctrl Pts',(6.55684416186541,-3.50571041914857,12.8197200612202));
#25379=CARTESIAN_POINT('Ctrl Pts',(6.45230198519655,-3.56424972738849,12.8255396317249));
#25380=CARTESIAN_POINT('Ctrl Pts',(6.34774858125766,-3.62279532243668,12.8313598272204));
#25381=CARTESIAN_POINT('Ctrl Pts',(6.24063094669848,-3.6767288814336,12.8371800227159));
#25382=CARTESIAN_POINT('Ctrl Pts',(6.13139570863319,-3.7258349234128,12.8430002182114));
#25383=CARTESIAN_POINT('Ctrl Pts',(6.02115704689783,-3.77539204844669,12.8488738774246));
#25384=CARTESIAN_POINT('Ctrl Pts',(5.9087620595364,-3.82003233393355,12.8547475366377));
#25385=CARTESIAN_POINT('Ctrl Pts',(5.79468971302631,-3.85958425319541,12.8606211958508));
#25386=CARTESIAN_POINT('Ctrl Pts',(5.68149632363534,-3.89883141462531,12.866449596991));
#25387=CARTESIAN_POINT('Ctrl Pts',(5.56665174243832,-3.93306829066049,12.8722779981312));
#25388=CARTESIAN_POINT('Ctrl Pts',(5.45063755135768,-3.96217794939712,12.8781063992714));
#25389=CARTESIAN_POINT('Ctrl Pts',(5.33327206892005,-3.99162666691517,12.884002687521));
#25390=CARTESIAN_POINT('Ctrl Pts',(5.21470997644599,-4.01582788214008,12.8898989757706));
#25391=CARTESIAN_POINT('Ctrl Pts',(5.09545770703646,-4.03471418665859,12.8957952640202));
#25392=CARTESIAN_POINT('Ctrl Pts',(4.97620543762694,-4.0536004911771,12.9016915522699));
#25393=CARTESIAN_POINT('Ctrl Pts',(4.85626341900325,-4.06717189238334,12.9075878405195));
#25394=CARTESIAN_POINT('Ctrl Pts',(4.73613955864215,-4.07541524731416,12.9134841287691));
#25395=CARTESIAN_POINT('Ctrl Pts',(4.6171857401835,-4.08357830953164,12.9193229854285));
#25396=CARTESIAN_POINT('Ctrl Pts',(4.49769483746589,-4.08654131907336,12.9251618420879));
#25397=CARTESIAN_POINT('Ctrl Pts',(4.37815714466965,-4.0842492867941,12.9310006987474));
#25398=CARTESIAN_POINT('Ctrl Pts',(4.25876385934941,-4.08196002340379,12.9368325017776));
#25399=CARTESIAN_POINT('Ctrl Pts',(4.13932429883191,-4.07442835476718,12.9426643048079));
#25400=CARTESIAN_POINT('Ctrl Pts',(4.0203327442935,-4.06165115117076,12.9484961078382));
#25401=CARTESIAN_POINT('Ctrl Pts',(3.90145443980128,-4.04888610826005,12.9543223604581));
#25402=CARTESIAN_POINT('Ctrl Pts',(3.7830236942198,-4.03088550700644,12.960148613078));
#25403=CARTESIAN_POINT('Ctrl Pts',(3.66553308053823,-4.00769824254287,12.9659748656978));
#25404=CARTESIAN_POINT('Ctrl Pts',(3.54754971553969,-3.98441373154409,12.9718255534071));
#25405=CARTESIAN_POINT('Ctrl Pts',(3.43051479968968,-3.95589896446489,12.9776762411164));
#25406=CARTESIAN_POINT('Ctrl Pts',(3.31492065169473,-3.92225599954601,12.9835269288257));
#25407=CARTESIAN_POINT('Ctrl Pts',(3.19992783839306,-3.88878804938646,12.9893471805522));
#25408=CARTESIAN_POINT('Ctrl Pts',(3.08636122927721,-3.85024525281661,12.9951674322787));
#25409=CARTESIAN_POINT('Ctrl Pts',(2.97469310746983,-3.80677880753963,13.0009876840053));
#25410=CARTESIAN_POINT('Ctrl Pts',(2.86303891359544,-3.76331778366427,13.0068072097943));
#25411=CARTESIAN_POINT('Ctrl Pts',(2.75328311394058,-3.7149344798687,13.0126267355833));
#25412=CARTESIAN_POINT('Ctrl Pts',(2.64587962648191,-3.66182887856162,13.0184462613723));
#25413=CARTESIAN_POINT('Ctrl Pts',(2.53846460544612,-3.60871757448302,13.024266412094));
#25414=CARTESIAN_POINT('Ctrl Pts',(2.43340276250765,-3.55088314442774,13.0300865628157));
#25415=CARTESIAN_POINT('Ctrl Pts',(2.33112440253129,-3.48857204175426,13.0359067135374));
#25416=CARTESIAN_POINT('Ctrl Pts',(2.22790463662733,-3.42568740581896,13.0417804349694));
#25417=CARTESIAN_POINT('Ctrl Pts',(2.12752021954158,-3.3582434783766,13.0476541564013));
#25418=CARTESIAN_POINT('Ctrl Pts',(2.03038352020519,-3.28653825922343,13.0535278778333));
#25419=CARTESIAN_POINT('Ctrl Pts',(1.93399704139872,-3.21538684442926,13.0593562344708));
#25420=CARTESIAN_POINT('Ctrl Pts',(1.84080856978275,-3.14004003365009,13.0651845911082));
#25421=CARTESIAN_POINT('Ctrl Pts',(1.75118690683325,-3.06082884554011,13.0710129477457));
#25422=CARTESIAN_POINT('Ctrl Pts',(1.66051889362329,-2.98069285147827,13.0769093515749));
#25423=CARTESIAN_POINT('Ctrl Pts',(1.57350181411223,-2.89660196789241,13.0828057554041));
#25424=CARTESIAN_POINT('Ctrl Pts',(1.49047771052929,-2.80893574876657,13.0887021592333));
#25425=CARTESIAN_POINT('Ctrl Pts',(1.40745360694636,-2.72126952964073,13.0945985630626));
#25426=CARTESIAN_POINT('Ctrl Pts',(1.32842271513739,-2.63002833195273,13.1004949668918));
#25427=CARTESIAN_POINT('Ctrl Pts',(1.25368315383551,-2.53562362018094,13.106391370721));
#25428=CARTESIAN_POINT('Ctrl Pts',(1.17967308579315,-2.44214034278348,13.1122302228765));
#25429=CARTESIAN_POINT('Ctrl Pts',(1.10964768046145,-2.34527308168121,13.1180690750319));
#25430=CARTESIAN_POINT('Ctrl Pts',(1.04392958940042,-2.24539507573978,13.1239079271874));
#25431=CARTESIAN_POINT('Ctrl Pts',(0.978290892232233,-2.14563773221525,
13.1297397254374));
#25432=CARTESIAN_POINT('Ctrl Pts',(0.916949378879206,-2.04287721577925,
13.1355715236874));
#25433=CARTESIAN_POINT('Ctrl Pts',(0.860187187972853,-1.93751938429037,
13.1414033219374));
#25434=CARTESIAN_POINT('Ctrl Pts',(0.803479023060019,-1.8322618319033,13.1472295695085));
#25435=CARTESIAN_POINT('Ctrl Pts',(0.751341699701744,-1.7244122386103,13.1530558170796));
#25436=CARTESIAN_POINT('Ctrl Pts',(0.704013486062314,-1.61440447805371,
13.1588820646507));
#25437=CARTESIAN_POINT('Ctrl Pts',(0.656486723895358,-1.50393521943507,
13.1647327541516));
#25438=CARTESIAN_POINT('Ctrl Pts',(0.61380973751515,-1.39128999224299,13.1705834436526));
#25439=CARTESIAN_POINT('Ctrl Pts',(0.576176808876447,-1.27693253039838,
13.1764341331535));
#25440=CARTESIAN_POINT('Ctrl Pts',(0.538739699238071,-1.16317011562208,
13.1822543792047));
#25441=CARTESIAN_POINT('Ctrl Pts',(0.506294399078778,-1.04771363468968,
13.188074625256));
#25442=CARTESIAN_POINT('Ctrl Pts',(0.478983332969678,-0.931038089234241,
13.1938948713072));
#25443=CARTESIAN_POINT('Ctrl Pts',(0.451675674329161,-0.814377100817839,
13.1997143911948));
#25444=CARTESIAN_POINT('Ctrl Pts',(0.429501067866308,-0.696497745366419,
13.2055339110823));
#25445=CARTESIAN_POINT('Ctrl Pts',(0.412551318847235,-0.577887470866143,
13.2113534309698));
#25446=CARTESIAN_POINT('Ctrl Pts',(0.395599750310187,-0.459264463815885,
13.2171735755699));
#25447=CARTESIAN_POINT('Ctrl Pts',(0.383874211789774,-0.339910783308017,
13.22299372017));
#25448=CARTESIAN_POINT('Ctrl Pts',(0.377414829203158,-0.220320687100959,
13.22881386477));
#25449=CARTESIAN_POINT('Ctrl Pts',(0.37089597694503,-0.0996295593878255,
13.234687593762));
#25450=CARTESIAN_POINT('Ctrl Pts',(0.369740775116918,0.0213019396648289,
13.2405613227539));
#25451=CARTESIAN_POINT('Ctrl Pts',(0.373936695342714,0.141965186403322,
13.2464350517458));
#25452=CARTESIAN_POINT('Ctrl Pts',(0.378100198935577,0.261696218998671,
13.2522634017728));
#25453=CARTESIAN_POINT('Ctrl Pts',(0.387532339693921,0.381162726950705,
13.2580917517998));
#25454=CARTESIAN_POINT('Ctrl Pts',(0.402168717863373,0.499873344943745,
13.2639201018268));
#25455=CARTESIAN_POINT('Ctrl Pts',(0.41697603215237,0.619970366878633,13.2698165203012));
#25456=CARTESIAN_POINT('Ctrl Pts',(0.437109846561945,0.739293308218146,
13.2757129387755));
#25457=CARTESIAN_POINT('Ctrl Pts',(0.462450598692844,0.857345415538152,
13.2816093572499));
#25458=CARTESIAN_POINT('Ctrl Pts',(0.487791350823743,0.975397522858159,
13.2875057757243));
#25459=CARTESIAN_POINT('Ctrl Pts',(0.518338879667798,1.09217839974952,13.2934021941986));
#25460=CARTESIAN_POINT('Ctrl Pts',(0.553922463351789,1.20720946825788,13.299298612673));
#25461=CARTESIAN_POINT('Ctrl Pts',(0.589158638859341,1.32111747018309,13.3051374634777));
#25462=CARTESIAN_POINT('Ctrl Pts',(0.629439213296274,1.43365326605997,13.3109763142825));
#25463=CARTESIAN_POINT('Ctrl Pts',(0.67463886394955,1.54433967075305,13.3168151650872));
#25464=CARTESIAN_POINT('Ctrl Pts',(0.719783911027166,1.65489236039775,13.3226469622504));
#25465=CARTESIAN_POINT('Ctrl Pts',(0.769836060649829,1.76359973066888,13.3284787594137));
#25466=CARTESIAN_POINT('Ctrl Pts',(0.824620176145967,1.86999955859155,13.3343105565769));
#25467=CARTESIAN_POINT('Ctrl Pts',(0.879352150831858,1.97629812042298,13.3401368033242));
#25468=CARTESIAN_POINT('Ctrl Pts',(0.938806945629637,2.08029315087318,13.3459630500714));
#25469=CARTESIAN_POINT('Ctrl Pts',(1.00276150719696,2.18154276154798,13.3517892968187));
#25470=CARTESIAN_POINT('Ctrl Pts',(1.0669843807211,2.28321715007287,13.3576399867273));
#25471=CARTESIAN_POINT('Ctrl Pts',(1.13574470350305,2.38212264872249,13.3634906766359));
#25472=CARTESIAN_POINT('Ctrl Pts',(1.20876991878967,2.47783675571566,13.3693413665445));
#25473=CARTESIAN_POINT('Ctrl Pts',(1.28141514775869,2.57305281486445,13.3751616124194));
#25474=CARTESIAN_POINT('Ctrl Pts',(1.35828073431569,2.66511029600926,13.3809818582943));
#25475=CARTESIAN_POINT('Ctrl Pts',(1.43905549995296,2.75362309126083,13.3868021041692));
#25476=CARTESIAN_POINT('Ctrl Pts',(1.51982019110276,2.8421248469131,13.3926216241244));
#25477=CARTESIAN_POINT('Ctrl Pts',(1.60449281800116,2.92708249657188,13.3984411440796));
#25478=CARTESIAN_POINT('Ctrl Pts',(1.69272330849149,3.00814463840212,13.4042606640348));
#25479=CARTESIAN_POINT('Ctrl Pts',(1.78096327402854,3.0892154854722,13.4100808089466));
#25480=CARTESIAN_POINT('Ctrl Pts',(1.87276156410223,3.16638971847438,13.4159009538584));
#25481=CARTESIAN_POINT('Ctrl Pts',(1.9677332618258,3.23935470376987,13.4217210987701));
#25482=CARTESIAN_POINT('Ctrl Pts',(2.06357934224492,3.31299146099376,13.4275948284247));
#25483=CARTESIAN_POINT('Ctrl Pts',(2.16265723391086,3.38234080424751,13.4334685580792));
#25484=CARTESIAN_POINT('Ctrl Pts',(2.26454039229395,3.44712539851308,13.4393422877338));
#25485=CARTESIAN_POINT('Ctrl Pts',(2.36563643116316,3.51140948593184,13.4451706386692));
#25486=CARTESIAN_POINT('Ctrl Pts',(2.46949415929186,3.57119895695132,13.4509989896046));
#25487=CARTESIAN_POINT('Ctrl Pts',(2.57567192763767,3.62626901553692,13.4568273405401));
#25488=CARTESIAN_POINT('Ctrl Pts',(2.68308972369881,3.68198222569742,13.4627237595542));
#25489=CARTESIAN_POINT('Ctrl Pts',(2.79288170743545,3.7328649066331,13.4686201785683));
#25490=CARTESIAN_POINT('Ctrl Pts',(2.90457058759781,3.7787347072669,13.4745165975825));
#25491=CARTESIAN_POINT('Ctrl Pts',(3.01625946776017,3.8246045079007,13.4804130165966));
#25492=CARTESIAN_POINT('Ctrl Pts',(3.12984482636902,3.86546133681569,13.4863094356108));
#25493=CARTESIAN_POINT('Ctrl Pts',(3.24483542673019,3.90117531350874,13.4922058546249));
#25494=CARTESIAN_POINT('Ctrl Pts',(3.35870348020416,3.93654064767587,13.4980447123533));
#25495=CARTESIAN_POINT('Ctrl Pts',(3.47429291146674,3.96696980476108,13.5038835700816));
#25496=CARTESIAN_POINT('Ctrl Pts',(3.59113930905819,3.99229624929648,13.50972242781));
#25497=CARTESIAN_POINT('Ctrl Pts',(3.70784454623759,4.01759209732723,13.5155542317003));
#25498=CARTESIAN_POINT('Ctrl Pts',(3.82580333555408,4.03779741068712,13.5213860355906));
#25499=CARTESIAN_POINT('Ctrl Pts',(3.94453543076624,4.0527951973839,13.527217839481));
#25500=CARTESIAN_POINT('Ctrl Pts',(4.063154518653,4.06777870942512,13.5330440927528));
#25501=CARTESIAN_POINT('Ctrl Pts',(4.18254504751353,4.07756450613422,13.5388703460247));
#25502=CARTESIAN_POINT('Ctrl Pts',(4.30221643997545,4.08208661286808,13.5446965992966));
#25503=CARTESIAN_POINT('Ctrl Pts',(4.42238970978578,4.08662768439285,13.5505472866832));
#25504=CARTESIAN_POINT('Ctrl Pts',(4.54284579927312,4.08586073163649,13.5563979740699));
#25505=CARTESIAN_POINT('Ctrl Pts',(4.66308212298528,4.07977156974532,13.5622486614566));
#25506=CARTESIAN_POINT('Ctrl Pts',(4.78269297231005,4.07371408392912,13.5680689133226));
#25507=CARTESIAN_POINT('Ctrl Pts',(4.90208592820469,4.06238965990478,13.5738891651887));
#25508=CARTESIAN_POINT('Ctrl Pts',(5.02076657283072,4.04583654751085,13.5797094170548));
#25509=CARTESIAN_POINT('Ctrl Pts',(5.13943241094131,4.02928550027182,13.5855289427902));
#25510=CARTESIAN_POINT('Ctrl Pts',(5.25738571286766,4.00750711838774,13.5913484685257));
#25511=CARTESIAN_POINT('Ctrl Pts',(5.3741386848926,3.98059135611474,13.5971679942611));
#25512=CARTESIAN_POINT('Ctrl Pts',(5.49090419061957,3.95367270437232,13.6029881447361));
#25513=CARTESIAN_POINT('Ctrl Pts',(5.60646871493071,3.92161566681467,13.6088082952112));
#25514=CARTESIAN_POINT('Ctrl Pts',(5.72035672823374,3.88456086049837,13.6146284456862));
#25515=CARTESIAN_POINT('Ctrl Pts',(5.83529300139865,3.84716499049131,13.6205021665937));
#25516=CARTESIAN_POINT('Ctrl Pts',(5.94852134084145,3.80467900203611,13.6263758875013));
#25517=CARTESIAN_POINT('Ctrl Pts',(6.05957178679717,3.75729780500834,13.6322496084088));
#25518=CARTESIAN_POINT('Ctrl Pts',(6.16976454776242,3.7102825510542,13.6380779643274));
#25519=CARTESIAN_POINT('Ctrl Pts',(6.27781259618175,3.6584476694299,13.6439063202459));
#25520=CARTESIAN_POINT('Ctrl Pts',(6.3832807544057,3.60203024312803,13.6497346761645));
#25521=CARTESIAN_POINT('Ctrl Pts',(6.48998027922065,3.54495412954965,13.6556310795665));
#25522=CARTESIAN_POINT('Ctrl Pts',(6.59403892002381,3.48318800327208,13.6615274829686));
#25523=CARTESIAN_POINT('Ctrl Pts',(6.69503634868013,3.41702234423136,13.6674238863706));
#25524=CARTESIAN_POINT('Ctrl Pts',(6.79603377733645,3.35085668519065,13.6733202897727));
#25525=CARTESIAN_POINT('Ctrl Pts',(6.89396968205752,3.28029178637921,13.6792166931748));
#25526=CARTESIAN_POINT('Ctrl Pts',(6.9884591187628,3.20565930447614,13.6851130965768));
#25527=CARTESIAN_POINT('Ctrl Pts',(7.08114847821915,3.13244861359426,13.6908971701568));
#25528=CARTESIAN_POINT('Ctrl Pts',(7.17081330379056,3.05509332019825,13.6966812437367));
#25529=CARTESIAN_POINT('Ctrl Pts',(7.25705769295394,2.97387433625659,13.7024653173167));
#25530=CARTESIAN_POINT('Ctrl Pts',(7.34318780350787,2.89276297198312,13.7082417266777));
#25531=CARTESIAN_POINT('Ctrl Pts',(7.42590619518058,2.80779838380308,13.7140181360387));
#25532=CARTESIAN_POINT('Ctrl Pts',(7.50484862644894,2.7193027232432,13.7197945453996));
#25533=CARTESIAN_POINT('Ctrl Pts',(7.5718505635827,2.64419253737513,13.7246972398143));
#25534=CARTESIAN_POINT('Ctrl Pts',(7.63613282774662,2.56653948717263,13.7295999342291));
#25535=CARTESIAN_POINT('Ctrl Pts',(7.69749241145743,2.48656247355587,13.7345026286438));
#25536=CARTESIAN_POINT('Ctrl Pts',(7.69775011106531,2.486760611716,12.4842647253843));
#25537=CARTESIAN_POINT('Ctrl Pts',(7.88067047589132,2.25281987648989,12.4987330318779));
#25538=CARTESIAN_POINT('Ctrl Pts',(8.35218024080415,1.49234549316982,12.5421829289241));
#25539=CARTESIAN_POINT('Ctrl Pts',(8.53713895924919,0.59800099527881,12.5856328259703));
#25540=CARTESIAN_POINT('Ctrl Pts',(8.53584491900118,0.000952226708496463,
12.6146144165228));
#25541=CARTESIAN_POINT('',(8.54146807353351,-0.00290465713063073,12.5103849713801));
#25542=CARTESIAN_POINT('Ctrl Pts',(7.69749241145744,2.48656247355586,12.3802773657823));
#25543=CARTESIAN_POINT('Ctrl Pts',(7.76924068774468,2.39304468020431,12.3860209409451));
#25544=CARTESIAN_POINT('Ctrl Pts',(7.83701986349459,2.29631207426909,12.3917645161079));
#25545=CARTESIAN_POINT('Ctrl Pts',(7.90052900384754,2.19674222919793,12.3975080912707));
#25546=CARTESIAN_POINT('Ctrl Pts',(7.96399713349499,2.09723668084958,12.4032479575489));
#25547=CARTESIAN_POINT('Ctrl Pts',(8.02320048347776,1.99489788651667,12.4089878238271));
#25548=CARTESIAN_POINT('Ctrl Pts',(8.07788012219632,1.8901341892449,12.4147276901054));
#25549=CARTESIAN_POINT('Ctrl Pts',(8.13253810792986,1.78541197810618,12.4204652834125));
#25550=CARTESIAN_POINT('Ctrl Pts',(8.18267575054377,1.67826714401205,12.4262028767196));
#25551=CARTESIAN_POINT('Ctrl Pts',(8.22807936496054,1.56913385539592,12.4319404700267));
#25552=CARTESIAN_POINT('Ctrl Pts',(8.27347633802212,1.46001653011095,12.4376772240748));
#25553=CARTESIAN_POINT('Ctrl Pts',(8.31414050054795,1.3489117158947,12.4434139781229));
#25554=CARTESIAN_POINT('Ctrl Pts',(8.34990605934031,1.23627411687835,12.4491507321709));
#25555=CARTESIAN_POINT('Ctrl Pts',(8.38568972458393,1.12357949464567,12.4548903904727));
#25556=CARTESIAN_POINT('Ctrl Pts',(8.41656970369862,1.00935093669711,12.4606300487745));
#25557=CARTESIAN_POINT('Ctrl Pts',(8.44242997616946,0.894058691148153,12.4663697070763));
#25558=CARTESIAN_POINT('Ctrl Pts',(8.46829731461118,0.778734943547124,12.4721109336624));
#25559=CARTESIAN_POINT('Ctrl Pts',(8.48914213702818,0.662347341222967,12.4778521602484));
#25560=CARTESIAN_POINT('Ctrl Pts',(8.50489977007518,0.545375246910505,12.4835933868345));
#25561=CARTESIAN_POINT('Ctrl Pts',(8.52067402217595,0.428279786003641,12.4893406685021));
#25562=CARTESIAN_POINT('Ctrl Pts',(8.53135033061166,0.310599019056449,12.4950879501697));
#25563=CARTESIAN_POINT('Ctrl Pts',(8.53691600221979,0.192816308727098,12.5008352318374));
#25564=CARTESIAN_POINT('Ctrl Pts',(8.53999866038249,0.127580006806133,12.5040184783516));
#25565=CARTESIAN_POINT('Ctrl Pts',(8.54151444644693,0.0623124390438113,
12.5072017248658));
#25566=CARTESIAN_POINT('Ctrl Pts',(8.54146807353351,-0.00290465713062882,
12.5103849713801));
#25567=CARTESIAN_POINT('Ctrl Pts',(8.54146807353315,-0.00290465763095525,
12.5103849714045));
#25568=CARTESIAN_POINT('Ctrl Pts',(8.54134087188272,-0.181796174867856,
12.5191166664979));
#25569=CARTESIAN_POINT('Ctrl Pts',(8.52945913442029,-0.360258821209145,
12.5278483615914));
#25570=CARTESIAN_POINT('Ctrl Pts',(8.50601097951343,-0.53706202288814,12.5365800566848));
#25571=CARTESIAN_POINT('Ctrl Pts',(8.50003337196073,-0.582134232530938,
12.5388060163284));
#25572=CARTESIAN_POINT('Ctrl Pts',(8.4933043018107,-0.627098745221606,12.5410319759719));
#25573=CARTESIAN_POINT('Ctrl Pts',(8.48582734134787,-0.671935423231146,
12.5432579356155));
#25574=CARTESIAN_POINT('Ctrl Pts',(8.46621380814478,-0.789550820186742,
12.5490970641751));
#25575=CARTESIAN_POINT('Ctrl Pts',(8.44141674655492,-0.906483969071624,
12.5549361927347));
#25576=CARTESIAN_POINT('Ctrl Pts',(8.41149627214712,-1.02224513535862,12.5607753212943));
#25577=CARTESIAN_POINT('Ctrl Pts',(8.38161192889726,-1.13786651158331,12.5666073986797));
#25578=CARTESIAN_POINT('Ctrl Pts',(8.34661658124467,-1.25231833093802,12.5724394760652));
#25579=CARTESIAN_POINT('Ctrl Pts',(8.30662171669774,-1.36511899701738,12.5782715534506));
#25580=CARTESIAN_POINT('Ctrl Pts',(8.26666490120857,-1.47781235034275,12.5840980824975));
#25581=CARTESIAN_POINT('Ctrl Pts',(8.22171816737487,-1.58885729550491,12.5899246115443));
#25582=CARTESIAN_POINT('Ctrl Pts',(8.17194321602948,-1.69778595215126,12.5957511405912));
#25583=CARTESIAN_POINT('Ctrl Pts',(8.12196276023786,-1.80716433948863,12.6016017254652));
#25584=CARTESIAN_POINT('Ctrl Pts',(8.06711423663364,-1.91440852484665,12.6074523103392));
#25585=CARTESIAN_POINT('Ctrl Pts',(8.00761096041533,-2.01906328067485,12.6133028952132));
#25586=CARTESIAN_POINT('Ctrl Pts',(7.94841334308679,-2.12318044162577,12.6191234265609));
#25587=CARTESIAN_POINT('Ctrl Pts',(7.88460889250782,-2.22473436194133,12.6249439579086));
#25588=CARTESIAN_POINT('Ctrl Pts',(7.81645412473464,-2.32330059943718,12.6307644892563));
#25589=CARTESIAN_POINT('Ctrl Pts',(7.74830784934303,-2.42185455514957,12.6365842953404));
#25590=CARTESIAN_POINT('Ctrl Pts',(7.67581256576471,-2.51742123506149,12.6424041014245));
#25591=CARTESIAN_POINT('Ctrl Pts',(7.59926799309304,-2.60960536416108,12.6482239075086));
#25592=CARTESIAN_POINT('Ctrl Pts',(7.5227151965993,-2.70179939737079,12.654044338863));
#25593=CARTESIAN_POINT('Ctrl Pts',(7.44211250513552,-2.79060984511978,12.6598647702174));
#25594=CARTESIAN_POINT('Ctrl Pts',(7.35779937464784,-2.87567516828553,12.6656852015718));
#25595=CARTESIAN_POINT('Ctrl Pts',(7.27271994995913,-2.96151362208319,12.6715585329048));
#25596=CARTESIAN_POINT('Ctrl Pts',(7.1838625901503,-3.04353822672158,12.6774318642378));
#25597=CARTESIAN_POINT('Ctrl Pts',(7.09161260727117,-3.12141694248914,12.6833051955707));
#25598=CARTESIAN_POINT('Ctrl Pts',(7.00006464315778,-3.19870300427225,12.6891338310817));
#25599=CARTESIAN_POINT('Ctrl Pts',(6.90517587314553,-3.27190585709956,12.6949624665927));
#25600=CARTESIAN_POINT('Ctrl Pts',(6.80735376868783,-3.34074337592175,12.7007911021037));
#25601=CARTESIAN_POINT('Ctrl Pts',(6.70840646794043,-3.41037269656827,12.7066867813476));
#25602=CARTESIAN_POINT('Ctrl Pts',(6.60645828806868,-3.47553539771189,12.7125824605916));
#25603=CARTESIAN_POINT('Ctrl Pts',(6.50195748839191,-3.53598674748539,12.7184781398355));
#25604=CARTESIAN_POINT('Ctrl Pts',(6.39745668871515,-3.59643809725888,12.7243738190795));
#25605=CARTESIAN_POINT('Ctrl Pts',(6.29040367073468,-3.6521779490307,12.7302694983234));
#25606=CARTESIAN_POINT('Ctrl Pts',(6.1812675513243,-3.70301165590381,12.7361651775674));
#25607=CARTESIAN_POINT('Ctrl Pts',(6.07318232100037,-3.75335587691225,12.7420040863763));
#25608=CARTESIAN_POINT('Ctrl Pts',(5.96272810830869,-3.79903982898839,12.7478429951853));
#25609=CARTESIAN_POINT('Ctrl Pts',(5.85034275302209,-3.83983609764082,12.7536819039942));
#25610=CARTESIAN_POINT('Ctrl Pts',(5.73809313555261,-3.88058309300103,12.7595137606322));
#25611=CARTESIAN_POINT('Ctrl Pts',(5.62391739373644,-3.91645401109673,12.7653456172702));
#25612=CARTESIAN_POINT('Ctrl Pts',(5.50827571355101,-3.94726840495689,12.7711774739082));
#25613=CARTESIAN_POINT('Ctrl Pts',(5.3927440668114,-3.97805347881813,12.7770037815151));
#25614=CARTESIAN_POINT('Ctrl Pts',(5.2757496470666,-4.00379149764778,12.782830089122));
#25615=CARTESIAN_POINT('Ctrl Pts',(5.15776973081019,-4.02435118173684,12.7886563967289));
#25616=CARTESIAN_POINT('Ctrl Pts',(5.03929653612431,-4.04499682663176,12.7945070643452));
#25617=CARTESIAN_POINT('Ctrl Pts',(4.91982997550732,-4.06042059919596,12.8003577319614));
#25618=CARTESIAN_POINT('Ctrl Pts',(4.79986616233747,-4.07054092988246,12.8062083995777));
#25619=CARTESIAN_POINT('Ctrl Pts',(4.680524816102,-4.08060874830672,12.8120287093132));
#25620=CARTESIAN_POINT('Ctrl Pts',(4.56069177431652,-4.085428005872,12.8178490190487));
#25621=CARTESIAN_POINT('Ctrl Pts',(4.44086211976386,-4.08497018617927,12.8236693287843));
#25622=CARTESIAN_POINT('Ctrl Pts',(4.32104738966884,-4.08451242350675,12.829488913616));
#25623=CARTESIAN_POINT('Ctrl Pts',(4.20123645154675,-4.07877889260651,12.8353084984478));
#25624=CARTESIAN_POINT('Ctrl Pts',(4.08192476980127,-4.06779320271541,12.8411280832795));
#25625=CARTESIAN_POINT('Ctrl Pts',(3.96260025600268,-4.05680633130584,12.8469482940116));
#25626=CARTESIAN_POINT('Ctrl Pts',(3.84377550930107,-4.04056621496815,12.8527685047437));
#25627=CARTESIAN_POINT('Ctrl Pts',(3.72594064703243,-4.01914831404855,12.8585887154758));
#25628=CARTESIAN_POINT('Ctrl Pts',(3.60702402556105,-3.99753379040646,12.8644623574794));
#25629=CARTESIAN_POINT('Ctrl Pts',(3.48911597154714,-3.97064599758179,12.8703359994831));
#25630=CARTESIAN_POINT('Ctrl Pts',(3.37270834167444,-3.93861493487687,12.8762096414867));
#25631=CARTESIAN_POINT('Ctrl Pts',(3.25719698051881,-3.90683049208431,12.8820380599806));
#25632=CARTESIAN_POINT('Ctrl Pts',(3.14316338995698,-3.86998188550789,12.8878664784745));
#25633=CARTESIAN_POINT('Ctrl Pts',(3.03107066098493,-3.8282455867311,12.8936948969684));
#25634=CARTESIAN_POINT('Ctrl Pts',(2.91767331740115,-3.78602353133368,12.8995911507269));
#25635=CARTESIAN_POINT('Ctrl Pts',(2.806262694842,-3.73879945511024,12.9054874044853));
#25636=CARTESIAN_POINT('Ctrl Pts',(2.69729429427881,-3.68680471154055,12.9113836582438));
#25637=CARTESIAN_POINT('Ctrl Pts',(2.58832589371562,-3.63480996797085,12.9172799120023));
#25638=CARTESIAN_POINT('Ctrl Pts',(2.4818000634012,-3.57804480545435,12.9231761657608));
#25639=CARTESIAN_POINT('Ctrl Pts',(2.37814277736662,-3.51678612810075,12.9290724195193));
#25640=CARTESIAN_POINT('Ctrl Pts',(2.2754962665976,-3.4561247918337,12.934911178164));
#25641=CARTESIAN_POINT('Ctrl Pts',(2.17535292698837,-3.39087421999619,12.9407499368087));
#25642=CARTESIAN_POINT('Ctrl Pts',(2.07814793218568,-3.32126683558369,12.9465886954534));
#25643=CARTESIAN_POINT('Ctrl Pts',(1.98106039525784,-3.25174356141123,12.9524203988209));
#25644=CARTESIAN_POINT('Ctrl Pts',(1.88690446724543,-3.17787418187297,12.9582521021883));
#25645=CARTESIAN_POINT('Ctrl Pts',(1.79608922994093,-3.09993611448662,12.9640838055558));
#25646=CARTESIAN_POINT('Ctrl Pts',(1.70536045084141,-3.02207224594185,12.9699099570069));
#25647=CARTESIAN_POINT('Ctrl Pts',(1.61796634064222,-2.94014765955751,12.975736108458));
#25648=CARTESIAN_POINT('Ctrl Pts',(1.53428510214239,-2.85448167734931,12.9815622599091));
#25649=CARTESIAN_POINT('Ctrl Pts',(1.45025091187488,-2.76845437209674,12.9874129849742));
#25650=CARTESIAN_POINT('Ctrl Pts',(1.3699613197849,-2.67865428144424,12.9932637100393));
#25651=CARTESIAN_POINT('Ctrl Pts',(1.29376422719912,-2.58544441986834,12.9991144351044));
#25652=CARTESIAN_POINT('Ctrl Pts',(1.2179653618943,-2.4927216990543,13.0049345826467));
#25653=CARTESIAN_POINT('Ctrl Pts',(1.14621657333452,-2.39662508607003,13.010754730189));
#25654=CARTESIAN_POINT('Ctrl Pts',(1.07882138956362,-2.29754671381835,13.0165748777313));
#25655=CARTESIAN_POINT('Ctrl Pts',(1.01143462280293,-2.19848071550238,13.0223942983932));
#25656=CARTESIAN_POINT('Ctrl Pts',(0.948400607313289,-2.09643403410519,
13.0282137190551));
#25657=CARTESIAN_POINT('Ctrl Pts',(0.889980100662972,-1.99182860037029,
13.0340331397169));
#25658=CARTESIAN_POINT('Ctrl Pts',(0.83155332862376,-1.88721194807943,13.0398531844907));
#25659=CARTESIAN_POINT('Ctrl Pts',(0.777741247004828,-1.78003635203042,
13.0456732292645));
#25660=CARTESIAN_POINT('Ctrl Pts',(0.728758828868994,-1.67074866097342,
13.0514932740382));
#25661=CARTESIAN_POINT('Ctrl Pts',(0.679323445976223,-1.56045033233869,
13.0573671396576));
#25662=CARTESIAN_POINT('Ctrl Pts',(0.634807689365803,-1.44800102578564,
13.0632410052771));
#25663=CARTESIAN_POINT('Ctrl Pts',(0.595382571242502,-1.33387996814883,
13.0691148708965));
#25664=CARTESIAN_POINT('Ctrl Pts',(0.556263625545629,-1.22064516584329,
13.0749431205286));
#25665=CARTESIAN_POINT('Ctrl Pts',(0.522156588801595,-1.10576489519778,
13.0807713701606));
#25666=CARTESIAN_POINT('Ctrl Pts',(0.49317784274618,-0.989720849980289,
13.0865996197927));
#25667=CARTESIAN_POINT('Ctrl Pts',(0.463858884569635,-0.872314441094877,
13.0924962934058));
#25668=CARTESIAN_POINT('Ctrl Pts',(0.439789486603947,-0.753717176795685,
13.0983929670189));
#25669=CARTESIAN_POINT('Ctrl Pts',(0.421036494612281,-0.634435684042738,
13.104289640632));
#25670=CARTESIAN_POINT('Ctrl Pts',(0.402283502620615,-0.515154191289791,
13.1101863142451));
#25671=CARTESIAN_POINT('Ctrl Pts',(0.388846908711802,-0.395188898015737,
13.1160829878582));
#25672=CARTESIAN_POINT('Ctrl Pts',(0.380739271722795,-0.275047843480715,
13.1219796614713));
#25673=CARTESIAN_POINT('Ctrl Pts',(0.372711071968696,-0.156083910366433,
13.1278185604889));
#25674=CARTESIAN_POINT('Ctrl Pts',(0.369883613835015,-0.0365888074691707,
13.1336574595066));
#25675=CARTESIAN_POINT('Ctrl Pts',(0.372311325438709,0.0829471018040055,
13.1394963585243));
#25676=CARTESIAN_POINT('Ctrl Pts',(0.374736104427346,0.202338614680651,
13.1453282042975));
#25677=CARTESIAN_POINT('Ctrl Pts',(0.382403416590484,0.32177043345333,13.1511600500708));
#25678=CARTESIAN_POINT('Ctrl Pts',(0.395315826060202,0.440748267224361,
13.1569918958441));
#25679=CARTESIAN_POINT('Ctrl Pts',(0.408215946971634,0.559612871466202,
13.1628181915319));
#25680=CARTESIAN_POINT('Ctrl Pts',(0.42635118959713,0.678023949096839,13.1686444872197));
#25681=CARTESIAN_POINT('Ctrl Pts',(0.449672095205043,0.795488977004324,
13.1744707829075));
#25682=CARTESIAN_POINT('Ctrl Pts',(0.473090570595575,0.913445453976044,
13.1803214545956));
#25683=CARTESIAN_POINT('Ctrl Pts',(0.501738186921314,1.03044753359977,13.1861721262838));
#25684=CARTESIAN_POINT('Ctrl Pts',(0.535512326060149,1.1460030227412,13.192022797972));
#25685=CARTESIAN_POINT('Ctrl Pts',(0.569111111575057,1.2609585536216,13.1978430932683));
#25686=CARTESIAN_POINT('Ctrl Pts',(0.60778318924555,1.37448208898405,13.2036633885647));
#25687=CARTESIAN_POINT('Ctrl Pts',(0.651376821521075,1.48610151232606,13.209483683861));
#25688=CARTESIAN_POINT('Ctrl Pts',(0.694965017369136,1.59770701595395,13.2153032533263));
#25689=CARTESIAN_POINT('Ctrl Pts',(0.743473399315608,1.70740850214749,13.2211228227916));
#25690=CARTESIAN_POINT('Ctrl Pts',(0.796701466056448,1.81475227511203,13.2269423922569));
#25691=CARTESIAN_POINT('Ctrl Pts',(0.849935249169389,1.92210757614787,13.2327625867087));
#25692=CARTESIAN_POINT('Ctrl Pts',(0.907889544653471,2.0271042970717,13.2385827811605));
#25693=CARTESIAN_POINT('Ctrl Pts',(0.970317407141414,2.12931240803774,13.2444029756123));
#25694=CARTESIAN_POINT('Ctrl Pts',(1.03331875227718,2.23245943595158,13.2502766362632));
#25695=CARTESIAN_POINT('Ctrl Pts',(1.10087606255093,2.33276599500634,13.2561502969141));
#25696=CARTESIAN_POINT('Ctrl Pts',(1.17269088283348,2.42982007145051,13.262023957565));
#25697=CARTESIAN_POINT('Ctrl Pts',(1.24395232102069,2.52612628014296,13.2678523576607));
#25698=CARTESIAN_POINT('Ctrl Pts',(1.31940558078958,2.6192296763458,13.2736807577564));
#25699=CARTESIAN_POINT('Ctrl Pts',(1.39871922202046,2.70876182889677,13.2795091578521));
#25700=CARTESIAN_POINT('Ctrl Pts',(1.47895673070527,2.79933687697666,13.2854054487806));
#25701=CARTESIAN_POINT('Ctrl Pts',(1.56314482844506,2.88625664717841,13.2913017397091));
#25702=CARTESIAN_POINT('Ctrl Pts',(1.65090360063393,2.96917954894533,13.2971980306377));
#25703=CARTESIAN_POINT('Ctrl Pts',(1.7386623728228,3.05210245071224,13.3030943215662));
#25704=CARTESIAN_POINT('Ctrl Pts',(1.82999146227194,3.13102824863487,13.3089906124947));
#25705=CARTESIAN_POINT('Ctrl Pts',(1.92447909665735,3.20565930683277,13.3148869034232));
#25706=CARTESIAN_POINT('Ctrl Pts',(2.01804635339524,3.27956340474405,13.3207257602291));
#25707=CARTESIAN_POINT('Ctrl Pts',(2.11499307489557,3.34947899065648,13.3265646170351));
#25708=CARTESIAN_POINT('Ctrl Pts',(2.2149456546496,3.41508383734098,13.332403473841));
#25709=CARTESIAN_POINT('Ctrl Pts',(2.31477748671508,3.48060943010711,13.3382352770175));
#25710=CARTESIAN_POINT('Ctrl Pts',(2.41760761688817,3.54183442230089,13.344067080194));
#25711=CARTESIAN_POINT('Ctrl Pts',(2.52302986581768,3.59847713674535,13.3498988833705));
#25712=CARTESIAN_POINT('Ctrl Pts',(2.62835177926144,3.65506594156139,13.355725136136));
#25713=CARTESIAN_POINT('Ctrl Pts',(2.73626054717992,3.70708095509481,13.3615513889015));
#25714=CARTESIAN_POINT('Ctrl Pts',(2.84632202440033,3.75428440250776,13.367377641667));
#25715=CARTESIAN_POINT('Ctrl Pts',(2.95684509161434,3.80168581781591,13.3732283293215));
#25716=CARTESIAN_POINT('Ctrl Pts',(3.06953861804267,3.84423499240065,13.379079016976));
#25717=CARTESIAN_POINT('Ctrl Pts',(3.18393865006805,3.88173817228442,13.3849297046305));
#25718=CARTESIAN_POINT('Ctrl Pts',(3.29774356320336,3.91904625737326,13.3907499565004));
#25719=CARTESIAN_POINT('Ctrl Pts',(3.4132368772308,3.95136060343397,13.3965702083702));
#25720=CARTESIAN_POINT('Ctrl Pts',(3.52994342808911,3.97853932590431,13.40239046024));
#25721=CARTESIAN_POINT('Ctrl Pts',(3.64663542256786,4.0057146584724,13.4082099861712));
#25722=CARTESIAN_POINT('Ctrl Pts',(3.76453995782569,4.02775554971939,13.4140295121023));
#25723=CARTESIAN_POINT('Ctrl Pts',(3.88316948104885,4.0445707485196,13.4198490380335));
#25724=CARTESIAN_POINT('Ctrl Pts',(4.00181174333475,4.06138775302438,13.425669188896));
#25725=CARTESIAN_POINT('Ctrl Pts',(4.12117874671891,4.07297789239719,13.4314893397585));
#25726=CARTESIAN_POINT('Ctrl Pts',(4.24077618740749,4.07930160257546,13.437309490621));
#25727=CARTESIAN_POINT('Ctrl Pts',(4.36147443784173,4.08568351802762,13.4431832118505));
#25728=CARTESIAN_POINT('Ctrl Pts',(4.48240696941911,4.08670153095217,13.44905693308));
#25729=CARTESIAN_POINT('Ctrl Pts',(4.60306517603562,4.08236874771423,13.4549306543095));
#25730=CARTESIAN_POINT('Ctrl Pts',(4.7227915042599,4.07806942782032,13.4607590110831));
#25731=CARTESIAN_POINT('Ctrl Pts',(4.84224732746244,4.06850176594928,13.4665873678567));
#25732=CARTESIAN_POINT('Ctrl Pts',(4.96094135312177,4.05373072022599,13.4724157246303));
#25733=CARTESIAN_POINT('Ctrl Pts',(5.08102114412744,4.03878722097625,13.4783121280878));
#25734=CARTESIAN_POINT('Ctrl Pts',(5.20032081395789,4.01851813519756,13.4842085315452));
#25735=CARTESIAN_POINT('Ctrl Pts',(5.31834375020069,3.99304358829952,13.4901049350027));
#25736=CARTESIAN_POINT('Ctrl Pts',(5.4363666864435,3.96756904140149,13.4960013384602));
#25737=CARTESIAN_POINT('Ctrl Pts',(5.55311249288124,3.93688919484002,13.5018977419176));
#25738=CARTESIAN_POINT('Ctrl Pts',(5.66810279045029,3.90117531203535,13.5077941453751));
#25739=CARTESIAN_POINT('Ctrl Pts',(5.7819541725698,3.8658151555341,13.5136321482098));
#25740=CARTESIAN_POINT('Ctrl Pts',(5.89442803691065,3.82541362846627,13.5194701510445));
#25741=CARTESIAN_POINT('Ctrl Pts',(6.00504754787872,3.78009653448483,13.5253081538791));
#25742=CARTESIAN_POINT('Ctrl Pts',(6.11554146611341,3.7348308916231,13.5311395284913));
#25743=CARTESIAN_POINT('Ctrl Pts',(6.22418484561038,3.68466093299057,13.5369709031034));
#25744=CARTESIAN_POINT('Ctrl Pts',(6.33051575959186,3.62976227058728,13.5428022777156));
#25745=CARTESIAN_POINT('Ctrl Pts',(6.4367506424443,3.57491318906632,13.5486283858115));
#25746=CARTESIAN_POINT('Ctrl Pts',(6.54067685555499,3.5153440839737,13.5544544939073));
#25747=CARTESIAN_POINT('Ctrl Pts',(6.64185278983194,3.45127848128702,13.5602806020032));
#25748=CARTESIAN_POINT('Ctrl Pts',(6.74296309344481,3.38725443658623,13.5661029308274));
#25749=CARTESIAN_POINT('Ctrl Pts',(6.84132632583219,3.31873991355129,13.5719252596516));
#25750=CARTESIAN_POINT('Ctrl Pts',(6.93652632958691,3.2460038768949,13.5777475884758));
#25751=CARTESIAN_POINT('Ctrl Pts',(7.03168744040331,3.17329755576451,13.5835675386502));
#25752=CARTESIAN_POINT('Ctrl Pts',(7.12368757265028,3.09637339939824,13.5893874888245));
#25753=CARTESIAN_POINT('Ctrl Pts',(7.21214086356068,3.01554276470838,13.5952074389989));
#25754=CARTESIAN_POINT('Ctrl Pts',(7.30060389556322,2.93470322838635,13.6010280301066));
#25755=CARTESIAN_POINT('Ctrl Pts',(7.38551899932978,2.84995662030946,13.6068486212144));
#25756=CARTESIAN_POINT('Ctrl Pts',(7.46653478833146,2.76165341586596,13.6126692123222));
#25757=CARTESIAN_POINT('Ctrl Pts',(7.54752149206514,2.67338191292656,13.6184877137946));
#25758=CARTESIAN_POINT('Ctrl Pts',(7.62461141413523,2.58155667271329,13.6243062152671));
#25759=CARTESIAN_POINT('Ctrl Pts',(7.69749241145744,2.48656247355586,13.6301247167396));
#25760=CARTESIAN_POINT('Origin',(4.45646910621825,2.93978508838399E-15,
8.23961502859548));
#25761=CARTESIAN_POINT('',(7.69668968132766,2.48593167737218,14.9842676783293));
#25762=CARTESIAN_POINT('',(7.70074909849077,2.48902547716684,14.8803008071898));
#25763=CARTESIAN_POINT('',(7.69749241145744,2.48656247355586,8.23961502859548));
#25764=CARTESIAN_POINT('',(8.54454168082834,-0.00144745710864128,13.8646150285955));
#25765=CARTESIAN_POINT('Ctrl Pts',(8.54666930739189,-0.00144821043386754,
13.8646150285955));
#25766=CARTESIAN_POINT('Ctrl Pts',(8.54710349746243,-0.0928747809970434,
13.8690834652399));
#25767=CARTESIAN_POINT('Ctrl Pts',(8.5037729238356,-1.49954483890456,13.9378543158683));
#25768=CARTESIAN_POINT('Ctrl Pts',(6.8902438015866,-4.1182632906804,14.0709275804807));
#25769=CARTESIAN_POINT('Ctrl Pts',(2.43669343542057,-4.33631261202236,14.2638348224326));
#25770=CARTESIAN_POINT('Ctrl Pts',(-0.262050461583375,-0.786882051116074,
14.4567420643845));
#25771=CARTESIAN_POINT('Ctrl Pts',(1.13891927667451,3.44634822095808,14.6496493063365));
#25772=CARTESIAN_POINT('Ctrl Pts',(5.04320204593008,4.57543617360612,14.8254911776514));
#25773=CARTESIAN_POINT('Ctrl Pts',(7.0992059979852,3.25061891740341,14.9370306349823));
#25774=CARTESIAN_POINT('Ctrl Pts',(7.69668968132748,2.48593167737241,14.9842676783293));
#25775=CARTESIAN_POINT('Ctrl Pts',(7.69749241145743,2.48656247355587,13.7345026286438));
#25776=CARTESIAN_POINT('Ctrl Pts',(7.76968844409539,2.39246106777425,13.7402711665733));
#25777=CARTESIAN_POINT('Ctrl Pts',(7.83783719235359,2.29514180401789,13.7460397045029));
#25778=CARTESIAN_POINT('Ctrl Pts',(7.90164394098947,2.19499324779346,13.7518082424324));
#25779=CARTESIAN_POINT('Ctrl Pts',(7.96542734353023,2.09488133467919,13.7575746697258));
#25780=CARTESIAN_POINT('Ctrl Pts',(8.02487168246655,1.9919425361957,13.7633410970191));
#25781=CARTESIAN_POINT('Ctrl Pts',(8.07972515864914,1.88659496938868,13.7691075243125));
#25782=CARTESIAN_POINT('Ctrl Pts',(8.13457196419649,1.7812602137149,13.7748732503607));
#25783=CARTESIAN_POINT('Ctrl Pts',(8.18482882630859,1.67351763997037,13.7806389764089));
#25784=CARTESIAN_POINT('Ctrl Pts',(8.23028991805605,1.56380992455593,13.7864047024571));
#25785=CARTESIAN_POINT('Ctrl Pts',(8.27575658665505,1.45408875095962,13.7921711358046));
#25786=CARTESIAN_POINT('Ctrl Pts',(8.31642615768105,1.3424023396563,13.7979375691521));
#25787=CARTESIAN_POINT('Ctrl Pts',(8.35214123659239,1.22921261489865,13.8037040024996));
#25788=CARTESIAN_POINT('Ctrl Pts',(8.38788801935198,1.11592241297654,13.809475554641));
#25789=CARTESIAN_POINT('Ctrl Pts',(8.41867140396666,1.00112662887301,13.8152471067824));
#25790=CARTESIAN_POINT('Ctrl Pts',(8.44438410516932,0.88530162156231,13.8210186589238));
#25791=CARTESIAN_POINT('Ctrl Pts',(8.47010954482429,0.769419232830652,13.8267930703774));
#25792=CARTESIAN_POINT('Ctrl Pts',(8.49075922567521,0.652507013129004,13.8325674818311));
#25793=CARTESIAN_POINT('Ctrl Pts',(8.50627742689127,0.535049124667352,13.8383418932847));
#25794=CARTESIAN_POINT('Ctrl Pts',(8.52181666906985,0.417431976315101,13.8441241342009));
#25795=CARTESIAN_POINT('Ctrl Pts',(8.53221050295707,0.29926809418751,13.8499063751171));
#25796=CARTESIAN_POINT('Ctrl Pts',(8.53745524789854,0.181044501195737,13.8556886160333));
#25797=CARTESIAN_POINT('Ctrl Pts',(8.54015412986084,0.120208078032049,13.8586640868873));
#25798=CARTESIAN_POINT('Ctrl Pts',(8.54149037829185,0.059355818985477,13.8616395577414));
#25799=CARTESIAN_POINT('Ctrl Pts',(8.54146885016146,-0.00144636911655798,
13.8646150285955));
#25800=CARTESIAN_POINT('',(8.53888143287343,0.00293751736108398,13.7603849714045));
#25801=CARTESIAN_POINT('Ctrl Pts',(7.69749241145744,2.48656247355586,13.6301247167396));
#25802=CARTESIAN_POINT('Ctrl Pts',(7.77116112387467,2.39054155457618,13.6360061059552));
#25803=CARTESIAN_POINT('Ctrl Pts',(7.84052912275375,2.29128309709694,13.6418874951708));
#25804=CARTESIAN_POINT('Ctrl Pts',(7.90531826065341,2.18921550103037,13.6477688843864));
#25805=CARTESIAN_POINT('Ctrl Pts',(7.96952297950996,2.08806858779367,13.6535972215633));
#25806=CARTESIAN_POINT('Ctrl Pts',(8.0292309536961,1.98416339191401,13.6594255587401));
#25807=CARTESIAN_POINT('Ctrl Pts',(8.0842177015797,1.87794172669251,13.6652538959169));
#25808=CARTESIAN_POINT('Ctrl Pts',(8.13995521910658,1.77026974835418,13.6711618111519));
#25809=CARTESIAN_POINT('Ctrl Pts',(8.1908414495447,1.66021796802013,13.677069726387));
#25810=CARTESIAN_POINT('Ctrl Pts',(8.23669336405316,1.54826663093806,13.682977641622));
#25811=CARTESIAN_POINT('Ctrl Pts',(8.28254527856162,1.43631529385599,13.688885556857));
#25812=CARTESIAN_POINT('Ctrl Pts',(8.32336278519854,1.32246482218004,13.694793472092));
#25813=CARTESIAN_POINT('Ctrl Pts',(8.35901574908476,1.20720946825774,13.7007013873271));
#25814=CARTESIAN_POINT('Ctrl Pts',(8.40091264668397,1.07176934674485,13.7076439607528));
#25815=CARTESIAN_POINT('Ctrl Pts',(8.43578063747411,0.934062884985015,13.7145865341786));
#25816=CARTESIAN_POINT('Ctrl Pts',(8.46341078772054,0.794759939251718,13.7215291076044));
#25817=CARTESIAN_POINT('Ctrl Pts',(8.49078114782047,0.656766777662076,13.7284064040718));
#25818=CARTESIAN_POINT('Ctrl Pts',(8.51104909580129,0.517207073291735,13.7352837005392));
#25819=CARTESIAN_POINT('Ctrl Pts',(8.52405849112768,0.376751371293978,13.7421609970066));
#25820=CARTESIAN_POINT('Ctrl Pts',(8.53554956117983,0.252688240734315,13.7482356448664));
#25821=CARTESIAN_POINT('Ctrl Pts',(8.54137809438647,0.127926344822457,13.7543102927261));
#25822=CARTESIAN_POINT('Ctrl Pts',(8.54146804824079,0.00294001266690675,
13.7603849405859));
#25823=CARTESIAN_POINT('Ctrl Pts',(8.53888143287343,0.00293751736108398,
13.7603849714045));
#25824=CARTESIAN_POINT('Ctrl Pts',(8.53231291773911,-0.910184697636579,
13.8047928573627));
#25825=CARTESIAN_POINT('Ctrl Pts',(7.78645395877844,-3.15524707040652,13.9135031573048));
#25826=CARTESIAN_POINT('Ctrl Pts',(4.12896712280502,-4.77242649979729,14.0865158712309));
#25827=CARTESIAN_POINT('Ctrl Pts',(0.335454948527761,-2.42911695903736,
14.2794231131828));
#25828=CARTESIAN_POINT('Ctrl Pts',(0.122429391055361,2.02471691783314,14.4723303551348));
#25829=CARTESIAN_POINT('Ctrl Pts',(3.67497223820188,4.71936388741884,14.6652375970867));
#25830=CARTESIAN_POINT('Ctrl Pts',(6.65799943773292,3.7284653965522,14.8012277477717));
#25831=CARTESIAN_POINT('Ctrl Pts',(7.60957770066985,2.60967412627678,14.8729154844728));
#25832=CARTESIAN_POINT('Ctrl Pts',(7.70074909849077,2.48902547716684,14.8803008071898));
#25833=CARTESIAN_POINT('Origin',(4.45646910621825,3.5527136788005E-15,11.));
#25834=CARTESIAN_POINT('',(7.63534122785693,-1.17693546839596,12.1796263343991));
#25835=CARTESIAN_POINT('',(7.6353412143218,-1.17693550495398,11.8350241089739));
#25836=CARTESIAN_POINT('',(7.63534122785693,-1.17693546839596,11.));
#25837=CARTESIAN_POINT('',(7.84621824929258,-0.00241029600555726,12.1089821966925));
#25838=CARTESIAN_POINT('Ctrl Pts',(7.84621824929188,-0.00241029699009288,
12.1089821967504));
#25839=CARTESIAN_POINT('Ctrl Pts',(7.84610765710331,-0.157942904798472,
12.1181307971768));
#25840=CARTESIAN_POINT('Ctrl Pts',(7.83528910987164,-0.313084630689196,
12.1272793976032));
#25841=CARTESIAN_POINT('Ctrl Pts',(7.81394315636294,-0.466661617347083,
12.1364279980296));
#25842=CARTESIAN_POINT('Ctrl Pts',(7.80972218403832,-0.497030099603801,
12.1382370523402));
#25843=CARTESIAN_POINT('Ctrl Pts',(7.80508971167061,-0.527337486378948,
12.1400461066508));
#25844=CARTESIAN_POINT('Ctrl Pts',(7.80004733817191,-0.557574810501385,
12.1418551609614));
#25845=CARTESIAN_POINT('Ctrl Pts',(7.7825007520135,-0.662795459675959,12.1481503565343));
#25846=CARTESIAN_POINT('Ctrl Pts',(7.759954023632,-0.767358033495362,12.1544455521073));
#25847=CARTESIAN_POINT('Ctrl Pts',(7.73247177283944,-0.870753461543981,
12.1607407476803));
#25848=CARTESIAN_POINT('Ctrl Pts',(7.70498952204689,-0.974148889592601,
12.1670359432532));
#25849=CARTESIAN_POINT('Ctrl Pts',(7.67257179221753,-1.07637668136229,12.1733311388262));
#25850=CARTESIAN_POINT('Ctrl Pts',(7.63534122785693,-1.17693546839596,12.1796263343991));
#25851=CARTESIAN_POINT('',(7.03046338747139,-2.20566509302208,11.000004601718));
#25852=CARTESIAN_POINT('Ctrl Pts',(7.03046338747139,-2.20566509302208,11.000004601718));
#25853=CARTESIAN_POINT('Ctrl Pts',(6.96364411350853,-2.28364267429769,11.0060599561424));
#25854=CARTESIAN_POINT('Ctrl Pts',(6.89316717227375,-2.35871057473643,11.0121153105668));
#25855=CARTESIAN_POINT('Ctrl Pts',(6.81931811192614,-2.43050398862565,11.0181706649912));
#25856=CARTESIAN_POINT('Ctrl Pts',(6.74555740159863,-2.50221151178682,11.0242187750352));
#25857=CARTESIAN_POINT('Ctrl Pts',(6.66843290009554,-2.57065203402839,11.0302668850792));
#25858=CARTESIAN_POINT('Ctrl Pts',(6.58826985773396,-2.63549437835429,11.0363149951232));
#25859=CARTESIAN_POINT('Ctrl Pts',(6.50818175580784,-2.7002761048022,11.0423574510903));
#25860=CARTESIAN_POINT('Ctrl Pts',(6.42506109837629,-2.76146607043511,11.0483999070575));
#25861=CARTESIAN_POINT('Ctrl Pts',(6.3392686178572,-2.81877119707722,11.0544423630247));
#25862=CARTESIAN_POINT('Ctrl Pts',(6.25351932447536,-2.87604747685122,11.0604817772756));
#25863=CARTESIAN_POINT('Ctrl Pts',(6.16510124073695,-2.9294425618507,11.0665211915266));
#25864=CARTESIAN_POINT('Ctrl Pts',(6.07440605265532,-2.97870527240509,11.0725606057776));
#25865=CARTESIAN_POINT('Ctrl Pts',(5.98373213828396,-3.02795642776396,11.0785986034072));
#25866=CARTESIAN_POINT('Ctrl Pts',(5.89078256297615,-3.07307692789121,11.0846366010367));
#25867=CARTESIAN_POINT('Ctrl Pts',(5.79597483524122,-3.11386086144108,11.0906745986663));
#25868=CARTESIAN_POINT('Ctrl Pts',(5.70116385893125,-3.15464619244739,11.0967128031871));
#25869=CARTESIAN_POINT('Ctrl Pts',(5.60449500353731,-3.19109449113594,11.1027510077078));
#25870=CARTESIAN_POINT('Ctrl Pts',(5.50640609840839,-3.22304783937979,11.1087892122286));
#25871=CARTESIAN_POINT('Ctrl Pts',(5.40823003702718,-3.25502957956131,11.1148327819564));
#25872=CARTESIAN_POINT('Ctrl Pts',(5.30863181993906,-3.28250825767039,11.1208763516841));
#25873=CARTESIAN_POINT('Ctrl Pts',(5.20806460500747,-3.30537581353464,11.1269199214119));
#25874=CARTESIAN_POINT('Ctrl Pts',(5.1074515196614,-3.32825379967944,11.1329662477144));
#25875=CARTESIAN_POINT('Ctrl Pts',(5.00586898412057,-3.34651639752689,11.1390125740169));
#25876=CARTESIAN_POINT('Ctrl Pts',(4.90377855029586,-3.36010704051805,11.1450589003194));
#25877=CARTESIAN_POINT('Ctrl Pts',(4.80153271273702,-3.37371837140906,11.1511144304391));
#25878=CARTESIAN_POINT('Ctrl Pts',(4.69877786588522,-3.38264350423802,11.1571699605588));
#25879=CARTESIAN_POINT('Ctrl Pts',(4.59597894094542,-3.38687792347383,11.1632254906785));
#25880=CARTESIAN_POINT('Ctrl Pts',(4.5162285551083,-3.39016294389646,11.1679233108529));
#25881=CARTESIAN_POINT('Ctrl Pts',(4.43645172653599,-3.39062591871191,11.1726211310273));
#25882=CARTESIAN_POINT('Ctrl Pts',(4.35686353873807,-3.38828626202494,11.1773189512018));
#25883=CARTESIAN_POINT('Ctrl Pts',(4.25307543195265,-3.38523519948931,11.1834452103291));
#25884=CARTESIAN_POINT('Ctrl Pts',(4.14926928185013,-3.37740639907282,11.1895714694564));
#25885=CARTESIAN_POINT('Ctrl Pts',(4.04591729830903,-3.3647960228701,11.1956977285837));
#25886=CARTESIAN_POINT('Ctrl Pts',(3.94269237402144,-3.35220114965951,11.2018164561873));
#25887=CARTESIAN_POINT('Ctrl Pts',(3.83992092339695,-3.33483644124615,11.2079351837909));
#25888=CARTESIAN_POINT('Ctrl Pts',(3.73807358322337,-3.31275005622834,11.2140539113945));
#25889=CARTESIAN_POINT('Ctrl Pts',(3.63632306575806,-3.29068466796518,11.2201668221376));
#25890=CARTESIAN_POINT('Ctrl Pts',(3.53549532339145,-3.26390662077776,11.2262797328806));
#25891=CARTESIAN_POINT('Ctrl Pts',(3.43605348907385,-3.23251558863802,11.2323926436237));
#25892=CARTESIAN_POINT('Ctrl Pts',(3.33667388802547,-3.20114420181724,11.2385017287492));
#25893=CARTESIAN_POINT('Ctrl Pts',(3.23867887293101,-3.16516569891973,11.2446108138748));
#25894=CARTESIAN_POINT('Ctrl Pts',(3.14251830080288,-3.12473012329838,11.2507198990004));
#25895=CARTESIAN_POINT('Ctrl Pts',(3.04638798576622,-3.0843072708013,11.2568270618916));
#25896=CARTESIAN_POINT('Ctrl Pts',(2.9520913562225,-3.03943029779103,11.2629342247829));
#25897=CARTESIAN_POINT('Ctrl Pts',(2.86005937057485,-2.99029781433939,11.2690413876742));
#25898=CARTESIAN_POINT('Ctrl Pts',(2.76803311035823,-2.94116838748426,11.2751481706309));
#25899=CARTESIAN_POINT('Ctrl Pts',(2.67827158723843,-2.88778417655825,11.2812549535875));
#25900=CARTESIAN_POINT('Ctrl Pts',(2.59118140944753,-2.83038987964128,11.2873617365441));
#25901=CARTESIAN_POINT('Ctrl Pts',(2.5040746653177,-2.77298466515128,11.2934696811362));
#25902=CARTESIAN_POINT('Ctrl Pts',(2.41964062997498,-2.71156808176117,11.2995776257283));
#25903=CARTESIAN_POINT('Ctrl Pts',(2.33825643994187,-2.64642781177312,11.3056855703204));
#25904=CARTESIAN_POINT('Ctrl Pts',(2.2567896085224,-2.58122139524953,11.3117997172106));
#25905=CARTESIAN_POINT('Ctrl Pts',(2.17837913695186,-2.51228400757457,11.3179138641007));
#25906=CARTESIAN_POINT('Ctrl Pts',(2.10336854946749,-2.43994320268305,11.3240280109909));
#25907=CARTESIAN_POINT('Ctrl Pts',(2.02831557589694,-2.3675615203142,11.3301456127902));
#25908=CARTESIAN_POINT('Ctrl Pts',(1.95666660454135,-2.29177289708959,11.3362632145894));
#25909=CARTESIAN_POINT('Ctrl Pts',(1.88872651126045,-2.21293990621964,11.3423808163886));
#25910=CARTESIAN_POINT('Ctrl Pts',(1.82068557647108,-2.13398990582949,11.3485074983667));
#25911=CARTESIAN_POINT('Ctrl Pts',(1.75636477447799,-2.05198684699319,11.3546341803447));
#25912=CARTESIAN_POINT('Ctrl Pts',(1.69602714989169,-1.96732439324378,11.3607608623227));
#25913=CARTESIAN_POINT('Ctrl Pts',(1.66495456278761,-1.92372503899987,11.3639159725997));
#25914=CARTESIAN_POINT('Ctrl Pts',(1.63493760256666,-1.87942085103863,11.3670710828767));
#25915=CARTESIAN_POINT('Ctrl Pts',(1.60600744878302,-1.83446815235141,11.3702261931537));
#25916=CARTESIAN_POINT('Ctrl Pts',(1.54997323606809,-1.74740020590397,11.3763372605791));
#25917=CARTESIAN_POINT('Ctrl Pts',(1.49784136340171,-1.6576218645813,11.3824483280045));
#25918=CARTESIAN_POINT('Ctrl Pts',(1.44988280934613,-1.56551713563308,11.3885593954299));
#25919=CARTESIAN_POINT('Ctrl Pts',(1.40198544232448,-1.47352991679927,11.394662666163));
#25920=CARTESIAN_POINT('Ctrl Pts',(1.35825100267684,-1.37922258670873,11.4007659368961));
#25921=CARTESIAN_POINT('Ctrl Pts',(1.31890687553446,-1.28300752573264,11.4068692076292));
#25922=CARTESIAN_POINT('Ctrl Pts',(1.27960179886222,-1.18688796168679,11.4129664206453));
#25923=CARTESIAN_POINT('Ctrl Pts',(1.24467852910567,-1.08886482493238,11.4190636336613));
#25924=CARTESIAN_POINT('Ctrl Pts',(1.21431785207666,-0.989373694701926,
11.4251608466773));
#25925=CARTESIAN_POINT('Ctrl Pts',(1.18397767780842,-0.889949751472577,
11.4312539422061));
#25926=CARTESIAN_POINT('Ctrl Pts',(1.15819409251278,-0.78906019282724,11.4373470377349));
#25927=CARTESIAN_POINT('Ctrl Pts',(1.137098915894,-0.687158352992052,11.4434401332636));
#25928=CARTESIAN_POINT('Ctrl Pts',(1.11601099280535,-0.585291551880595,
11.4495311336949));
#25929=CARTESIAN_POINT('Ctrl Pts',(1.09960836013549,-0.482413578327243,
11.4556221341262));
#25930=CARTESIAN_POINT('Ctrl Pts',(1.08797214948141,-0.378989861282093,
11.4617131345575));
#25931=CARTESIAN_POINT('Ctrl Pts',(1.07633695469905,-0.275575173398873,
11.4678036032284));
#25932=CARTESIAN_POINT('Ctrl Pts',(1.06946740168239,-0.171615260226652,
11.4738940718994));
#25933=CARTESIAN_POINT('Ctrl Pts',(1.06739286425132,-0.0675817182033117,
11.4799845405704));
#25934=CARTESIAN_POINT('Ctrl Pts',(1.06531797573343,0.0364694300609991,
11.4860760399691));
#25935=CARTESIAN_POINT('Ctrl Pts',(1.06803972356699,0.14059380593717,11.4921675393678));
#25936=CARTESIAN_POINT('Ctrl Pts',(1.07553536429218,0.244319657837441,11.4982590387665));
#25937=CARTESIAN_POINT('Ctrl Pts',(1.08303851283162,0.348149404048647,11.5043566395577));
#25938=CARTESIAN_POINT('Ctrl Pts',(1.09532507055292,0.451579403665733,11.5104542403489));
#25939=CARTESIAN_POINT('Ctrl Pts',(1.11232038896645,0.554142959355393,11.51655184114));
#25940=CARTESIAN_POINT('Ctrl Pts',(1.12932511918393,0.656763313514801,11.5226528187096));
#25941=CARTESIAN_POINT('Ctrl Pts',(1.15104371547761,0.75851585140497,11.5287537962791));
#25942=CARTESIAN_POINT('Ctrl Pts',(1.17735076910878,0.858945861933337,11.5348547738486));
#25943=CARTESIAN_POINT('Ctrl Pts',(1.20369711598113,0.959525878641883,11.5409648640762));
#25944=CARTESIAN_POINT('Ctrl Pts',(1.23464547965846,1.05877901668213,11.5470749543038));
#25945=CARTESIAN_POINT('Ctrl Pts',(1.27002112670429,1.15626741558838,11.5531850445313));
#25946=CARTESIAN_POINT('Ctrl Pts',(1.28922055696488,1.20917730904112,11.5565011747227));
#25947=CARTESIAN_POINT('Ctrl Pts',(1.30972323911573,1.26156775104713,11.5598173049141));
#25948=CARTESIAN_POINT('Ctrl Pts',(1.33149552586891,1.31337168563153,11.5631334351056));
#25949=CARTESIAN_POINT('Ctrl Pts',(1.37167159184059,1.40896468957506,11.5692526391585));
#25950=CARTESIAN_POINT('Ctrl Pts',(1.41630116220111,1.5028630143177,11.5753718432114));
#25951=CARTESIAN_POINT('Ctrl Pts',(1.46521933320156,1.59462530330093,11.5814910472643));
#25952=CARTESIAN_POINT('Ctrl Pts',(1.51407599835094,1.68627221761737,11.5876025575126));
#25953=CARTESIAN_POINT('Ctrl Pts',(1.56721034389962,1.77578806447175,11.5937140677608));
#25954=CARTESIAN_POINT('Ctrl Pts',(1.6244094644662,1.86275152611917,11.599825578009));
#25955=CARTESIAN_POINT('Ctrl Pts',(1.68155273476896,1.94963007505764,11.6059311208673));
#25956=CARTESIAN_POINT('Ctrl Pts',(1.74275265396909,2.03396084232813,11.6120366637255));
#25957=CARTESIAN_POINT('Ctrl Pts',(1.80775088932139,2.11534793118738,11.6181422065837));
#25958=CARTESIAN_POINT('Ctrl Pts',(1.87270634746321,2.19668145685971,11.6242437312084));
#25959=CARTESIAN_POINT('Ctrl Pts',(1.94145488559652,2.27507482618555,11.6303452558331));
#25960=CARTESIAN_POINT('Ctrl Pts',(2.01369589367489,2.35016256769199,11.6364467804577));
#25961=CARTESIAN_POINT('Ctrl Pts',(2.08591277564395,2.42522523237423,11.6425462673748));
#25962=CARTESIAN_POINT('Ctrl Pts',(2.16161951463887,2.49698415810805,11.6486457542919));
#25963=CARTESIAN_POINT('Ctrl Pts',(2.24047691939051,2.5651089042024,11.6547452412089));
#25964=CARTESIAN_POINT('Ctrl Pts',(2.31932804958399,2.63322822971915,11.6608442427995));
#25965=CARTESIAN_POINT('Ctrl Pts',(2.40132902530304,2.69771367333297,11.6669432443902));
#25966=CARTESIAN_POINT('Ctrl Pts',(2.48610635141016,2.75827403949736,11.6730422459808));
#25967=CARTESIAN_POINT('Ctrl Pts',(2.57089849848763,2.81884499296655,11.6791423138131));
#25968=CARTESIAN_POINT('Ctrl Pts',(2.6584676148026,2.87548925863655,11.6852423816454));
#25969=CARTESIAN_POINT('Ctrl Pts',(2.74841064676608,2.92795856555278,11.6913424494777));
#25970=CARTESIAN_POINT('Ctrl Pts',(2.83844368463475,2.98048037845375,11.6974486216421));
#25971=CARTESIAN_POINT('Ctrl Pts',(2.93085501384979,3.02881867664673,11.7035547938064));
#25972=CARTESIAN_POINT('Ctrl Pts',(3.02521642954576,3.07277087300987,11.7096609659707));
#25973=CARTESIAN_POINT('Ctrl Pts',(3.11963022305209,3.11674746620713,11.7157705275281));
#25974=CARTESIAN_POINT('Ctrl Pts',(3.21599586664937,3.15633294622868,11.7218800890854));
#25975=CARTESIAN_POINT('Ctrl Pts',(3.31386635016529,3.19137337275979,11.7279896506428));
#25976=CARTESIAN_POINT('Ctrl Pts',(3.41188184714174,3.22646571824877,11.7341082646605));
#25977=CARTESIAN_POINT('Ctrl Pts',(3.51140623094587,3.25699943722907,11.7402268786781));
#25978=CARTESIAN_POINT('Ctrl Pts',(3.61197850559916,3.28287079976749,11.7463454926958));
#25979=CARTESIAN_POINT('Ctrl Pts',(3.66509874609967,3.29653552998121,11.7495772208163));
#25980=CARTESIAN_POINT('Ctrl Pts',(3.71851115781609,3.30890044691213,11.7528089489369));
#25981=CARTESIAN_POINT('Ctrl Pts',(3.77214707404916,3.31995608687645,11.7560406770575));
#25982=CARTESIAN_POINT('Ctrl Pts',(3.87369261179996,3.34088704106166,11.7621591065151));
#25983=CARTESIAN_POINT('Ctrl Pts',(3.97635925686529,3.35718786702286,11.7682775359728));
#25984=CARTESIAN_POINT('Ctrl Pts',(4.07968985990864,3.36874493870498,11.7743959654304));
#25985=CARTESIAN_POINT('Ctrl Pts',(4.18289065755572,3.38028749222669,11.7805067088286));
#25986=CARTESIAN_POINT('Ctrl Pts',(4.2867533356158,3.38709809394802,11.7866174522268));
#25987=CARTESIAN_POINT('Ctrl Pts',(4.39081011957819,3.38911403761712,11.7927281956249));
#25988=CARTESIAN_POINT('Ctrl Pts',(4.49476543877261,3.39112801555896,11.7988329804961));
#25989=CARTESIAN_POINT('Ctrl Pts',(4.5989140646279,3.38835662578775,11.8049377653672));
#25990=CARTESIAN_POINT('Ctrl Pts',(4.70278349365506,3.38078900333068,11.8110425502383));
#25991=CARTESIAN_POINT('Ctrl Pts',(4.80658483771223,3.37322634134516,11.8171433335077));
#25992=CARTESIAN_POINT('Ctrl Pts',(4.91010692625367,3.36087373015861,11.823244116777));
#25993=CARTESIAN_POINT('Ctrl Pts',(5.01287843551619,3.34377237873188,11.8293449000463));
#25994=CARTESIAN_POINT('Ctrl Pts',(5.11561579902865,3.3266767092152,11.8354436563354));
#25995=CARTESIAN_POINT('Ctrl Pts',(5.21760266030219,3.30483550566695,11.8415424126245));
#25996=CARTESIAN_POINT('Ctrl Pts',(5.31837476715059,3.27834160729977,11.8476411689135));
#25997=CARTESIAN_POINT('Ctrl Pts',(5.41913904894595,3.2518497662098,11.8537394516282));
#25998=CARTESIAN_POINT('Ctrl Pts',(5.51868835312645,3.22070605722529,11.8598377343428));
#25999=CARTESIAN_POINT('Ctrl Pts',(5.61657139540344,3.18505380506002,11.8659360170575));
#26000=CARTESIAN_POINT('Ctrl Pts',(5.71447175706836,3.14939524459894,11.8720353787999));
#26001=CARTESIAN_POINT('Ctrl Pts',(5.81070487181571,3.10922670121194,11.8781347405424));
#26002=CARTESIAN_POINT('Ctrl Pts',(5.90483814298822,3.06474015143634,11.8842341022849));
#26003=CARTESIAN_POINT('Ctrl Pts',(5.99906599235371,3.02020890484487,11.8903395922177));
#26004=CARTESIAN_POINT('Ctrl Pts',(6.09118940106688,2.97135117154634,11.8964450821506));
#26005=CARTESIAN_POINT('Ctrl Pts',(6.18079922753286,2.91840550561898,11.9025505720835));
#26006=CARTESIAN_POINT('Ctrl Pts',(6.27045898630629,2.86543033735495,11.9086594641121));
#26007=CARTESIAN_POINT('Ctrl Pts',(6.35760201741397,2.80836293144945,11.9147683561406));
#26008=CARTESIAN_POINT('Ctrl Pts',(6.4418486703467,2.74748485871008,11.9208772481691));
#26009=CARTESIAN_POINT('Ctrl Pts',(6.52622052546176,2.68651631273175,11.9269952188564));
#26010=CARTESIAN_POINT('Ctrl Pts',(6.60768707418294,2.62172605487704,11.9331131895437));
#26011=CARTESIAN_POINT('Ctrl Pts',(6.68590217092384,2.55343558221026,11.939231160231));
#26012=CARTESIAN_POINT('Ctrl Pts',(6.72731008577615,2.51728187026412,11.9424700798238));
#26013=CARTESIAN_POINT('Ctrl Pts',(6.76780731826133,2.48014775675753,11.9457089994166));
#26014=CARTESIAN_POINT('Ctrl Pts',(6.80734692460347,2.44208487680596,11.9489479190095));
#26015=CARTESIAN_POINT('Ctrl Pts',(6.88096398400294,2.37121726952471,11.954978321386));
#26016=CARTESIAN_POINT('Ctrl Pts',(6.95150718080944,2.29688915272491,11.9610087237626));
#26017=CARTESIAN_POINT('Ctrl Pts',(7.01862897299606,2.21940124348283,11.9670391261392));
#26018=CARTESIAN_POINT('Ctrl Pts',(7.08564999444784,2.14202966774886,11.9730604750019));
#26019=CARTESIAN_POINT('Ctrl Pts',(7.14925954296759,2.06150806386155,11.9790818238645));
#26020=CARTESIAN_POINT('Ctrl Pts',(7.20914579240184,1.97817494773373,11.9851031727272));
#26021=CARTESIAN_POINT('Ctrl Pts',(7.26898114075436,1.89491266165112,11.9911194036676));
#26022=CARTESIAN_POINT('Ctrl Pts',(7.32509922049556,1.80884396368172,11.997135634608));
#26023=CARTESIAN_POINT('Ctrl Pts',(7.37722785029553,1.72034107705307,12.0031518655484));
#26024=CARTESIAN_POINT('Ctrl Pts',(7.42932646657381,1.63188914674762,12.0091646325904));
#26025=CARTESIAN_POINT('Ctrl Pts',(7.47743997416593,1.54100618929599,12.0151773996323));
#26026=CARTESIAN_POINT('Ctrl Pts',(7.52133959459298,1.44809321246585,12.0211901666743));
#26027=CARTESIAN_POINT('Ctrl Pts',(7.56522597477905,1.35520825843389,12.0272011202499));
#26028=CARTESIAN_POINT('Ctrl Pts',(7.60490080717506,1.26029489868599,12.0332120738256));
#26029=CARTESIAN_POINT('Ctrl Pts',(7.64018184602719,1.16377757878312,12.0392230274012));
#26030=CARTESIAN_POINT('Ctrl Pts',(7.67547718543311,1.06722113726788,12.045236417412));
#26031=CARTESIAN_POINT('Ctrl Pts',(7.70637501566812,0.969059846948902,12.0512498074228));
#26032=CARTESIAN_POINT('Ctrl Pts',(7.73274191522095,0.869736479337045,12.0572631974337));
#26033=CARTESIAN_POINT('Ctrl Pts',(7.75911344850643,0.770395656584837,12.0632776442408));
#26034=CARTESIAN_POINT('Ctrl Pts',(7.78095236506544,0.669892777560101,12.0692920910479));
#26035=CARTESIAN_POINT('Ctrl Pts',(7.79817607439928,0.568682337786512,12.075306537855));
#26036=CARTESIAN_POINT('Ctrl Pts',(7.81541945859331,0.467356284052392,12.0813278550405));
#26037=CARTESIAN_POINT('Ctrl Pts',(7.82803704330347,0.365321490399033,12.087349172226));
#26038=CARTESIAN_POINT('Ctrl Pts',(7.83599799990535,0.263039007058008,12.0933704894115));
#26039=CARTESIAN_POINT('Ctrl Pts',(7.84287822894921,0.17464172671174,12.0985743918385));
#26040=CARTESIAN_POINT('Ctrl Pts',(7.84628115626159,0.0860596860178569,
12.1037782942655));
#26041=CARTESIAN_POINT('Ctrl Pts',(7.84621824929258,-0.00241029600555718,
12.1089821966925));
#26042=CARTESIAN_POINT('',(1.88323467920355,-2.20655152809225,11.));
#26043=CARTESIAN_POINT('Origin',(4.45646910621825,3.5527136788005E-15,11.));
#26044=CARTESIAN_POINT('Ctrl Pts',(1.88323467920354,-2.20655152809226,11.));
#26045=CARTESIAN_POINT('Ctrl Pts',(1.86599707596286,-2.18644939427239,11.0015541500662));
#26046=CARTESIAN_POINT('Ctrl Pts',(1.8489951410639,-2.1661453996546,11.0030951979296));
#26047=CARTESIAN_POINT('Ctrl Pts',(1.81139159419215,-2.12015425598179,11.006526711438));
#26048=CARTESIAN_POINT('Ctrl Pts',(1.79092266321204,-2.09436181098513,11.0084107827258));
#26049=CARTESIAN_POINT('Ctrl Pts',(1.62499832560114,-1.87891046881364,11.0238519423018));
#26050=CARTESIAN_POINT('Ctrl Pts',(1.49959158403363,-1.67464106458276,11.0366502112481));
#26051=CARTESIAN_POINT('Ctrl Pts',(1.33667743832326,-1.33295299818795,11.0574582868395));
#26052=CARTESIAN_POINT('Ctrl Pts',(1.28447620893895,-1.20346180213168,11.0652154451724));
#26053=CARTESIAN_POINT('Ctrl Pts',(1.21548125192911,-0.996304529957284,
11.077703238766));
#26054=CARTESIAN_POINT('Ctrl Pts',(1.19318050994874,-0.920636325469628,
11.0822788091142));
#26055=CARTESIAN_POINT('Ctrl Pts',(1.1523122573658,-0.761719512053923,11.0919578357044));
#26056=CARTESIAN_POINT('Ctrl Pts',(1.13420681741972,-0.678410363563903,
11.0970707307868));
#26057=CARTESIAN_POINT('Ctrl Pts',(1.06422917855726,-0.285601044751504,
11.1214147892952));
#26058=CARTESIAN_POINT('Ctrl Pts',(1.05236403147467,0.0294219237589118,
11.14179860344));
#26059=CARTESIAN_POINT('Ctrl Pts',(1.09634753074839,0.46378243409643,11.1698014612439));
#26060=CARTESIAN_POINT('Ctrl Pts',(1.11537236474605,0.585310845423136,11.1775990267017));
#26061=CARTESIAN_POINT('Ctrl Pts',(1.15078591102381,0.751726609831858,11.1880304145553));
#26062=CARTESIAN_POINT('Ctrl Pts',(1.16157756953607,0.79769954298666,11.1908852127355));
#26063=CARTESIAN_POINT('Ctrl Pts',(1.18344704280919,0.882828367067341,11.1961042093075));
#26064=CARTESIAN_POINT('Ctrl Pts',(1.19427523192246,0.922036107538697,11.1984788403858));
#26065=CARTESIAN_POINT('Ctrl Pts',(1.22738459860688,1.03402645834213,11.2051961989925));
#26066=CARTESIAN_POINT('Ctrl Pts',(1.25141577354736,1.10626953407051,11.2094520277691));
#26067=CARTESIAN_POINT('Ctrl Pts',(1.34699503400008,1.36424923960056,11.2245713213735));
#26068=CARTESIAN_POINT('Ctrl Pts',(1.43243035575875,1.54441045902614,11.2350010545271));
#26069=CARTESIAN_POINT('Ctrl Pts',(1.5873827163874,1.80837236019493,11.2513924892617));
#26070=CARTESIAN_POINT('Ctrl Pts',(1.64592345453565,1.89807758131636,11.2571777844786));
#26071=CARTESIAN_POINT('Ctrl Pts',(1.76041897694343,2.0565864989518,11.2679745692397));
#26072=CARTESIAN_POINT('Ctrl Pts',(1.81501514150776,2.12625338449111,11.2729414045865));
#26073=CARTESIAN_POINT('Ctrl Pts',(1.91502022565397,2.24406019877022,11.2818003746455));
#26074=CARTESIAN_POINT('Ctrl Pts',(1.95922996613896,2.29315598508195,11.2856436733013));
#26075=CARTESIAN_POINT('Ctrl Pts',(2.05967356350227,2.398349410893,11.2942393478943));
#26076=CARTESIAN_POINT('Ctrl Pts',(2.1165002418265,2.45382413784225,11.2990160694685));
#26077=CARTESIAN_POINT('Ctrl Pts',(2.36518002948247,2.68008836632022,11.3195885037407));
#26078=CARTESIAN_POINT('Ctrl Pts',(2.57414599822951,2.83075716253,11.33617056169));
#26079=CARTESIAN_POINT('Ctrl Pts',(2.88432174146297,3.00475251093036,11.359070476376));
#26080=CARTESIAN_POINT('Ctrl Pts',(2.97265184442071,3.04933978594295,11.3654082948755));
#26081=CARTESIAN_POINT('Ctrl Pts',(3.12559804265472,3.11832194519425,11.3759503750373));
#26082=CARTESIAN_POINT('Ctrl Pts',(3.18924058666404,3.14472300507211,11.3802155435408));
#26083=CARTESIAN_POINT('Ctrl Pts',(3.29060010282618,3.18319284747261,11.3867720965788));
#26084=CARTESIAN_POINT('Ctrl Pts',(3.32779580161469,3.19657071234315,11.3891280939164));
#26085=CARTESIAN_POINT('Ctrl Pts',(3.41127574389892,3.22495613083378,11.3943002819086));
#26086=CARTESIAN_POINT('Ctrl Pts',(3.4576636707273,3.23962334989183,11.3970995439316));
#26087=CARTESIAN_POINT('Ctrl Pts',(3.63159529065526,3.29052661118421,11.4073724179686));
#26088=CARTESIAN_POINT('Ctrl Pts',(3.76092336929158,3.32027172265474,11.4145718351935));
#26089=CARTESIAN_POINT('Ctrl Pts',(4.06731017860474,3.37204542548141,11.4312592311656));
#26090=CARTESIAN_POINT('Ctrl Pts',(4.24501204395672,3.38783416809086,11.440668178534));
#26091=CARTESIAN_POINT('Ctrl Pts',(4.54231166880054,3.39075825727141,11.4568327327308));
#26092=CARTESIAN_POINT('Ctrl Pts',(4.66146210208325,3.38564391744804,11.4634206011539));
#26093=CARTESIAN_POINT('Ctrl Pts',(4.85233760093863,3.36733738452042,11.4743083452772));
#26094=CARTESIAN_POINT('Ctrl Pts',(4.92434078053615,3.35808992285324,11.4784918963722));
#26095=CARTESIAN_POINT('Ctrl Pts',(5.07197939904934,3.33428806425678,11.4872541801692));
#26096=CARTESIAN_POINT('Ctrl Pts',(5.14752646565309,3.31945299500239,11.4918389858457));
#26097=CARTESIAN_POINT('Ctrl Pts',(5.39176457972627,3.26279330462831,11.507012139282));
#26098=CARTESIAN_POINT('Ctrl Pts',(5.55774102229941,3.21057400687688,11.5178926534708));
#26099=CARTESIAN_POINT('Ctrl Pts',(5.90438543180064,3.07145903335125,11.5416331507391));
#26100=CARTESIAN_POINT('Ctrl Pts',(6.08286584137707,2.98079861255615,11.5545033000869));
#26101=CARTESIAN_POINT('Ctrl Pts',(6.30284899078352,2.84338443618124,11.570554953987));
#26102=CARTESIAN_POINT('Ctrl Pts',(6.35253513118355,2.8104960842805,11.5741917594508));
#26103=CARTESIAN_POINT('Ctrl Pts',(6.43471717966392,2.75292593343445,11.5801945342524));
#26104=CARTESIAN_POINT('Ctrl Pts',(6.46767730413894,2.72893909535353,11.5825965726888));
#26105=CARTESIAN_POINT('Ctrl Pts',(6.54904336713181,2.66744933865935,11.5885146334459));
#26106=CARTESIAN_POINT('Ctrl Pts',(6.59687960221767,2.62921981924175,11.5919876026597));
#26107=CARTESIAN_POINT('Ctrl Pts',(6.83676138376692,2.4266234467912,11.6095157968681));
#26108=CARTESIAN_POINT('Ctrl Pts',(7.01103279304588,2.24243578382843,11.6226839857892));
#26109=CARTESIAN_POINT('Ctrl Pts',(7.24547380827723,1.93145799718472,11.6437250880342));
#26110=CARTESIAN_POINT('Ctrl Pts',(7.32105273238859,1.81747984360567,11.6512200627761));
#26111=CARTESIAN_POINT('Ctrl Pts',(7.4265070189314,1.63545617439083,11.6631202900468));
#26112=CARTESIAN_POINT('Ctrl Pts',(7.46137672294725,1.57046845839114,11.6673549373204));
#26113=CARTESIAN_POINT('Ctrl Pts',(7.52666551280824,1.43863962808292,11.6759471247199));
#26114=CARTESIAN_POINT('Ctrl Pts',(7.55708705302273,1.37184441781834,11.6803016692319));
#26115=CARTESIAN_POINT('Ctrl Pts',(7.63631703766182,1.18175546240165,11.6927163876306));
#26116=CARTESIAN_POINT('Ctrl Pts',(7.68009141904249,1.05651869234713,11.7009260284344));
#26117=CARTESIAN_POINT('Ctrl Pts',(7.77124250330589,0.736678651269657,11.7219078270026));
#26118=CARTESIAN_POINT('Ctrl Pts',(7.80892991403089,0.539832381377944,11.7348513874113));
#26119=CARTESIAN_POINT('Ctrl Pts',(7.83621918018113,0.269798371086886,11.7520789207683));
#26120=CARTESIAN_POINT('Ctrl Pts',(7.84115195959594,0.198556561711271,11.7565713628072));
#26121=CARTESIAN_POINT('Ctrl Pts',(7.84594020274366,0.0710536103046219,
11.7644649827159));
#26122=CARTESIAN_POINT('Ctrl Pts',(7.84665245852064,0.0148509416709774,
11.7678935900683));
#26123=CARTESIAN_POINT('Ctrl Pts',(7.84547994795152,-0.0812683973432962,
11.7736428003223));
#26124=CARTESIAN_POINT('Ctrl Pts',(7.84428782265352,-0.121176166923975,
11.7759940772057));
#26125=CARTESIAN_POINT('Ctrl Pts',(7.83949257344823,-0.221985910305632,
11.7818483196353));
#26126=CARTESIAN_POINT('Ctrl Pts',(7.83495030864903,-0.282827206983951,
11.7853064847601));
#26127=CARTESIAN_POINT('Ctrl Pts',(7.80310914697135,-0.595411722914734,
11.8028328868572));
#26128=CARTESIAN_POINT('Ctrl Pts',(7.74930659200723,-0.843657386814209,
11.8159983886954));
#26129=CARTESIAN_POINT('Ctrl Pts',(7.65780130280229,-1.11488409573876,11.8314418949571));
#26130=CARTESIAN_POINT('Ctrl Pts',(7.64679635725797,-1.14599546259751,11.8332287944345));
#26131=CARTESIAN_POINT('Ctrl Pts',(7.6353412143218,-1.17693550495398,11.8350241089739));
#26132=CARTESIAN_POINT('Origin',(4.45646910621825,3.5527136788005E-15,11.));
#26133=CARTESIAN_POINT('',(7.63534122785692,-1.17693546839596,13.4294624954408));
#26134=CARTESIAN_POINT('',(7.63534118037484,-1.17693559664385,13.0872737913614));
#26135=CARTESIAN_POINT('',(7.63534122785693,-1.17693546839596,11.));
#26136=CARTESIAN_POINT('',(7.84621822868222,0.00243910941253872,13.3589821967011));
#26137=CARTESIAN_POINT('Ctrl Pts',(7.84621822868283,0.00243910857111449,
13.3589821967504));
#26138=CARTESIAN_POINT('Ctrl Pts',(7.84629283776119,-0.101248796474601,
13.3650553057062));
#26139=CARTESIAN_POINT('Ctrl Pts',(7.84160563766044,-0.205006137387628,
13.3711284146619));
#26140=CARTESIAN_POINT('Ctrl Pts',(7.83216418985855,-0.308363040565317,
13.3772015236177));
#26141=CARTESIAN_POINT('Ctrl Pts',(7.82272594910728,-0.411684835693171,
13.3832725696729));
#26142=CARTESIAN_POINT('Ctrl Pts',(7.80853671345539,-0.514606036863708,
13.3893436157281));
#26143=CARTESIAN_POINT('Ctrl Pts',(7.78965603869954,-0.616660308140516,
13.3954146617833));
#26144=CARTESIAN_POINT('Ctrl Pts',(7.77077031345568,-0.718741878435034,
13.4014873318136));
#26145=CARTESIAN_POINT('Ctrl Pts',(7.74719071430171,-0.819955632267821,
13.4075600018439));
#26146=CARTESIAN_POINT('Ctrl Pts',(7.71902814867664,-0.91984431126849,13.4136326718741));
#26147=CARTESIAN_POINT('Ctrl Pts',(7.69455739458182,-1.00663865142994,13.4189092797297));
#26148=CARTESIAN_POINT('Ctrl Pts',(7.66662732283726,-1.09243253871243,13.4241858875853));
#26149=CARTESIAN_POINT('Ctrl Pts',(7.63534122785692,-1.17693546839597,13.4294624954408));
#26150=CARTESIAN_POINT('Ctrl Pts',(7.63534122785693,-1.17693546839596,12.1796263343991));
#26151=CARTESIAN_POINT('Ctrl Pts',(7.59924171155339,-1.27443932401376,12.1857302847185));
#26152=CARTESIAN_POINT('Ctrl Pts',(7.55861770762308,-1.37037367847503,12.1918342350379));
#26153=CARTESIAN_POINT('Ctrl Pts',(7.5136320904601,-1.46429489867357,12.1979381853572));
#26154=CARTESIAN_POINT('Ctrl Pts',(7.46867510623004,-1.5581563388765,12.2040382505682));
#26155=CARTESIAN_POINT('Ctrl Pts',(7.41936221301803,-1.6500068108107,12.2101383157791));
#26156=CARTESIAN_POINT('Ctrl Pts',(7.36590431060266,-1.73942285082974,12.2162383809901));
#26157=CARTESIAN_POINT('Ctrl Pts',(7.31246346601551,-1.82881035917466,12.2223364997374));
#26158=CARTESIAN_POINT('Ctrl Pts',(7.2548804594675,-1.91576461544835,12.2284346184847));
#26159=CARTESIAN_POINT('Ctrl Pts',(7.19341164031467,-1.99988765373304,12.234532737232));
#26160=CARTESIAN_POINT('Ctrl Pts',(7.13194677682776,-2.08400527849848,12.2406304635507));
#26161=CARTESIAN_POINT('Ctrl Pts',(7.06659684914164,-2.16529170479224,12.2467281898694));
#26162=CARTESIAN_POINT('Ctrl Pts',(6.9976604290699,-2.2433795316806,12.2528259161881));
#26163=CARTESIAN_POINT('Ctrl Pts',(6.92871088510468,-2.32148222467778,12.2589248033724));
#26164=CARTESIAN_POINT('Ctrl Pts',(6.85617377320426,-2.39638478970671,12.2650236905566));
#26165=CARTESIAN_POINT('Ctrl Pts',(6.78038608409376,-2.46775504101237,12.2711225777408));
#26166=CARTESIAN_POINT('Ctrl Pts',(6.7045217732068,-2.53919744804022,12.2772276309339));
#26167=CARTESIAN_POINT('Ctrl Pts',(6.62540063383492,-2.60710011987618,12.2833326841271));
#26168=CARTESIAN_POINT('Ctrl Pts',(6.54339438856573,-2.67116976779816,12.2894377373203));
#26169=CARTESIAN_POINT('Ctrl Pts',(6.46134143492393,-2.73527590792848,12.2955462677742));
#26170=CARTESIAN_POINT('Ctrl Pts',(6.37640044843766,-2.79554442959542,12.3016547982282));
#26171=CARTESIAN_POINT('Ctrl Pts',(6.28897236312811,-2.85172524551625,12.3077633286821));
#26172=CARTESIAN_POINT('Ctrl Pts',(6.20141581713618,-2.90798860957851,12.3138808345813));
#26173=CARTESIAN_POINT('Ctrl Pts',(6.1113652427459,-2.96015206216199,12.3199983404804));
#26174=CARTESIAN_POINT('Ctrl Pts',(6.0192463995132,-3.00801133542773,12.3261158463796));
#26175=CARTESIAN_POINT('Ctrl Pts',(5.97584577192874,-3.03055962655446,12.3289980318908));
#26176=CARTESIAN_POINT('Ctrl Pts',(5.93198634547982,-3.05215320939512,12.331880217402));
#26177=CARTESIAN_POINT('Ctrl Pts',(5.88771403383095,-3.07277448239907,12.3347624029133));
#26178=CARTESIAN_POINT('Ctrl Pts',(5.79374212281867,-3.11654496466023,12.3408800974789));
#26179=CARTESIAN_POINT('Ctrl Pts',(5.69761202737596,-3.1560699057085,12.3469977920445));
#26180=CARTESIAN_POINT('Ctrl Pts',(5.59974222852627,-3.19113328306858,12.3531154866101));
#26181=CARTESIAN_POINT('Ctrl Pts',(5.50199565204499,-3.22615251409901,12.35922547873));
#26182=CARTESIAN_POINT('Ctrl Pts',(5.40251412457098,-3.25672120866668,12.3653354708498));
#26183=CARTESIAN_POINT('Ctrl Pts',(5.30173822038799,-3.28267043535148,12.3714454629697));
#26184=CARTESIAN_POINT('Ctrl Pts',(5.20106084450981,-3.30859429155375,12.3775494813683));
#26185=CARTESIAN_POINT('Ctrl Pts',(5.09909201849968,-3.32990755705062,12.3836534997669));
#26186=CARTESIAN_POINT('Ctrl Pts',(4.99628888419061,-3.34649064989129,12.3897575181655));
#26187=CARTESIAN_POINT('Ctrl Pts',(4.89355347132187,-3.36306281863962,12.3958575155493));
#26188=CARTESIAN_POINT('Ctrl Pts',(4.78998526172517,-3.37491094449382,12.4019575129331));
#26189=CARTESIAN_POINT('Ctrl Pts',(4.68605226650424,-3.38196638584908,12.408057510317));
#26190=CARTESIAN_POINT('Ctrl Pts',(4.58215400582777,-3.3890194692665,12.4141554690737));
#26191=CARTESIAN_POINT('Ctrl Pts',(4.47789162550102,-3.39128302356307,12.4202534278303));
#26192=CARTESIAN_POINT('Ctrl Pts',(4.37373817058073,-3.38874027549892,12.426351386587));
#26193=CARTESIAN_POINT('Ctrl Pts',(4.26959298581961,-3.38619772933812,12.4324488611437));
#26194=CARTESIAN_POINT('Ctrl Pts',(4.16555713410043,-3.37884965056749,12.4385463357005));
#26195=CARTESIAN_POINT('Ctrl Pts',(4.0621026914221,-3.36673138123326,12.4446438102573));
#26196=CARTESIAN_POINT('Ctrl Pts',(3.95863010421886,-3.35461098651674,12.4507423542295));
#26197=CARTESIAN_POINT('Ctrl Pts',(3.85573955074917,-3.33771878829351,12.4568408982018));
#26198=CARTESIAN_POINT('Ctrl Pts',(3.75389614779341,-3.31614177932581,12.462939442174));
#26199=CARTESIAN_POINT('Ctrl Pts',(3.65195056971743,-3.29454312307,12.469044104554));
#26200=CARTESIAN_POINT('Ctrl Pts',(3.55105465609129,-3.26825036007636,12.4751487669339));
#26201=CARTESIAN_POINT('Ctrl Pts',(3.45166144513326,-3.23740121497551,12.4812534293139));
#26202=CARTESIAN_POINT('Ctrl Pts',(3.35221295032704,-3.20653491116292,12.4873614871896));
#26203=CARTESIAN_POINT('Ctrl Pts',(3.25426922269691,-3.17110732122112,12.4934695450653));
#26204=CARTESIAN_POINT('Ctrl Pts',(3.15826452624802,-3.13130482882844,12.4995776029411));
#26205=CARTESIAN_POINT('Ctrl Pts',(3.0621171747642,-3.09144319322556,12.5056947368854));
#26206=CARTESIAN_POINT('Ctrl Pts',(2.96791499270935,-3.04719385380684,12.5118118708297));
#26207=CARTESIAN_POINT('Ctrl Pts',(2.87606885046154,-2.99878977157521,12.517929004774));
#26208=CARTESIAN_POINT('Ctrl Pts',(2.82731833954408,-2.973097633816,12.5211758848044));
#26209=CARTESIAN_POINT('Ctrl Pts',(2.77923113941815,-2.94623572387818,12.5244227648349));
#26210=CARTESIAN_POINT('Ctrl Pts',(2.73186526944357,-2.91824376443813,12.5276696448653));
#26211=CARTESIAN_POINT('Ctrl Pts',(2.64262191263345,-2.86550333286866,12.5337871820969));
#26212=CARTESIAN_POINT('Ctrl Pts',(2.55565895113433,-2.8085820529641,12.5399047193284));
#26213=CARTESIAN_POINT('Ctrl Pts',(2.47139121516819,-2.7477028276297,12.54602225656));
#26214=CARTESIAN_POINT('Ctrl Pts',(2.38722962559938,-2.6869002877594,12.5521320879415));
#26215=CARTESIAN_POINT('Ctrl Pts',(2.30575685286816,-2.62214996278217,12.558241919323));
#26216=CARTESIAN_POINT('Ctrl Pts',(2.22736139037672,-2.55371961140524,12.5643517507045));
#26217=CARTESIAN_POINT('Ctrl Pts',(2.14904261733581,-2.48535620122465,12.5704556052144));
#26218=CARTESIAN_POINT('Ctrl Pts',(2.07379548602307,-2.41332020266512,12.5765594597244));
#26219=CARTESIAN_POINT('Ctrl Pts',(2.00197716475091,-2.33792095071066,12.5826633142343));
#26220=CARTESIAN_POINT('Ctrl Pts',(1.93020620209745,-2.26257141872127,12.5887631437251));
#26221=CARTESIAN_POINT('Ctrl Pts',(1.8618598449964,-2.18386335119967,12.5948629732159));
#26222=CARTESIAN_POINT('Ctrl Pts',(1.79725940115328,-2.10214385972707,12.6009628027067));
#26223=CARTESIAN_POINT('Ctrl Pts',(1.73268057287378,-2.02045171191905,12.6070605911704));
#26224=CARTESIAN_POINT('Ctrl Pts',(1.67184542949749,-1.93575047638809,12.6131583796341));
#26225=CARTESIAN_POINT('Ctrl Pts',(1.61503535218568,-1.84842075403421,12.6192561680979));
#26226=CARTESIAN_POINT('Ctrl Pts',(1.55822980625213,-1.76109799741638,12.6253534701799));
#26227=CARTESIAN_POINT('Ctrl Pts',(1.50544891930639,-1.67114752740054,12.6314507722618));
#26228=CARTESIAN_POINT('Ctrl Pts',(1.4569305466712,-1.57897862312647,12.6375480743438));
#26229=CARTESIAN_POINT('Ctrl Pts',(1.40840367996345,-1.48679358291633,12.6436464438756));
#26230=CARTESIAN_POINT('Ctrl Pts',(1.36414100829734,-1.39238971280386,12.6497448134073));
#26231=CARTESIAN_POINT('Ctrl Pts',(1.32433385594505,-1.29619976720259,12.6558431829391));
#26232=CARTESIAN_POINT('Ctrl Pts',(1.2844867784221,-1.19991334647645,12.6619476689205));
#26233=CARTESIAN_POINT('Ctrl Pts',(1.24910430528545,-1.10183766688726,12.6680521549019));
#26234=CARTESIAN_POINT('Ctrl Pts',(1.21832909176972,-1.00242421625141,12.6741566408834));
#26235=CARTESIAN_POINT('Ctrl Pts',(1.18753676689898,-0.902955490650669,
12.6802645210257));
#26236=CARTESIAN_POINT('Ctrl Pts',(1.16135691147584,-0.802147923491726,
12.6863724011681));
#26237=CARTESIAN_POINT('Ctrl Pts',(1.13988143393021,-0.700465041616654,
12.6924802813104));
#26238=CARTESIAN_POINT('Ctrl Pts',(1.11837404622141,-0.598631070325962,
12.6985972370811));
#26239=CARTESIAN_POINT('Ctrl Pts',(1.10158506425489,-0.495919606182577,
12.7047141928517));
#26240=CARTESIAN_POINT('Ctrl Pts',(1.0895547535995,-0.392801227887379,12.7108311486224));
#26241=CARTESIAN_POINT('Ctrl Pts',(1.08316572271305,-0.338037346657733,
12.7140797280206));
#26242=CARTESIAN_POINT('Ctrl Pts',(1.07811796237808,-0.28315874308651,12.7173283074189));
#26243=CARTESIAN_POINT('Ctrl Pts',(1.07441152813231,-0.228235845150309,
12.7205768868171));
#26244=CARTESIAN_POINT('Ctrl Pts',(1.06743161727289,-0.124805727059441,
12.726694571124));
#26245=CARTESIAN_POINT('Ctrl Pts',(1.06518963076198,-0.020891687627824,
12.7328122554308));
#26246=CARTESIAN_POINT('Ctrl Pts',(1.06773634292286,0.0830380724030555,
12.7389299397376));
#26247=CARTESIAN_POINT('Ctrl Pts',(1.07027984816573,0.186836960077974,12.7450399204208));
#26248=CARTESIAN_POINT('Ctrl Pts',(1.07760005143083,0.290651107318951,12.7511499011039));
#26249=CARTESIAN_POINT('Ctrl Pts',(1.08969583892884,0.394008666358254,12.7572598817871));
#26250=CARTESIAN_POINT('Ctrl Pts',(1.10177979810024,0.497265153270898,12.7633638875929));
#26251=CARTESIAN_POINT('Ctrl Pts',(1.11863000429741,0.600065519871241,12.7694678933986));
#26252=CARTESIAN_POINT('Ctrl Pts',(1.14019333927317,0.701940239673467,12.7755718992044));
#26253=CARTESIAN_POINT('Ctrl Pts',(1.16174246346846,0.803747821471268,12.7816718823167));
#26254=CARTESIAN_POINT('Ctrl Pts',(1.18799845112701,0.904630555004316,12.7877718654291));
#26255=CARTESIAN_POINT('Ctrl Pts',(1.21885674812158,1.0041271240235,12.7938718485414));
#26256=CARTESIAN_POINT('Ctrl Pts',(1.24970472697017,1.10359042419044,12.799969791991));
#26257=CARTESIAN_POINT('Ctrl Pts',(1.28515183016389,1.20166807570536,12.8060677354407));
#26258=CARTESIAN_POINT('Ctrl Pts',(1.32504330395334,1.29791275030704,12.8121656788904));
#26259=CARTESIAN_POINT('Ctrl Pts',(1.36493160354042,1.39414976662875,12.8182631371209));
#26260=CARTESIAN_POINT('Ctrl Pts',(1.4092634073296,1.4885537036636,12.8243605953514));
#26261=CARTESIAN_POINT('Ctrl Pts',(1.45783569400808,1.58069691012439,12.8304580535819));
#26262=CARTESIAN_POINT('Ctrl Pts',(1.5064164916417,1.67285626214371,12.836556580224));
#26263=CARTESIAN_POINT('Ctrl Pts',(1.55923905039582,1.76275372054627,12.8426551068661));
#26264=CARTESIAN_POINT('Ctrl Pts',(1.61605467255734,1.84998673172291,12.8487536335082));
#26265=CARTESIAN_POINT('Ctrl Pts',(1.67292728220228,1.93730723978136,12.8548582771244));
#26266=CARTESIAN_POINT('Ctrl Pts',(1.73380071967899,2.02195760801406,12.8609629207405));
#26267=CARTESIAN_POINT('Ctrl Pts',(1.79838331220078,2.10356482527697,12.8670675643567));
#26268=CARTESIAN_POINT('Ctrl Pts',(1.86300181767719,2.18521742251265,12.8731756026304));
#26269=CARTESIAN_POINT('Ctrl Pts',(1.93133330827163,2.26382317713033,12.8792836409042));
#26270=CARTESIAN_POINT('Ctrl Pts',(2.00304748164049,2.33904411983918,12.8853916791779));
#26271=CARTESIAN_POINT('Ctrl Pts',(2.07486820335519,2.41437682102814,12.8915087923854));
#26272=CARTESIAN_POINT('Ctrl Pts',(2.15008133734535,2.48631437397807,12.897625905593));
#26273=CARTESIAN_POINT('Ctrl Pts',(2.22832155775466,2.55455741074177,12.9037430188005));
#26274=CARTESIAN_POINT('Ctrl Pts',(2.26985240000642,2.59078162866687,12.9069900554567));
#26275=CARTESIAN_POINT('Ctrl Pts',(2.31223562210947,2.62596557660632,12.9102370921129));
#26276=CARTESIAN_POINT('Ctrl Pts',(2.35541325923941,2.66006943337501,12.9134841287691));
#26277=CARTESIAN_POINT('Ctrl Pts',(2.43676289320398,2.72432344191568,12.9196017688488));
#26278=CARTESIAN_POINT('Ctrl Pts',(2.52119126830436,2.78494389035308,12.9257194089284));
#26279=CARTESIAN_POINT('Ctrl Pts',(2.60834098847442,2.841624099508,12.9318370490081));
#26280=CARTESIAN_POINT('Ctrl Pts',(2.69538095956685,2.89823293034224,12.9379469850429));
#26281=CARTESIAN_POINT('Ctrl Pts',(2.7851351077961,2.95091115840678,12.9440569210777));
#26282=CARTESIAN_POINT('Ctrl Pts',(2.87721368190512,2.99939283310432,12.9501668571124));
#26283=CARTESIAN_POINT('Ctrl Pts',(2.96920220750083,3.047827095005,12.9562708179172));
#26284=CARTESIAN_POINT('Ctrl Pts',(3.06351026360784,3.09207276888496,12.962374778722));
#26285=CARTESIAN_POINT('Ctrl Pts',(3.15972060002561,3.131908104365,12.9684787395268));
#26286=CARTESIAN_POINT('Ctrl Pts',(3.2558675257344,3.17171718500633,12.9745786773077));
#26287=CARTESIAN_POINT('Ctrl Pts',(3.35391384652886,3.20712154625899,12.9806786150886));
#26288=CARTESIAN_POINT('Ctrl Pts',(3.45341999148072,3.23794649985516,12.9867785528696));
#26289=CARTESIAN_POINT('Ctrl Pts',(3.55289286117137,3.26876114546097,12.9928764508064));
#26290=CARTESIAN_POINT('Ctrl Pts',(3.65382417897349,3.29499930205128,12.9989743487432));
#26291=CARTESIAN_POINT('Ctrl Pts',(3.75575751735508,3.31653559180855,13.00507224668));
#26292=CARTESIAN_POINT('Ctrl Pts',(3.85768274271901,3.33807016746225,13.0111696592765));
#26293=CARTESIAN_POINT('Ctrl Pts',(3.96060941417043,3.35490353306712,13.017267071873));
#26294=CARTESIAN_POINT('Ctrl Pts',(4.06407003205697,3.36696124555918,13.0233644844696));
#26295=CARTESIAN_POINT('Ctrl Pts',(4.16754877766877,3.37902107072853,13.0294629654168));
#26296=CARTESIAN_POINT('Ctrl Pts',(4.27156123349589,3.38630353094607,13.035561446364));
#26297=CARTESIAN_POINT('Ctrl Pts',(4.3756347637861,3.38878604688812,13.0416599273112));
#26298=CARTESIAN_POINT('Ctrl Pts',(4.47981268632778,3.39127105294872,13.0477645254157));
#26299=CARTESIAN_POINT('Ctrl Pts',(4.58405138014277,3.38894649161483,13.0538691235202));
#26300=CARTESIAN_POINT('Ctrl Pts',(4.68787826684144,3.38184193345575,13.0599737216247));
#26301=CARTESIAN_POINT('Ctrl Pts',(4.79176289060649,3.37473342452477,13.0660817144336));
#26302=CARTESIAN_POINT('Ctrl Pts',(4.89523482901213,3.36283967216909,13.0721897072425));
#26303=CARTESIAN_POINT('Ctrl Pts',(4.9978285542204,3.3462419234955,13.0782977000514));
#26304=CARTESIAN_POINT('Ctrl Pts',(5.10057471614357,3.32961951340837,13.0844147682921));
#26305=CARTESIAN_POINT('Ctrl Pts',(5.20243964332922,3.30827923643923,13.0905318365328));
#26306=CARTESIAN_POINT('Ctrl Pts',(5.30296983350351,3.2823530555389,13.0966489047735));
#26307=CARTESIAN_POINT('Ctrl Pts',(5.35634027807688,3.26858911260453,13.0998963934227));
#26308=CARTESIAN_POINT('Ctrl Pts',(5.40933481077559,3.25353349967415,13.1031438820719));
#26309=CARTESIAN_POINT('Ctrl Pts',(5.46188777968828,3.23721150892829,13.1063913707211));
#26310=CARTESIAN_POINT('Ctrl Pts',(5.56088732379996,3.20646406161434,13.1125090059837));
#26311=CARTESIAN_POINT('Ctrl Pts',(5.65863159018404,3.17112253339257,13.1186266412464));
#26312=CARTESIAN_POINT('Ctrl Pts',(5.75466552655046,3.13130821171227,13.1247442765091));
#26313=CARTESIAN_POINT('Ctrl Pts',(5.85057852101174,3.09154403084778,13.1308542074279));
#26314=CARTESIAN_POINT('Ctrl Pts',(5.94478507870008,3.04731841852647,13.1369641383468));
#26315=CARTESIAN_POINT('Ctrl Pts',(6.03684543611479,2.99880238068512,13.1430740692656));
#26316=CARTESIAN_POINT('Ctrl Pts',(6.12881575838942,2.95033379158704,13.1491780246647));
#26317=CARTESIAN_POINT('Ctrl Pts',(6.21864368080046,2.89758331959839,13.1552819800638));
#26318=CARTESIAN_POINT('Ctrl Pts',(6.30591033829472,2.84076964775314,13.1613859354628));
#26319=CARTESIAN_POINT('Ctrl Pts',(6.39311947380145,2.78399342475053,13.1674858674278));
#26320=CARTESIAN_POINT('Ctrl Pts',(6.47777034684508,2.72315955986921,13.1735857993927));
#26321=CARTESIAN_POINT('Ctrl Pts',(6.55947027975403,2.65853176144412,13.1796857313577));
#26322=CARTESIAN_POINT('Ctrl Pts',(6.64114288847495,2.59392557750576,13.1857836232269));
#26323=CARTESIAN_POINT('Ctrl Pts',(6.71986618601038,2.52552824588085,13.1918815150961));
#26324=CARTESIAN_POINT('Ctrl Pts',(6.79527862666104,2.45364526563768,13.1979794069653));
#26325=CARTESIAN_POINT('Ctrl Pts',(6.87068506210165,2.38176800954813,13.2040768132498));
#26326=CARTESIAN_POINT('Ctrl Pts',(6.94278085764178,2.30640595036319,13.2101742195344));
#26327=CARTESIAN_POINT('Ctrl Pts',(7.01124021072977,2.22790252615616,13.216271625819));
#26328=CARTESIAN_POINT('Ctrl Pts',(7.07971155618826,2.14938535010799,13.222370100217));
#26329=CARTESIAN_POINT('Ctrl Pts',(7.14454491413589,2.06772603590349,13.228468574615));
#26330=CARTESIAN_POINT('Ctrl Pts',(7.20545434862895,1.98330159065841,13.234567049013));
#26331=CARTESIAN_POINT('Ctrl Pts',(7.26642487592567,1.89879246680648,13.240671640245));
#26332=CARTESIAN_POINT('Ctrl Pts',(7.32346337260496,1.81151301957376,13.246776231477));
#26333=CARTESIAN_POINT('Ctrl Pts',(7.37632694268223,1.7218697039381,13.252880822709));
#26334=CARTESIAN_POINT('Ctrl Pts',(7.42921990801619,1.63217654134226,13.258988808453));
#26335=CARTESIAN_POINT('Ctrl Pts',(7.47793312346699,1.54011726738474,13.2650967941971));
#26336=CARTESIAN_POINT('Ctrl Pts',(7.5222702978688,1.44612174998307,13.2712047799411));
#26337=CARTESIAN_POINT('Ctrl Pts',(7.56667334808656,1.35198657480011,13.2773218408811));
#26338=CARTESIAN_POINT('Ctrl Pts',(7.6066872097305,1.25590980320544,13.2834389018211));
#26339=CARTESIAN_POINT('Ctrl Pts',(7.64216421798083,1.15834006983787,13.2895559627611));
#26340=CARTESIAN_POINT('Ctrl Pts',(7.66099897510223,1.10654026142646,13.2928035127317));
#26341=CARTESIAN_POINT('Ctrl Pts',(7.67855584428645,1.05431990122149,13.2960510627023));
#26342=CARTESIAN_POINT('Ctrl Pts',(7.69481855117705,1.00174744064313,13.299298612673));
#26343=CARTESIAN_POINT('Ctrl Pts',(7.73124472625844,0.883992526509213,13.3065726676388));
#26344=CARTESIAN_POINT('Ctrl Pts',(7.7612676626192,0.764172971569869,13.3138467226047));
#26345=CARTESIAN_POINT('Ctrl Pts',(7.78468903878415,0.642928567549356,13.3211207775705));
#26346=CARTESIAN_POINT('Ctrl Pts',(7.80788532081294,0.52284939840633,13.3283249242992));
#26347=CARTESIAN_POINT('Ctrl Pts',(7.82460627941273,0.401372698938182,13.3355290710279));
#26348=CARTESIAN_POINT('Ctrl Pts',(7.83470626179514,0.27913936157369,13.3427332177567));
#26349=CARTESIAN_POINT('Ctrl Pts',(7.8422997773657,0.187240117062702,13.3481495440715));
#26350=CARTESIAN_POINT('Ctrl Pts',(7.84615168825675,0.0949135788670932,
13.3535658703863));
#26351=CARTESIAN_POINT('Ctrl Pts',(7.84621822868222,0.00243910941253646,
13.3589821967011));
#26352=CARTESIAN_POINT('Ctrl Pts',(7.6353412143218,-1.17693550495398,11.8350241089739));
#26353=CARTESIAN_POINT('Ctrl Pts',(7.59939412479864,-1.27402765636897,11.8406579393705));
#26354=CARTESIAN_POINT('Ctrl Pts',(7.55901381146477,-1.36943260069423,11.8463767776613));
#26355=CARTESIAN_POINT('Ctrl Pts',(7.48271919242755,-1.52891420592338,11.8563684436921));
#26356=CARTESIAN_POINT('Ctrl Pts',(7.44898437731065,-1.59393207582782,11.8605705113664));
#26357=CARTESIAN_POINT('Ctrl Pts',(7.37777340050005,-1.72093732018166,11.8690677127489));
#26358=CARTESIAN_POINT('Ctrl Pts',(7.34036371683698,-1.78291748472974,11.8733589661347));
#26359=CARTESIAN_POINT('Ctrl Pts',(7.23141182631281,-1.95101727885506,11.8854234247197));
#26360=CARTESIAN_POINT('Ctrl Pts',(7.15580663627251,-2.05434823706306,11.8933343672199));
#26361=CARTESIAN_POINT('Ctrl Pts',(6.9237314505997,-2.33653535712539,11.9163500508177));
#26362=CARTESIAN_POINT('Ctrl Pts',(6.75407388599113,-2.50355444928424,11.931795940656));
#26363=CARTESIAN_POINT('Ctrl Pts',(6.50706173627038,-2.70029944414172,11.9516617985081));
#26364=CARTESIAN_POINT('Ctrl Pts',(6.44407945362782,-2.74699000628053,11.956524804522));
#26365=CARTESIAN_POINT('Ctrl Pts',(6.34531078721631,-2.81503267195845,11.963784911166));
#26366=CARTESIAN_POINT('Ctrl Pts',(6.31065742938208,-2.83797782725912,11.9662660369821));
#26367=CARTESIAN_POINT('Ctrl Pts',(6.23512791481641,-2.88601402732262,11.9715212601879));
#26368=CARTESIAN_POINT('Ctrl Pts',(6.19412507662408,-2.91088583940233,11.9742835275195));
#26369=CARTESIAN_POINT('Ctrl Pts',(6.02296686748904,-3.00980221776042,11.9855023245916));
#26370=CARTESIAN_POINT('Ctrl Pts',(5.88849332338007,-3.07605909063025,11.9935928935305));
#26371=CARTESIAN_POINT('Ctrl Pts',(5.59564813971285,-3.19696518230707,12.0105678650837));
#26372=CARTESIAN_POINT('Ctrl Pts',(5.43673052756863,-3.24921549845157,12.0194182542229));
#26373=CARTESIAN_POINT('Ctrl Pts',(5.16297343628663,-3.31730167323249,12.0347829003798));
#26374=CARTESIAN_POINT('Ctrl Pts',(5.05000409631921,-3.33936395396416,12.0411530313047));
#26375=CARTESIAN_POINT('Ctrl Pts',(4.86542865271063,-3.36574793624902,12.0517511978732));
#26376=CARTESIAN_POINT('Ctrl Pts',(4.79442123605421,-3.37361740332017,12.0558724504454));
#26377=CARTESIAN_POINT('Ctrl Pts',(4.64721185745451,-3.38523791809803,12.0645325923212));
#26378=CARTESIAN_POINT('Ctrl Pts',(4.57102606595582,-3.38867140970339,12.0690784597731));
#26379=CARTESIAN_POINT('Ctrl Pts',(4.20637445379349,-3.39279440411933,12.0911712598678));
#26380=CARTESIAN_POINT('Ctrl Pts',(3.91875224933209,-3.35922767031148,12.1097366117395));
#26381=CARTESIAN_POINT('Ctrl Pts',(3.51999442944,-3.26012822152478,12.1359373946312));
#26382=CARTESIAN_POINT('Ctrl Pts',(3.40275317250551,-3.22414458090072,12.1436784140135));
#26383=CARTESIAN_POINT('Ctrl Pts',(3.24406718969492,-3.16585665797537,12.1540035090913));
#26384=CARTESIAN_POINT('Ctrl Pts',(3.20075584311501,-3.14892862338292,12.1568050012285));
#26385=CARTESIAN_POINT('Ctrl Pts',(3.11826335098376,-3.11471392803585,12.1620906774738));
#26386=CARTESIAN_POINT('Ctrl Pts',(3.07903599894315,-3.09756609483025,12.1645804651959));
#26387=CARTESIAN_POINT('Ctrl Pts',(2.9611219389252,-3.04333811757872,12.1720207928299));
#26388=CARTESIAN_POINT('Ctrl Pts',(2.88352299211825,-3.0039661795607,12.1768580591568));
#26389=CARTESIAN_POINT('Ctrl Pts',(2.56983477908364,-2.8293148452143,12.1964960817438));
#26390=CARTESIAN_POINT('Ctrl Pts',(2.34894263725578,-2.66884908466894,12.210608147046));
#26391=CARTESIAN_POINT('Ctrl Pts',(2.07601817461247,-2.41535576104555,12.2310706382502));
#26392=CARTESIAN_POINT('Ctrl Pts',(2.00551506299891,-2.34378154487994,12.23667974451));
#26393=CARTESIAN_POINT('Ctrl Pts',(1.89155580699101,-2.21731819085286,12.2464087645975));
#26394=CARTESIAN_POINT('Ctrl Pts',(1.84643145505943,-2.16402002049441,12.2504588488683));
#26395=CARTESIAN_POINT('Ctrl Pts',(1.75292972627744,-2.04639947403242,12.2593141725608));
#26396=CARTESIAN_POINT('Ctrl Pts',(1.70513306459173,-1.98167212289564,12.2641378871508));
#26397=CARTESIAN_POINT('Ctrl Pts',(1.51596121347347,-1.70543871393861,12.2845467611581));
#26398=CARTESIAN_POINT('Ctrl Pts',(1.39633239272305,-1.48008013236416,12.300863095758));
#26399=CARTESIAN_POINT('Ctrl Pts',(1.26756112844971,-1.15352786223426,12.3233147791539));
#26400=CARTESIAN_POINT('Ctrl Pts',(1.23594445242736,-1.06206553357178,12.3294729747448));
#26401=CARTESIAN_POINT('Ctrl Pts',(1.18872657029609,-0.903847210691334,
12.3397915948604));
#26402=CARTESIAN_POINT('Ctrl Pts',(1.17115733061626,-0.837740332106849,
12.3440059256093));
#26403=CARTESIAN_POINT('Ctrl Pts',(1.1463787369525,-0.731675804999072,12.3505691078849));
#26404=CARTESIAN_POINT('Ctrl Pts',(1.13786661108437,-0.69204464645415,12.3529770085836));
#26405=CARTESIAN_POINT('Ctrl Pts',(1.12009369889256,-0.601406870737667,
12.3583759504963));
#26406=CARTESIAN_POINT('Ctrl Pts',(1.11128813892158,-0.55032354653126,12.3613451447146));
#26407=CARTESIAN_POINT('Ctrl Pts',(1.06453215217256,-0.236202091498968,
12.3792610135361));
#26408=CARTESIAN_POINT('Ctrl Pts',(1.05644910169118,0.0303660499579962,
12.3930626936703));
#26409=CARTESIAN_POINT('Ctrl Pts',(1.09191895413979,0.436166562009752,12.415016004438));
#26410=CARTESIAN_POINT('Ctrl Pts',(1.11306186505697,0.576247973025385,12.4227574877883));
#26411=CARTESIAN_POINT('Ctrl Pts',(1.15848830373778,0.786891539037361,12.4349288004372));
#26412=CARTESIAN_POINT('Ctrl Pts',(1.1764417810872,0.85865899249561,12.4391703511497));
#26413=CARTESIAN_POINT('Ctrl Pts',(1.21661518773907,0.999504326079326,12.4477134786788));
#26414=CARTESIAN_POINT('Ctrl Pts',(1.23873399972851,1.06857004365929,12.4520099754027));
#26415=CARTESIAN_POINT('Ctrl Pts',(1.30552719999954,1.25618935389685,12.4639976465676));
#26416=CARTESIAN_POINT('Ctrl Pts',(1.35465512984795,1.37302261147682,12.4718215591557));
#26417=CARTESIAN_POINT('Ctrl Pts',(1.51479286503673,1.70111972168263,12.4947970005818));
#26418=CARTESIAN_POINT('Ctrl Pts',(1.64169858755669,1.90376616259543,12.5102993430162));
#26419=CARTESIAN_POINT('Ctrl Pts',(1.83730522303411,2.15326804677619,12.5302357786496));
#26420=CARTESIAN_POINT('Ctrl Pts',(1.88793913090982,2.21342229628961,12.5351112721881));
#26421=CARTESIAN_POINT('Ctrl Pts',(1.96856950286904,2.30271569972786,12.5423920715016));
#26422=CARTESIAN_POINT('Ctrl Pts',(1.99708783076453,2.33314989176322,12.5448814009696));
#26423=CARTESIAN_POINT('Ctrl Pts',(2.05971417491399,2.39755857450699,12.55015445583));
#26424=CARTESIAN_POINT('Ctrl Pts',(2.09399765259246,2.43134746031777,12.5529262038059));
#26425=CARTESIAN_POINT('Ctrl Pts',(2.22359553564354,2.55374506318365,12.5630393415191));
#26426=CARTESIAN_POINT('Ctrl Pts',(2.32327505129667,2.6375797846765,12.5701152373717));
#26427=CARTESIAN_POINT('Ctrl Pts',(2.5848749665293,2.833040088811,12.5876670197476));
#26428=CARTESIAN_POINT('Ctrl Pts',(2.75212912853562,2.93669968774034,12.5980235958127));
#26429=CARTESIAN_POINT('Ctrl Pts',(3.02476398440121,3.07449552821056,12.6147137268906));
#26430=CARTESIAN_POINT('Ctrl Pts',(3.12442190893559,3.11896611154662,12.6207731176418));
#26431=CARTESIAN_POINT('Ctrl Pts',(3.29190333729299,3.18420904588795,12.6310095543348));
#26432=CARTESIAN_POINT('Ctrl Pts',(3.35854486819454,3.20779706586694,12.6350952727651));
#26433=CARTESIAN_POINT('Ctrl Pts',(3.49964936771098,3.25282931956057,12.6437965943737));
#26434=CARTESIAN_POINT('Ctrl Pts',(3.57420744985247,3.2738380471302,12.6484229844899));
#26435=CARTESIAN_POINT('Ctrl Pts',(3.89666806233474,3.35288463269726,12.6685793779479));
#26436=CARTESIAN_POINT('Ctrl Pts',(4.14993097592737,3.38544104252741,12.6848614926114));
#26437=CARTESIAN_POINT('Ctrl Pts',(4.5065347992183,3.39091900890328,12.7076852506868));
#26438=CARTESIAN_POINT('Ctrl Pts',(4.60868905497216,3.38787088068285,12.7141992932499));
#26439=CARTESIAN_POINT('Ctrl Pts',(4.7810628131189,3.3749138758117,12.725017599064));
#26440=CARTESIAN_POINT('Ctrl Pts',(4.8513942573988,3.36740853466274,12.7293818736601));
#26441=CARTESIAN_POINT('Ctrl Pts',(4.96185500546183,3.35211195056281,12.7361082266828));
#26442=CARTESIAN_POINT('Ctrl Pts',(5.00216406107272,3.34578646349311,12.7385347970792));
#26443=CARTESIAN_POINT('Ctrl Pts',(5.09247575967662,3.32993845836428,12.7438998099865));
#26444=CARTESIAN_POINT('Ctrl Pts',(5.142395913438,3.32001500209211,12.746818944577));
#26445=CARTESIAN_POINT('Ctrl Pts',(5.37801584642126,3.26763503907511,12.7604545105832));
#26446=CARTESIAN_POINT('Ctrl Pts',(5.56015879023537,3.21069621808778,12.7705858259196));
#26447=CARTESIAN_POINT('Ctrl Pts',(5.86470278742348,3.08649197024779,12.7881558314274));
#26448=CARTESIAN_POINT('Ctrl Pts',(5.9895142863646,3.0264376557331,12.7955535988208));
#26449=CARTESIAN_POINT('Ctrl Pts',(6.20122032760839,2.90810881486592,12.8088433710381));
#26450=CARTESIAN_POINT('Ctrl Pts',(6.28974217509598,2.85313177000169,12.8146465952904));
#26451=CARTESIAN_POINT('Ctrl Pts',(6.43341893650006,2.75445031050719,12.8245917401459));
#26452=CARTESIAN_POINT('Ctrl Pts',(6.48999944734876,2.71294682648828,12.82865468865));
#26453=CARTESIAN_POINT('Ctrl Pts',(6.60742021645467,2.62107721505996,12.8374279275551));
#26454=CARTESIAN_POINT('Ctrl Pts',(6.66786933557167,2.57028091566056,12.8421529970381));
#26455=CARTESIAN_POINT('Ctrl Pts',(6.92442278681109,2.33894088160492,12.8631703412766));
#26456=CARTESIAN_POINT('Ctrl Pts',(7.10059453398932,2.13775607919232,12.8802905622182));
#26457=CARTESIAN_POINT('Ctrl Pts',(7.30368557874387,1.84182351181568,12.9032273525282));
#26458=CARTESIAN_POINT('Ctrl Pts',(7.35286906891361,1.7634693865021,12.9091049078491));
#26459=CARTESIAN_POINT('Ctrl Pts',(7.43180014423054,1.6254937466807,12.919024677382));
#26460=CARTESIAN_POINT('Ctrl Pts',(7.46310890545218,1.56682577365974,12.9231160110645));
#26461=CARTESIAN_POINT('Ctrl Pts',(7.51062329382593,1.47111412955073,12.9295483015617));
#26462=CARTESIAN_POINT('Ctrl Pts',(7.52792616979899,1.43463815450433,12.9319437576622));
#26463=CARTESIAN_POINT('Ctrl Pts',(7.56598182415703,1.35056666294337,12.9373326001084));
#26464=CARTESIAN_POINT('Ctrl Pts',(7.58630027160577,1.30278822334662,12.9403037975482));
#26465=CARTESIAN_POINT('Ctrl Pts',(7.66006920353912,1.11762223201926,12.9515389208032));
#26466=CARTESIAN_POINT('Ctrl Pts',(7.7056385530825,0.977260540281947,12.9594778719187));
#26467=CARTESIAN_POINT('Ctrl Pts',(7.78167456611536,0.677856454243271,12.9760106523204));
#26468=CARTESIAN_POINT('Ctrl Pts',(7.81018681229028,0.51870657280797,12.9845782001725));
#26469=CARTESIAN_POINT('Ctrl Pts',(7.83918761306181,0.245751029150855,12.9995425814277));
#26470=CARTESIAN_POINT('Ctrl Pts',(7.84549940580953,0.13284753890433,13.0058069524936));
#26471=CARTESIAN_POINT('Ctrl Pts',(7.84657713646169,-0.051228267440547,
13.0162761682707));
#26472=CARTESIAN_POINT('Ctrl Pts',(7.84475774865628,-0.122294007574997,
13.0203792879573));
#26473=CARTESIAN_POINT('Ctrl Pts',(7.83635119928191,-0.269513960458309,
13.0290315105716));
#26474=CARTESIAN_POINT('Ctrl Pts',(7.82941958043541,-0.345607415734581,
13.0335885742225));
#26475=CARTESIAN_POINT('Ctrl Pts',(7.79843587348286,-0.592908989731343,
13.0486968707893));
#26476=CARTESIAN_POINT('Ctrl Pts',(7.76386322198776,-0.762505344958133,
13.0595433922846));
#26477=CARTESIAN_POINT('Ctrl Pts',(7.6926492407927,-1.01248795280147,13.0761160301206));
#26478=CARTESIAN_POINT('Ctrl Pts',(7.66556896018746,-1.09529115884783,13.0817024939094));
#26479=CARTESIAN_POINT('Ctrl Pts',(7.63534118037484,-1.17693559664385,13.0872737913614));
#26480=CARTESIAN_POINT('Origin',(4.45646910621825,3.5527136788005E-15,11.));
#26481=CARTESIAN_POINT('',(7.63534122785693,-1.17693546839596,14.6796206134749));
#26482=CARTESIAN_POINT('',(7.63534113152507,-1.17693572858576,14.3356579957882));
#26483=CARTESIAN_POINT('',(7.63534122785693,-1.17693546839596,11.));
#26484=CARTESIAN_POINT('',(7.84621807431328,-0.00264495721902113,14.6089821967061));
#26485=CARTESIAN_POINT('Ctrl Pts',(7.84621807431269,-0.0026449579738531,
14.6089821967504));
#26486=CARTESIAN_POINT('Ctrl Pts',(7.8461078714415,-0.143879742266134,14.6172792981224));
#26487=CARTESIAN_POINT('Ctrl Pts',(7.83716707831609,-0.284765752000311,
14.6255763994944));
#26488=CARTESIAN_POINT('Ctrl Pts',(7.8195478372724,-0.424389574838021,14.6338735008664));
#26489=CARTESIAN_POINT('Ctrl Pts',(7.80838097683225,-0.512881453681321,
14.6391321026897));
#26490=CARTESIAN_POINT('Ctrl Pts',(7.79372905419119,-0.600866932194777,
14.6443907045131));
#26491=CARTESIAN_POINT('Ctrl Pts',(7.77564046454811,-0.688118126881346,
14.6496493063364));
#26492=CARTESIAN_POINT('Ctrl Pts',(7.75459665394175,-0.789623974069688,
14.6557670315438));
#26493=CARTESIAN_POINT('Ctrl Pts',(7.72885907290368,-0.89032385383473,14.6618847567511));
#26494=CARTESIAN_POINT('Ctrl Pts',(7.69850452231244,-0.989753213326928,
14.6680024819585));
#26495=CARTESIAN_POINT('Ctrl Pts',(7.67928914682901,-1.05269509319353,14.671875192464));
#26496=CARTESIAN_POINT('Ctrl Pts',(7.65822466204407,-1.11512790720145,14.6757479029694));
#26497=CARTESIAN_POINT('Ctrl Pts',(7.63534122785692,-1.17693546839596,14.6796206134749));
#26498=CARTESIAN_POINT('Ctrl Pts',(7.63534122785692,-1.17693546839597,13.4294624954408));
#26499=CARTESIAN_POINT('Ctrl Pts',(7.59929922010739,-1.27428399490357,13.4355412195942));
#26500=CARTESIAN_POINT('Ctrl Pts',(7.55880248267084,-1.36991849247735,13.4416199437476));
#26501=CARTESIAN_POINT('Ctrl Pts',(7.51405356222015,-1.46341462235265,13.4476986679009));
#26502=CARTESIAN_POINT('Ctrl Pts',(7.46927795159138,-1.55696651733538,13.4537810176665));
#26503=CARTESIAN_POINT('Ctrl Pts',(7.42024531040631,-1.64837712732693,13.459863367432));
#26504=CARTESIAN_POINT('Ctrl Pts',(7.36720343152648,-1.73724803927718,13.4659457171975));
#26505=CARTESIAN_POINT('Ctrl Pts',(7.31408188775627,-1.82625242861565,13.4720372021924));
#26506=CARTESIAN_POINT('Ctrl Pts',(7.25693932145514,-1.9127091478361,13.4781286871872));
#26507=CARTESIAN_POINT('Ctrl Pts',(7.19606594651401,-1.99625003823206,13.4842201721821));
#26508=CARTESIAN_POINT('Ctrl Pts',(7.16946512903899,-2.03275624442273,13.4868820663297));
#26509=CARTESIAN_POINT('Ctrl Pts',(7.14215239520289,-2.06870609562014,13.4895439604773));
#26510=CARTESIAN_POINT('Ctrl Pts',(7.11415422067151,-2.10407102896113,13.4922058546248));
#26511=CARTESIAN_POINT('Ctrl Pts',(7.04980801601922,-2.18534772918755,13.4983234958086));
#26512=CARTESIAN_POINT('Ctrl Pts',(6.98162835676472,-2.26379847575191,13.5044411369924));
#26513=CARTESIAN_POINT('Ctrl Pts',(6.9098923138079,-2.33904245941807,13.5105587781762));
#26514=CARTESIAN_POINT('Ctrl Pts',(6.83824661186574,-2.41419168433323,13.516668715089));
#26515=CARTESIAN_POINT('Ctrl Pts',(6.76305372283813,-2.48614187112884,13.5227786520018));
#26516=CARTESIAN_POINT('Ctrl Pts',(6.68463159050479,-2.55454438327425,13.5288885889146));
#26517=CARTESIAN_POINT('Ctrl Pts',(6.60628615420595,-2.62287999847009,13.5349925503723));
#26518=CARTESIAN_POINT('Ctrl Pts',(6.52471807458976,-2.68767456155618,13.54109651183));
#26519=CARTESIAN_POINT('Ctrl Pts',(6.4402822431893,-2.74861610634899,13.5472004732877));
#26520=CARTESIAN_POINT('Ctrl Pts',(6.35590206676477,-2.8095174821738,13.5533004113845));
#26521=CARTESIAN_POINT('Ctrl Pts',(6.26865824172616,-2.86657064266844,13.5594003494812));
#26522=CARTESIAN_POINT('Ctrl Pts',(6.17893822835096,-2.9195042705568,13.565500287578));
#26523=CARTESIAN_POINT('Ctrl Pts',(6.08924822078695,-2.97242019541118,13.5715981856216));
#26524=CARTESIAN_POINT('Ctrl Pts',(5.99708403686773,-3.02121911075121,13.5776960836653));
#26525=CARTESIAN_POINT('Ctrl Pts',(5.9028609070006,-3.06567379561648,13.5837939817089));
#26526=CARTESIAN_POINT('Ctrl Pts',(5.80864527971112,-3.11012494074873,13.5898913942035));
#26527=CARTESIAN_POINT('Ctrl Pts',(5.71237141703989,-3.15023236235972,13.5959888066981));
#26528=CARTESIAN_POINT('Ctrl Pts',(5.61447706529752,-3.18581584985841,13.6020862191926));
#26529=CARTESIAN_POINT('Ctrl Pts',(5.5165655644685,-3.22140557085576,13.6081846998291));
#26530=CARTESIAN_POINT('Ctrl Pts',(5.41703340990849,-3.25246963786218,13.6142831804655));
#26531=CARTESIAN_POINT('Ctrl Pts',(5.31633530185756,-3.27887712305551,13.6203816611019));
#26532=CARTESIAN_POINT('Ctrl Pts',(5.2155361925113,-3.3053110952431,13.6264862585806));
#26533=CARTESIAN_POINT('Ctrl Pts',(5.11356920641443,-3.32707905227634,13.6325908560593));
#26534=CARTESIAN_POINT('Ctrl Pts',(5.0109010101027,-3.34410082480404,13.638695453538));
#26535=CARTESIAN_POINT('Ctrl Pts',(4.90817572407401,-3.36113206246515,13.6448034455416));
#26536=CARTESIAN_POINT('Ctrl Pts',(4.80474887296885,-3.37341180815158,13.6509114375451));
#26537=CARTESIAN_POINT('Ctrl Pts',(4.70109217569869,-3.38091180251392,13.6570194295487));
#26538=CARTESIAN_POINT('Ctrl Pts',(4.59728146691846,-3.38842294025135,13.6631364967118));
#26539=CARTESIAN_POINT('Ctrl Pts',(4.4932406545901,-3.39114013356474,13.669253563875));
#26540=CARTESIAN_POINT('Ctrl Pts',(4.38944144750029,-3.38908724518369,13.6753706310381));
#26541=CARTESIAN_POINT('Ctrl Pts',(4.33433550805494,-3.3879973876984,13.678618119551));
#26542=CARTESIAN_POINT('Ctrl Pts',(4.27929758883208,-3.38556399141405,13.681865608064));
#26543=CARTESIAN_POINT('Ctrl Pts',(4.22439740407751,-3.38179653254974,13.6851130965769));
#26544=CARTESIAN_POINT('Ctrl Pts',(4.12097530172035,-3.37469931570006,13.6912307825353));
#26545=CARTESIAN_POINT('Ctrl Pts',(4.01771563058386,-3.36284229879227,13.6973484684937));
#26546=CARTESIAN_POINT('Ctrl Pts',(3.91508915340603,-3.3462386061357,13.7034661544522));
#26547=CARTESIAN_POINT('Ctrl Pts',(3.81259191307791,-3.32965582240041,13.7095761364488));
#26548=CARTESIAN_POINT('Ctrl Pts',(3.71072669758179,-3.30833831589669,13.7156861184454));
#26549=CARTESIAN_POINT('Ctrl Pts',(3.60996085344077,-3.2823511147468,13.721796100442));
#26550=CARTESIAN_POINT('Ctrl Pts',(3.50929355255171,-3.25638932759839,13.7279001072245));
#26551=CARTESIAN_POINT('Ctrl Pts',(3.40972389432364,-3.22576703404182,13.734004114007));
#26552=CARTESIAN_POINT('Ctrl Pts',(3.31170988001849,-3.19060047272148,13.7401081207895));
#26553=CARTESIAN_POINT('Ctrl Pts',(3.2137604675027,-3.15545708995169,13.7462081043742));
#26554=CARTESIAN_POINT('Ctrl Pts',(3.11736505866215,-3.11577553953006,13.7523080879589));
#26555=CARTESIAN_POINT('Ctrl Pts',(3.02296655182748,-3.07172190945976,13.7584080715437));
#26556=CARTESIAN_POINT('Ctrl Pts',(2.92859961403187,-3.02768301193996,13.7645060151532));
#26557=CARTESIAN_POINT('Ctrl Pts',(2.83622863543238,-2.97927512095402,13.7706039587626));
#26558=CARTESIAN_POINT('Ctrl Pts',(2.74627585447121,-2.92671216626761,13.7767019023721));
#26559=CARTESIAN_POINT('Ctrl Pts',(2.65633023574562,-2.8741533967577,13.7827993604501));
#26560=CARTESIAN_POINT('Ctrl Pts',(2.56880279846301,-2.81744043624613,13.7888968185281));
#26561=CARTESIAN_POINT('Ctrl Pts',(2.48408974638786,-2.7568323712941,13.794994276606));
#26562=CARTESIAN_POINT('Ctrl Pts',(2.39936185502347,-2.69621368955298,13.8010928027832));
#26563=CARTESIAN_POINT('Ctrl Pts',(2.31744967407315,-2.63169879489073,13.8071913289604));
#26564=CARTESIAN_POINT('Ctrl Pts',(2.23871835293567,-2.56358862901491,13.8132898551376));
#26565=CARTESIAN_POINT('Ctrl Pts',(2.15990806840072,-2.49541015220486,13.8193944978176));
#26566=CARTESIAN_POINT('Ctrl Pts',(2.08428533522398,-2.4236294831259,13.8254991404976));
#26567=CARTESIAN_POINT('Ctrl Pts',(2.01218021056879,-2.34858614002228,13.8316037831775));
#26568=CARTESIAN_POINT('Ctrl Pts',(1.94003499301122,-2.27350107026686,13.8377118202465));
#26569=CARTESIAN_POINT('Ctrl Pts',(1.87141156017656,-2.1951500321528,13.8438198573155));
#26570=CARTESIAN_POINT('Ctrl Pts',(1.80660001705502,-2.1139060700034,13.8499278943845));
#26571=CARTESIAN_POINT('Ctrl Pts',(1.74169218537689,-2.03254140614763,13.8560450059802));
#26572=CARTESIAN_POINT('Ctrl Pts',(1.68060780208891,-1.94827557919912,13.8621621175758));
#26573=CARTESIAN_POINT('Ctrl Pts',(1.62359398184741,-1.86151110451184,13.8682792291714));
#26574=CARTESIAN_POINT('Ctrl Pts',(1.59333035991995,-1.81545547716486,13.8715262656238));
#26575=CARTESIAN_POINT('Ctrl Pts',(1.5642128977516,-1.76869626324997,13.8747733020763));
#26576=CARTESIAN_POINT('Ctrl Pts',(1.5362731965169,-1.72129628811065,13.8780203385288));
#26577=CARTESIAN_POINT('Ctrl Pts',(1.48363383219249,-1.63199309408694,13.8841378676089));
#26578=CARTESIAN_POINT('Ctrl Pts',(1.43501147634242,-1.54013187947467,13.8902553966891));
#26579=CARTESIAN_POINT('Ctrl Pts',(1.39066155975781,-1.44610827760795,13.8963729257693));
#26580=CARTESIAN_POINT('Ctrl Pts',(1.34636749575522,-1.35220308545513,13.9024827506683));
#26581=CARTESIAN_POINT('Ctrl Pts',(1.3063353522736,-1.25614130243304,13.9085925755673));
#26582=CARTESIAN_POINT('Ctrl Pts',(1.27077582408489,-1.15834510171639,13.9147024004663));
#26583=CARTESIAN_POINT('Ctrl Pts',(1.23525107195512,-1.06064454249481,13.9208062501557));
#26584=CARTESIAN_POINT('Ctrl Pts',(1.20419038018315,-0.961213336674987,
13.9269100998452));
#26585=CARTESIAN_POINT('Ctrl Pts',(1.17775692561686,-0.860494915310985,
13.9330139495347));
#26586=CARTESIAN_POINT('Ctrl Pts',(1.1513408911021,-0.759842868929724,13.9391137766937));
#26587=CARTESIAN_POINT('Ctrl Pts',(1.12954613655457,-0.65790570418471,13.9452136038527));
#26588=CARTESIAN_POINT('Ctrl Pts',(1.11248618679602,-0.555142591693679,
13.9513134310117));
#26589=CARTESIAN_POINT('Ctrl Pts',(1.09543194105117,-0.452413838166731,
13.9574112186866));
#26590=CARTESIAN_POINT('Ctrl Pts',(1.08310942254938,-0.34886010476542,13.9635090063614));
#26591=CARTESIAN_POINT('Ctrl Pts',(1.07558101662333,-0.244950583047285,
13.9696067940362));
#26592=CARTESIAN_POINT('Ctrl Pts',(1.06805320928708,-0.141049323261376,
13.9757040968709));
#26593=CARTESIAN_POINT('Ctrl Pts',(1.06531878676402,-0.0367927553354598,
13.9818013997056));
#26594=CARTESIAN_POINT('Ctrl Pts',(1.06738816919642,0.0673458596739129,
13.9878987025402));
#26595=CARTESIAN_POINT('Ctrl Pts',(1.0694579144371,0.171502732474264,13.9939970743663));
#26596=CARTESIAN_POINT('Ctrl Pts',(1.07633312966777,0.275541186363404,14.0000954461923));
#26597=CARTESIAN_POINT('Ctrl Pts',(1.08797215363175,0.37898989817075,14.0061938180184));
#26598=CARTESIAN_POINT('Ctrl Pts',(1.09962285556094,0.482542404803256,14.0122983086199));
#26599=CARTESIAN_POINT('Ctrl Pts',(1.11604686192597,0.585503564954292,14.0184027992214));
#26600=CARTESIAN_POINT('Ctrl Pts',(1.13715085018088,0.687409177737005,14.0245072898229));
#26601=CARTESIAN_POINT('Ctrl Pts',(1.15826657705757,0.789371473239115,14.0306151759108));
#26602=CARTESIAN_POINT('Ctrl Pts',(1.18406736617564,0.890276640175051,14.0367230619988));
#26603=CARTESIAN_POINT('Ctrl Pts',(1.21440965026856,0.989674464956628,14.0428309480867));
#26604=CARTESIAN_POINT('Ctrl Pts',(1.2447970295493,1.08922001637488,14.0489479118126));
#26605=CARTESIAN_POINT('Ctrl Pts',(1.27973924018433,1.18725335180328,14.0550648755385));
#26606=CARTESIAN_POINT('Ctrl Pts',(1.31904409608155,1.28334304387748,14.0611818392645));
#26607=CARTESIAN_POINT('Ctrl Pts',(1.339918011708,1.33437409536318,14.0644304196699));
#26608=CARTESIAN_POINT('Ctrl Pts',(1.36202158688407,1.38485734260872,14.0676790000753));
#26609=CARTESIAN_POINT('Ctrl Pts',(1.38532083165587,1.43473110308257,14.0709275804807));
#26610=CARTESIAN_POINT('Ctrl Pts',(1.42919782694037,1.52865306383986,14.0770452872358));
#26611=CARTESIAN_POINT('Ctrl Pts',(1.47745655938762,1.62070886166848,14.0831629939909));
#26612=CARTESIAN_POINT('Ctrl Pts',(1.5299152038231,1.71046406535645,14.089280700746));
#26613=CARTESIAN_POINT('Ctrl Pts',(1.58230777925693,1.80010622691829,14.0953907025598));
#26614=CARTESIAN_POINT('Ctrl Pts',(1.63888953601503,1.88745319155252,14.1015007043735));
#26615=CARTESIAN_POINT('Ctrl Pts',(1.69943146028127,1.97209241197929,14.1076107061873));
#26616=CARTESIAN_POINT('Ctrl Pts',(1.75991416835196,2.05664884658965,14.1137147317942));
#26617=CARTESIAN_POINT('Ctrl Pts',(1.82434909401893,2.13850246040086,14.1198187574012));
#26618=CARTESIAN_POINT('Ctrl Pts',(1.89246281734669,2.21726787130628,14.1259227830081));
#26619=CARTESIAN_POINT('Ctrl Pts',(1.96053162936574,2.29598134763066,14.1320227838787));
#26620=CARTESIAN_POINT('Ctrl Pts',(2.03227413749924,2.37161035018557,14.1381227847492));
#26621=CARTESIAN_POINT('Ctrl Pts',(2.10737585959488,2.44380154291802,14.1442227856198));
#26622=CARTESIAN_POINT('Ctrl Pts',(2.18245245420379,2.51596858196682,14.1503207455559));
#26623=CARTESIAN_POINT('Ctrl Pts',(2.26088572236917,2.58469980352577,14.1564187054921));
#26624=CARTESIAN_POINT('Ctrl Pts',(2.34232399418702,2.64967837817621,14.1625166654282));
#26625=CARTESIAN_POINT('Ctrl Pts',(2.42375576872593,2.71465176872935,14.1686141388591));
#26626=CARTESIAN_POINT('Ctrl Pts',(2.50819173768904,2.77587284305098,14.17471161229));
#26627=CARTESIAN_POINT('Ctrl Pts',(2.59524748423437,2.83306532511337,14.1808090857209));
#26628=CARTESIAN_POINT('Ctrl Pts',(2.68231846628117,2.8902678163501,14.1869076262619));
#26629=CARTESIAN_POINT('Ctrl Pts',(2.77200978174592,2.94344008108176,14.1930061668028));
#26630=CARTESIAN_POINT('Ctrl Pts',(2.86390915502518,2.9923498900289,14.1991047073438));
#26631=CARTESIAN_POINT('Ctrl Pts',(2.95590067464842,3.04130874022537,14.2052093628146));
#26632=CARTESIAN_POINT('Ctrl Pts',(3.05010429684792,3.0859964013375,14.2113140182853));
#26633=CARTESIAN_POINT('Ctrl Pts',(3.14608440038722,3.12622727664259,14.2174186737561));
#26634=CARTESIAN_POINT('Ctrl Pts',(3.24211785825333,3.16648051586676,14.2235267227404));
#26635=CARTESIAN_POINT('Ctrl Pts',(3.33992936572046,3.20227188799659,14.2296347717247));
#26636=CARTESIAN_POINT('Ctrl Pts',(3.43906641780329,3.23346514317165,14.235742820709));
#26637=CARTESIAN_POINT('Ctrl Pts',(3.53835073078122,3.26470473366313,14.2418599427568));
#26638=CARTESIAN_POINT('Ctrl Pts',(3.63896410986365,3.29133245872545,14.2479770648045));
#26639=CARTESIAN_POINT('Ctrl Pts',(3.74044204364157,3.31326278887713,14.2540941868523));
#26640=CARTESIAN_POINT('Ctrl Pts',(3.79430504025231,3.32490308598071,14.257341065379));
#26641=CARTESIAN_POINT('Ctrl Pts',(3.84841148040424,3.33522084499568,14.2605879439058));
#26642=CARTESIAN_POINT('Ctrl Pts',(3.90269138321293,3.34420921833594,14.2638348224326));
#26643=CARTESIAN_POINT('Ctrl Pts',(4.00496826297327,3.36114555631361,14.2699527516752));
#26644=CARTESIAN_POINT('Ctrl Pts',(4.1081843232239,3.37341244336819,14.2760706809178));
#26645=CARTESIAN_POINT('Ctrl Pts',(4.21187841710675,3.3809141452128,14.2821886101604));
#26646=CARTESIAN_POINT('Ctrl Pts',(4.31544196361134,3.38840640266697,14.2882988371358));
#26647=CARTESIAN_POINT('Ctrl Pts',(4.41948192640586,3.39114537336765,14.2944090641111));
#26648=CARTESIAN_POINT('Ctrl Pts',(4.52352852080174,3.38908661698337,14.3005192910865));
#26649=CARTESIAN_POINT('Ctrl Pts',(4.62747339020213,3.38702987341829,14.3066235441728));
#26650=CARTESIAN_POINT('Ctrl Pts',(4.73142445543331,3.380184740341,14.3127277972591));
#26651=CARTESIAN_POINT('Ctrl Pts',(4.83490922267138,3.3685587631447,14.3188320503454));
#26652=CARTESIAN_POINT('Ctrl Pts',(4.93832580055099,3.35694044666938,14.324932281148));
#26653=CARTESIAN_POINT('Ctrl Pts',(5.04127627031441,3.34054759880824,14.3310325119505));
#26654=CARTESIAN_POINT('Ctrl Pts',(5.14329134486078,3.31943975318217,14.337132742753));
#26655=CARTESIAN_POINT('Ctrl Pts',(5.24527231194867,3.29833896469909,14.34323093402));
#26656=CARTESIAN_POINT('Ctrl Pts',(5.34631808977652,3.27252639827933,14.349329125287));
#26657=CARTESIAN_POINT('Ctrl Pts',(5.44596846752743,3.24211290310328,14.355427316554));
#26658=CARTESIAN_POINT('Ctrl Pts',(5.54561091307468,3.21170182885169,14.3615250224029));
#26659=CARTESIAN_POINT('Ctrl Pts',(5.64385777313427,3.17669067861854,14.3676227282518));
#26660=CARTESIAN_POINT('Ctrl Pts',(5.74026376159041,3.13724024348438,14.3737204341007));
#26661=CARTESIAN_POINT('Ctrl Pts',(5.83668663355153,3.09778289942652,14.379819207836));
#26662=CARTESIAN_POINT('Ctrl Pts',(5.93126760004852,3.05388488660293,14.3859179815714));
#26663=CARTESIAN_POINT('Ctrl Pts',(6.02358194473019,3.00575488253302,14.3920167553067));
#26664=CARTESIAN_POINT('Ctrl Pts',(6.1159888446647,2.95757662285656,14.3981216437315));
#26665=CARTESIAN_POINT('Ctrl Pts',(6.20612420804209,2.90515809698845,14.4042265321562));
#26666=CARTESIAN_POINT('Ctrl Pts',(6.29358857292772,2.84875360948207,14.4103314205809));
#26667=CARTESIAN_POINT('Ctrl Pts',(6.38110155870265,2.79231776707651,14.4164397026747));
#26668=CARTESIAN_POINT('Ctrl Pts',(6.46594024217969,2.7318917955,14.4225479847684));
#26669=CARTESIAN_POINT('Ctrl Pts',(6.54773630843541,2.66777183271562,14.4286562668622));
#26670=CARTESIAN_POINT('Ctrl Pts',(6.62965384610285,2.60355664845231,14.4347736200725));
#26671=CARTESIAN_POINT('Ctrl Pts',(6.70851942143287,2.53563679506501,14.4408909732828));
#26672=CARTESIAN_POINT('Ctrl Pts',(6.78399975764928,2.46434699852701,14.4470083264931));
#26673=CARTESIAN_POINT('Ctrl Pts',(6.82403372786696,2.42653564613393,14.4502529057902));
#26674=CARTESIAN_POINT('Ctrl Pts',(6.86311603266176,2.38777688581644,14.4534974850874));
#26675=CARTESIAN_POINT('Ctrl Pts',(6.90120154150049,2.34812443928745,14.4567420643846));
#26676=CARTESIAN_POINT('Ctrl Pts',(6.9756608983498,2.27060162927189,14.4630854032313));
#26677=CARTESIAN_POINT('Ctrl Pts',(7.04657001351865,2.18938676520692,14.469428742078));
#26678=CARTESIAN_POINT('Ctrl Pts',(7.11354011887247,2.10484647806263,14.4757720809248));
#26679=CARTESIAN_POINT('Ctrl Pts',(7.17716397400672,2.02453035859624,14.481798466425));
#26680=CARTESIAN_POINT('Ctrl Pts',(7.23723258799101,1.94121348097766,14.4878248519252));
#26681=CARTESIAN_POINT('Ctrl Pts',(7.29344937492137,1.85524877509437,14.4938512374254));
#26682=CARTESIAN_POINT('Ctrl Pts',(7.34961845323007,1.76935702353404,14.4998725086072));
#26683=CARTESIAN_POINT('Ctrl Pts',(7.40194195912083,1.68082227180889,14.5058937797891));
#26684=CARTESIAN_POINT('Ctrl Pts',(7.4501644639003,1.59002929780962,14.5119150509709));
#26685=CARTESIAN_POINT('Ctrl Pts',(7.49835921900135,1.49928857069888,14.5179328572075));
#26686=CARTESIAN_POINT('Ctrl Pts',(7.5424574574542,1.40629258939893,14.5239506634441));
#26687=CARTESIAN_POINT('Ctrl Pts',(7.5822484268014,1.3114528971773,14.5299684696807));
#26688=CARTESIAN_POINT('Ctrl Pts',(7.62202736757881,1.21664187442204,14.5359844567708));
#26689=CARTESIAN_POINT('Ctrl Pts',(7.65750145937001,1.11998865268956,14.5420004438609));
#26690=CARTESIAN_POINT('Ctrl Pts',(7.68850750006142,1.02192606543904,14.548016430951));
#26691=CARTESIAN_POINT('Ctrl Pts',(7.71952301078012,0.923833527399664,14.5540342554754));
#26692=CARTESIAN_POINT('Ctrl Pts',(7.74606760777517,0.824331180515576,14.5600520799997));
#26693=CARTESIAN_POINT('Ctrl Pts',(7.768027719248,0.723867815950181,14.5660699045241));
#26694=CARTESIAN_POINT('Ctrl Pts',(7.78999175642468,0.623386492030765,14.5720888048261));
#26695=CARTESIAN_POINT('Ctrl Pts',(7.80736959523124,0.52194423900002,14.5781077051281));
#26696=CARTESIAN_POINT('Ctrl Pts',(7.8200989427707,0.419999268039994,14.5841266054301));
#26697=CARTESIAN_POINT('Ctrl Pts',(7.83283950703884,0.317964466153722,14.590150809411));
#26698=CARTESIAN_POINT('Ctrl Pts',(7.84092336412678,0.215426498290773,14.5961750133919));
#26699=CARTESIAN_POINT('Ctrl Pts',(7.84434019546452,0.112847441926262,14.6021992173728));
#26700=CARTESIAN_POINT('Ctrl Pts',(7.84562259429113,0.0743476599604382,
14.6044602104839));
#26701=CARTESIAN_POINT('Ctrl Pts',(7.84624810502525,0.0358420830154314,
14.606721203595));
#26702=CARTESIAN_POINT('Ctrl Pts',(7.84621807431328,-0.0026449572190203,
14.6089821967061));
#26703=CARTESIAN_POINT('Ctrl Pts',(7.63534118037484,-1.17693559664385,13.0872737913614));
#26704=CARTESIAN_POINT('Ctrl Pts',(7.61078196418787,-1.24326939326156,13.0918003129721));
#26705=CARTESIAN_POINT('Ctrl Pts',(7.58414505308867,-1.30883829589362,13.0963165266834));
#26706=CARTESIAN_POINT('Ctrl Pts',(7.51900898479892,-1.45579851001032,13.1064781970875));
#26707=CARTESIAN_POINT('Ctrl Pts',(7.47928913008439,-1.53657454578565,13.1120921354455));
#26708=CARTESIAN_POINT('Ctrl Pts',(7.41583733814597,-1.65360387171743,13.1201767496037));
#26709=CARTESIAN_POINT('Ctrl Pts',(7.39455172315452,-1.69113488675286,13.1227614784648));
#26710=CARTESIAN_POINT('Ctrl Pts',(7.34925064900939,-1.76757151201247,13.1279938090185));
#26711=CARTESIAN_POINT('Ctrl Pts',(7.32515342140494,-1.80641768869974,13.1306365108775));
#26712=CARTESIAN_POINT('Ctrl Pts',(7.24845778784824,-1.92464814904058,13.138665454069));
#26713=CARTESIAN_POINT('Ctrl Pts',(7.19329225887402,-2.00231690846836,13.1439200856325));
#26714=CARTESIAN_POINT('Ctrl Pts',(7.00757048412473,-2.24175478279824,13.160387588591));
#26715=CARTESIAN_POINT('Ctrl Pts',(6.86538677605168,-2.39388863739322,13.1712905176747));
#26716=CARTESIAN_POINT('Ctrl Pts',(6.64148260839246,-2.59317858126606,13.1875282510223));
#26717=CARTESIAN_POINT('Ctrl Pts',(6.57034620338852,-2.65148661492758,13.1925667182765));
#26718=CARTESIAN_POINT('Ctrl Pts',(6.43169872917916,-2.75600185095779,13.2022639292715));
#26719=CARTESIAN_POINT('Ctrl Pts',(6.36471464615591,-2.80279784428053,13.2068989017737));
#26720=CARTESIAN_POINT('Ctrl Pts',(6.23765415249025,-2.88489661338535,13.2156449354446));
#26721=CARTESIAN_POINT('Ctrl Pts',(6.17805313344893,-2.9208553645319,13.2197297285821));
#26722=CARTESIAN_POINT('Ctrl Pts',(6.03216555724536,-3.00285594055521,13.2297055909474));
#26723=CARTESIAN_POINT('Ctrl Pts',(5.94491484472188,-3.04704605515623,13.2356546106145));
#26724=CARTESIAN_POINT('Ctrl Pts',(5.6434460138536,-3.18369155678734,13.2561562572981));
#26725=CARTESIAN_POINT('Ctrl Pts',(5.42165239914339,-3.25779183649517,13.2712023388256));
#26726=CARTESIAN_POINT('Ctrl Pts',(5.07646650795671,-3.33474424778458,13.2937557554643));
#26727=CARTESIAN_POINT('Ctrl Pts',(4.95756803085305,-3.35467143186798,13.3013632913643));
#26728=CARTESIAN_POINT('Ctrl Pts',(4.79187773083286,-3.37343251348913,13.3115479624383));
#26729=CARTESIAN_POINT('Ctrl Pts',(4.74579824427791,-3.37769670072365,13.3143358840097));
#26730=CARTESIAN_POINT('Ctrl Pts',(4.66230090379853,-3.38370211587476,13.3192906002656));
#26731=CARTESIAN_POINT('Ctrl Pts',(4.62491588752283,-3.38576912071431,13.3214729899031));
#26732=CARTESIAN_POINT('Ctrl Pts',(4.51088435797457,-3.39018042211444,13.3280391914891));
#26733=CARTESIAN_POINT('Ctrl Pts',(4.4341813645076,-3.39054408842784,13.3323320831021));
#26734=CARTESIAN_POINT('Ctrl Pts',(4.12530267015517,-3.38152450747078,13.3493448430437));
#26735=CARTESIAN_POINT('Ctrl Pts',(3.89438109492653,-3.3508876727214,13.3614774078569));
#26736=CARTESIAN_POINT('Ctrl Pts',(3.53943768799696,-3.26604341622901,13.3812042907396));
#26737=CARTESIAN_POINT('Ctrl Pts',(3.41240719546698,-3.22767971391738,13.3884841856169));
#26738=CARTESIAN_POINT('Ctrl Pts',(3.21929175106573,-3.15676226176972,13.4001246252176));
#26739=CARTESIAN_POINT('Ctrl Pts',(3.15146488721055,-3.12933198239916,13.4043265173063));
#26740=CARTESIAN_POINT('Ctrl Pts',(3.0175015341898,-3.07004210748855,13.4128842679216));
#26741=CARTESIAN_POINT('Ctrl Pts',(2.95140690789296,-3.03818577387404,13.417238239867));
#26742=CARTESIAN_POINT('Ctrl Pts',(2.76702000447868,-2.94182108555106,13.4297828428999));
#26743=CARTESIAN_POINT('Ctrl Pts',(2.65147615423855,-2.87237592559581,13.4381302917912));
#26744=CARTESIAN_POINT('Ctrl Pts',(2.37866539689465,-2.6854361810908,13.4590061915412));
#26745=CARTESIAN_POINT('Ctrl Pts',(2.22687080265957,-2.56080500113723,13.4716830138176));
#26746=CARTESIAN_POINT('Ctrl Pts',(2.01563532629613,-2.35427599483544,13.4904223071858));
#26747=CARTESIAN_POINT('Ctrl Pts',(1.94764818503486,-2.28168920322794,13.4966506267712));
#26748=CARTESIAN_POINT('Ctrl Pts',(1.85413777866381,-2.17261036555619,13.5053955852988));
#26749=CARTESIAN_POINT('Ctrl Pts',(1.82598953162957,-2.13844377800599,13.5080534679178));
#26750=CARTESIAN_POINT('Ctrl Pts',(1.77096178265462,-2.06891924013892,13.5132854149777));
#26751=CARTESIAN_POINT('Ctrl Pts',(1.74409168914495,-2.03356474828833,13.5158587319844));
#26752=CARTESIAN_POINT('Ctrl Pts',(1.65862143537455,-1.91639732272909,13.5241422967821));
#26753=CARTESIAN_POINT('Ctrl Pts',(1.60296463275702,-1.83249712087603,13.5296955889111));
#26754=CARTESIAN_POINT('Ctrl Pts',(1.44716782202941,-1.57328617990728,13.5461222043731));
#26755=CARTESIAN_POINT('Ctrl Pts',(1.35886565655006,-1.39139516313471,13.5567204116079));
#26756=CARTESIAN_POINT('Ctrl Pts',(1.24122107107703,-1.08139971131767,13.5746617927697));
#26757=CARTESIAN_POINT('Ctrl Pts',(1.20218579876288,-0.957539042409238,
13.581795547008));
#26758=CARTESIAN_POINT('Ctrl Pts',(1.15246897373447,-0.761115911058011,
13.5932671517121));
#26759=CARTESIAN_POINT('Ctrl Pts',(1.13687322374893,-0.689924905624793,
13.5974551854113));
#26760=CARTESIAN_POINT('Ctrl Pts',(1.11014802912544,-0.545863097076909,
13.606018670329));
#26761=CARTESIAN_POINT('Ctrl Pts',(1.09907719306723,-0.473021775956921,
13.6103933686582));
#26762=CARTESIAN_POINT('Ctrl Pts',(1.07412122129508,-0.262949999343718,
13.6231567213181));
#26763=CARTESIAN_POINT('Ctrl Pts',(1.06622634454318,-0.125167713253653,
13.6317122703283));
#26764=CARTESIAN_POINT('Ctrl Pts',(1.06771488854485,0.272124175616757,13.6568189481909));
#26765=CARTESIAN_POINT('Ctrl Pts',(1.09846364833005,0.530568255769381,13.6737461673805));
#26766=CARTESIAN_POINT('Ctrl Pts',(1.17159015607771,0.838596312333952,13.6933472274091));
#26767=CARTESIAN_POINT('Ctrl Pts',(1.18620139841751,0.893881103396226,13.6968380644214));
#26768=CARTESIAN_POINT('Ctrl Pts',(1.21340117076398,0.987175531749563,13.7026535808208));
#26769=CARTESIAN_POINT('Ctrl Pts',(1.22527554651082,1.02537487673441,13.7050109413401));
#26770=CARTESIAN_POINT('Ctrl Pts',(1.25674456755835,1.12062722063087,13.7108337075722));
#26771=CARTESIAN_POINT('Ctrl Pts',(1.27719027523242,1.17738248505034,13.7142563416665));
#26772=CARTESIAN_POINT('Ctrl Pts',(1.37565483209962,1.42940394058866,13.7293653938634));
#26773=CARTESIAN_POINT('Ctrl Pts',(1.47022956198287,1.61771441049224,13.7404340956421));
#26774=CARTESIAN_POINT('Ctrl Pts',(1.67155468800349,1.93996060283554,13.760785975133));
#26775=CARTESIAN_POINT('Ctrl Pts',(1.77212765093836,2.07689648618657,13.769969562884));
#26776=CARTESIAN_POINT('Ctrl Pts',(1.93213535107965,2.26361598318493,13.7838052629432));
#26777=CARTESIAN_POINT('Ctrl Pts',(1.98368384144824,2.31981680811819,13.7881615779485));
#26778=CARTESIAN_POINT('Ctrl Pts',(2.08691822265776,2.4250147693373,13.796731899266));
#26779=CARTESIAN_POINT('Ctrl Pts',(2.13833956164798,2.47421550079124,13.8009337757446));
#26780=CARTESIAN_POINT('Ctrl Pts',(2.27586259718405,2.59774722999733,13.8120214511218));
#26781=CARTESIAN_POINT('Ctrl Pts',(2.36421922520013,2.66942347973461,13.8190041824762));
#26782=CARTESIAN_POINT('Ctrl Pts',(2.58796179419694,2.83298501455062,13.8363397563454));
#26783=CARTESIAN_POINT('Ctrl Pts',(2.72671799455055,2.91977372002874,13.8468150722673));
#26784=CARTESIAN_POINT('Ctrl Pts',(2.99843663105924,3.06353933953465,13.8664965580249));
#26785=CARTESIAN_POINT('Ctrl Pts',(3.12985976312979,3.12269837708176,13.8756820254468));
#26786=CARTESIAN_POINT('Ctrl Pts',(3.31335398373097,3.19161386866007,13.8877576643366));
#26787=CARTESIAN_POINT('Ctrl Pts',(3.36247134863246,3.20878182769038,13.8909192229858));
#26788=CARTESIAN_POINT('Ctrl Pts',(3.45036101518317,3.23724887816915,13.8964287401332));
#26789=CARTESIAN_POINT('Ctrl Pts',(3.48897049672086,3.24899682826651,13.8987971818032));
#26790=CARTESIAN_POINT('Ctrl Pts',(3.59154378570079,3.27821662143074,13.9049647483041));
#26791=CARTESIAN_POINT('Ctrl Pts',(3.6558251658698,3.29450610223103,13.9087063445116));
#26792=CARTESIAN_POINT('Ctrl Pts',(3.81040943591592,3.32888670139834,13.9174978846356));
#26793=CARTESIAN_POINT('Ctrl Pts',(3.90105342166349,3.34520475621724,13.9224881702002));
#26794=CARTESIAN_POINT('Ctrl Pts',(4.2676011516645,3.39587978158245,13.9423765631823));
#26795=CARTESIAN_POINT('Ctrl Pts',(4.54656441299923,3.39993331084547,13.956955043098));
#26796=CARTESIAN_POINT('Ctrl Pts',(4.89841967273763,3.36167472098892,13.9768776631696));
#26797=CARTESIAN_POINT('Ctrl Pts',(4.97364734803257,3.3509256440861,13.9812203634815));
#26798=CARTESIAN_POINT('Ctrl Pts',(5.11863902437216,3.32520946985065,13.9897857369685));
#26799=CARTESIAN_POINT('Ctrl Pts',(5.18841699528812,3.31054953273259,13.9939970677708));
#26800=CARTESIAN_POINT('Ctrl Pts',(5.36937046529832,3.26653175542016,14.0051713214528));
#26801=CARTESIAN_POINT('Ctrl Pts',(5.47959899762967,3.23370059869532,14.0122344207196));
#26802=CARTESIAN_POINT('Ctrl Pts',(5.74542376035879,3.13957198013849,14.0298844242536));
#26803=CARTESIAN_POINT('Ctrl Pts',(5.8985622568264,3.0722430424454,14.0406010019327));
#26804=CARTESIAN_POINT('Ctrl Pts',(6.17799358335042,2.92387717791532,14.060850471175));
#26805=CARTESIAN_POINT('Ctrl Pts',(6.30512353791423,2.84520436517367,14.0703627033318));
#26806=CARTESIAN_POINT('Ctrl Pts',(6.46569938650064,2.73051287052803,14.082446919164));
#26807=CARTESIAN_POINT('Ctrl Pts',(6.50414640408515,2.70180033828092,14.0853452345017));
#26808=CARTESIAN_POINT('Ctrl Pts',(6.57492556085352,2.64656277872113,14.0906711249749));
#26809=CARTESIAN_POINT('Ctrl Pts',(6.60739967357696,2.62023855722424,14.0931088165143));
#26810=CARTESIAN_POINT('Ctrl Pts',(6.70000469248057,2.54228886728828,14.100066552028));
#26811=CARTESIAN_POINT('Ctrl Pts',(6.75882614837989,2.48914411900959,14.1044953466474));
#26812=CARTESIAN_POINT('Ctrl Pts',(6.9899088925653,2.26515505759865,14.1221821276839));
#26813=CARTESIAN_POINT('Ctrl Pts',(7.14546472943476,2.07811434792671,14.1348228197469));
#26814=CARTESIAN_POINT('Ctrl Pts',(7.34801936292616,1.77329282884427,14.1546774779979));
#26815=CARTESIAN_POINT('Ctrl Pts',(7.41064253472399,1.66687904799674,14.1614807233479));
#26816=CARTESIAN_POINT('Ctrl Pts',(7.50049269678464,1.49316391094426,14.1725706555008));
#26817=CARTESIAN_POINT('Ctrl Pts',(7.53160355190887,1.42799339733243,14.1767267002323));
#26818=CARTESIAN_POINT('Ctrl Pts',(7.5905380079332,1.29366406403061,14.1853113003037));
#26819=CARTESIAN_POINT('Ctrl Pts',(7.61820874850869,1.2244818380462,14.1897419755079));
#26820=CARTESIAN_POINT('Ctrl Pts',(7.69371447104145,1.01603168115716,14.2031388340943));
#26821=CARTESIAN_POINT('Ctrl Pts',(7.7347765606307,0.874511207641564,14.2123028973801));
#26822=CARTESIAN_POINT('Ctrl Pts',(7.80982716998081,0.534574062973371,14.2343667223056));
#26823=CARTESIAN_POINT('Ctrl Pts',(7.83561314585523,0.334907602015024,14.2473786631015));
#26824=CARTESIAN_POINT('Ctrl Pts',(7.8468295138858,0.0516807095146062,14.2652453393694));
#26825=CARTESIAN_POINT('Ctrl Pts',(7.84708312737092,-0.0308724860350004,
14.2703782550505));
#26826=CARTESIAN_POINT('Ctrl Pts',(7.84289991434231,-0.155893278208164,
14.2779649048766));
#26827=CARTESIAN_POINT('Ctrl Pts',(7.84067564013924,-0.198401320532778,
14.2805113548649));
#26828=CARTESIAN_POINT('Ctrl Pts',(7.83434283382549,-0.287300981476298,
14.28575333076));
#26829=CARTESIAN_POINT('Ctrl Pts',(7.83007794313444,-0.333671503058707,
14.2884413932368));
#26830=CARTESIAN_POINT('Ctrl Pts',(7.81091591323208,-0.503553200940941,
14.2981660767072));
#26831=CARTESIAN_POINT('Ctrl Pts',(7.7901779705527,-0.626314399420544,14.3049552114575));
#26832=CARTESIAN_POINT('Ctrl Pts',(7.72974380590606,-0.893561105008769,
14.3197127536322));
#26833=CARTESIAN_POINT('Ctrl Pts',(7.68716662343717,-1.03695645662067,14.3276212883842));
#26834=CARTESIAN_POINT('Ctrl Pts',(7.63534113152507,-1.17693572858576,14.3356579957882));
#26835=CARTESIAN_POINT('Origin',(4.45646910621825,3.5527136788005E-15,11.));
#26836=CARTESIAN_POINT('',(7.63534122786267,-1.17693546838044,15.9331819277137));
#26837=CARTESIAN_POINT('',(7.63534118765004,-1.1769355769937,15.5865253037982));
#26838=CARTESIAN_POINT('',(7.63534122785693,-1.17693546839596,11.));
#26839=CARTESIAN_POINT('',(7.84621680191345,0.00395247126457767,15.8589808168116));
#26840=CARTESIAN_POINT('Ctrl Pts',(7.84621673818046,0.00400675761810125,
15.8598626507015));
#26841=CARTESIAN_POINT('Ctrl Pts',(7.84635597463948,-0.113788353100374,
15.8674415510758));
#26842=CARTESIAN_POINT('Ctrl Pts',(7.84035501031268,-0.231516686720479,
15.8749656324585));
#26843=CARTESIAN_POINT('Ctrl Pts',(7.81594889922953,-0.46751264752174,15.8898584151366));
#26844=CARTESIAN_POINT('Ctrl Pts',(7.79738934461118,-0.585601546171405,
15.8972129536422));
#26845=CARTESIAN_POINT('Ctrl Pts',(7.75665422830044,-0.777899395116433,
15.9090356595868));
#26846=CARTESIAN_POINT('Ctrl Pts',(7.73810725094379,-0.852761209403362,
15.9136000387725));
#26847=CARTESIAN_POINT('Ctrl Pts',(7.69333519420788,-1.01025069608165,15.9231472973591));
#26848=CARTESIAN_POINT('Ctrl Pts',(7.66646200780271,-1.09263703021642,15.9281085052823));
#26849=CARTESIAN_POINT('Ctrl Pts',(7.63608789069674,-1.17491727604896,15.9330604654293));
#26850=CARTESIAN_POINT('Ctrl Pts',(7.63571479859986,-1.1759264635252,15.9331212021678));
#26851=CARTESIAN_POINT('Ctrl Pts',(7.63534122786842,-1.17693546836491,15.9331819277137));
#26852=CARTESIAN_POINT('Ctrl Pts',(7.63534122785692,-1.17693546839596,14.6796206134749));
#26853=CARTESIAN_POINT('Ctrl Pts',(7.59925654215824,-1.27439926693538,14.6857274565409));
#26854=CARTESIAN_POINT('Ctrl Pts',(7.55864642848513,-1.37030743254935,14.6918342996069));
#26855=CARTESIAN_POINT('Ctrl Pts',(7.51367023832885,-1.46421525067923,14.697941142673));
#26856=CARTESIAN_POINT('Ctrl Pts',(7.46873004583586,-1.55804790766262,14.7040430979955));
#26857=CARTESIAN_POINT('Ctrl Pts',(7.41943091115226,-1.64988302006714,14.710145053318));
#26858=CARTESIAN_POINT('Ctrl Pts',(7.36598036809627,-1.7392956274035,14.7162470086406));
#26859=CARTESIAN_POINT('Ctrl Pts',(7.31255275719406,-1.82866987360182,14.7223463460107));
#26860=CARTESIAN_POINT('Ctrl Pts',(7.25497749599115,-1.91562331656183,14.7284456833808));
#26861=CARTESIAN_POINT('Ctrl Pts',(7.19350781112107,-1.99975603271096,14.7345450207509));
#26862=CARTESIAN_POINT('Ctrl Pts',(7.13204884861661,-2.08387407330507,14.740643294193));
#26863=CARTESIAN_POINT('Ctrl Pts',(7.06669706390409,-2.16517202256828,14.746741567635));
#26864=CARTESIAN_POINT('Ctrl Pts',(6.9977482079261,-2.24328009613667,14.752839841077));
#26865=CARTESIAN_POINT('Ctrl Pts',(6.92879382502816,-2.32139443082518,14.7589386033549));
#26866=CARTESIAN_POINT('Ctrl Pts',(6.85624207946546,-2.3963180635243,14.7650373656327));
#26867=CARTESIAN_POINT('Ctrl Pts',(6.78042749679774,-2.46771604147543,14.7711361279105));
#26868=CARTESIAN_POINT('Ctrl Pts',(6.70454113290327,-2.53918161901314,14.7772406644949));
#26869=CARTESIAN_POINT('Ctrl Pts',(6.62538607070449,-2.60711458175522,14.7833452010792));
#26870=CARTESIAN_POINT('Ctrl Pts',(6.54333202014636,-2.67121849367877,14.7894497376635));
#26871=CARTESIAN_POINT('Ctrl Pts',(6.4612393624972,-2.73535256700868,14.7955571464815));
#26872=CARTESIAN_POINT('Ctrl Pts',(6.3762453448536,-2.79565375292429,14.8016645552994));
#26873=CARTESIAN_POINT('Ctrl Pts',(6.28874935509067,-2.85186853695818,14.8077719641173));
#26874=CARTESIAN_POINT('Ctrl Pts',(6.20111478934914,-2.90817235385781,14.8138890458374));
#26875=CARTESIAN_POINT('Ctrl Pts',(6.11097070112765,-2.96037662220921,14.8200061275576));
#26876=CARTESIAN_POINT('Ctrl Pts',(6.01874207763718,-3.00827329630701,14.8261232092777));
#26877=CARTESIAN_POINT('Ctrl Pts',(5.93615235562846,-3.05116424327304,14.831600988948));
#26878=CARTESIAN_POINT('Ctrl Pts',(5.85189155830507,-3.09060148796669,14.8370787686182));
#26879=CARTESIAN_POINT('Ctrl Pts',(5.76627707734561,-3.12646895734968,14.8425565482884));
#26880=CARTESIAN_POINT('Ctrl Pts',(5.67063788999286,-3.16653619347313,14.8486757280147));
#26881=CARTESIAN_POINT('Ctrl Pts',(5.57300807714975,-3.20227406034225,14.8547949077409));
#26882=CARTESIAN_POINT('Ctrl Pts',(5.47381452586385,-3.23348316210648,14.8609140874672));
#26883=CARTESIAN_POINT('Ctrl Pts',(5.37474561246936,-3.2646530492586,14.8670255783704));
#26884=CARTESIAN_POINT('Ctrl Pts',(5.27411726975106,-3.29130535986388,14.8731370692736));
#26885=CARTESIAN_POINT('Ctrl Pts',(5.17237659623641,-3.31328862736645,14.8792485601769));
#26886=CARTESIAN_POINT('Ctrl Pts',(5.07073518188626,-3.33525044778508,14.8853540886517));
#26887=CARTESIAN_POINT('Ctrl Pts',(4.96798400832247,-3.35255219560697,14.8914596171266));
#26888=CARTESIAN_POINT('Ctrl Pts',(4.86458477785658,-3.3650923703612,14.8975651456014));
#26889=CARTESIAN_POINT('Ctrl Pts',(4.76125347176171,-3.37762430730284,14.9036666632709));
#26890=CARTESIAN_POINT('Ctrl Pts',(4.65727537604443,-3.38540084126951,14.9097681809405));
#26891=CARTESIAN_POINT('Ctrl Pts',(4.55312104360974,-3.38837180154399,14.91586969861));
#26892=CARTESIAN_POINT('Ctrl Pts',(4.44900141669852,-3.39134177185742,14.9219691831777));
#26893=CARTESIAN_POINT('Ctrl Pts',(4.34470609398513,-3.3895093396803,14.9280686677454));
#26894=CARTESIAN_POINT('Ctrl Pts',(4.24070861432847,-3.38287636082661,14.9341681523131));
#26895=CARTESIAN_POINT('Ctrl Pts',(4.13671933112334,-3.37624390474414,14.9402671561564));
#26896=CARTESIAN_POINT('Ctrl Pts',(4.03302826812358,-3.36481168187265,14.9463661599996));
#26897=CARTESIAN_POINT('Ctrl Pts',(3.93010594542762,-3.34863358483165,14.9524651638429));
#26898=CARTESIAN_POINT('Ctrl Pts',(3.82716555195804,-3.3324526472919,14.9585652385299));
#26899=CARTESIAN_POINT('Ctrl Pts',(3.72499458654479,-3.31152424580401,14.9646653132168));
#26900=CARTESIAN_POINT('Ctrl Pts',(3.62405458660875,-3.28595361045211,14.9707653879037));
#26901=CARTESIAN_POINT('Ctrl Pts',(3.52301346137032,-3.26035735752309,14.9768715738637));
#26902=CARTESIAN_POINT('Ctrl Pts',(3.42320617622278,-3.23010968941689,14.9829777598236));
#26903=CARTESIAN_POINT('Ctrl Pts',(3.32508020856909,-3.19536605489515,14.9890839457836));
#26904=CARTESIAN_POINT('Ctrl Pts',(3.22689971002588,-3.16060311252513,14.9951935250935));
#26905=CARTESIAN_POINT('Ctrl Pts',(3.13040278355711,-3.12133938647638,15.0013031044034));
#26906=CARTESIAN_POINT('Ctrl Pts',(3.03601624188276,-3.07777821207134,15.0074126837134));
#26907=CARTESIAN_POINT('Ctrl Pts',(2.94148975664343,-3.03415245106389,15.0135313214791));
#26908=CARTESIAN_POINT('Ctrl Pts',(2.84908028160397,-2.98621671291607,15.0196499592447));
#26909=CARTESIAN_POINT('Ctrl Pts',(2.75918943086372,-2.93421995871618,15.0257685970104));
#26910=CARTESIAN_POINT('Ctrl Pts',(2.71171104319487,-2.90675640671846,15.029000328087));
#26911=CARTESIAN_POINT('Ctrl Pts',(2.66493479381262,-2.87816067354097,15.0322320591637));
#26912=CARTESIAN_POINT('Ctrl Pts',(2.61891630898795,-2.84847411430946,15.0354637902403));
#26913=CARTESIAN_POINT('Ctrl Pts',(2.53190268614322,-2.79234156065477,15.0415744788063));
#26914=CARTESIAN_POINT('Ctrl Pts',(2.447324003263,-2.73212835339743,15.0476851673722));
#26915=CARTESIAN_POINT('Ctrl Pts',(2.36558555678323,-2.66807253372205,15.0537958559381));
#26916=CARTESIAN_POINT('Ctrl Pts',(2.28395036483308,-2.60409763133609,15.0598988252936));
#26917=CARTESIAN_POINT('Ctrl Pts',(2.20514860836062,-2.53629002873644,15.066001794649));
#26918=CARTESIAN_POINT('Ctrl Pts',(2.12955756925958,-2.46493159370978,15.0721047640044));
#26919=CARTESIAN_POINT('Ctrl Pts',(2.0540406049299,-2.39364308575148,15.0782017528089));
#26920=CARTESIAN_POINT('Ctrl Pts',(1.98172840905519,-2.3188109566093,15.0842987416134));
#26921=CARTESIAN_POINT('Ctrl Pts',(1.91296537712471,-2.24075742609218,15.0903957304179));
#26922=CARTESIAN_POINT('Ctrl Pts',(1.84424747924138,-2.16275512763431,15.0964887173369));
#26923=CARTESIAN_POINT('Ctrl Pts',(1.77907439344342,-2.08153595168046,15.1025817042559));
#26924=CARTESIAN_POINT('Ctrl Pts',(1.71775323376058,-1.99745849329803,15.1086746911749));
#26925=CARTESIAN_POINT('Ctrl Pts',(1.65645243872213,-1.91340895688494,15.1147656546242));
#26926=CARTESIAN_POINT('Ctrl Pts',(1.5990012778261,-1.82650336887972,15.1208566180734));
#26927=CARTESIAN_POINT('Ctrl Pts',(1.54566567361456,-1.73713224575521,15.1269475815227));
#26928=CARTESIAN_POINT('Ctrl Pts',(1.49233409906925,-1.64776787488939,15.1330380847812));
#26929=CARTESIAN_POINT('Ctrl Pts',(1.44311768089322,-1.55593870543276,15.1391285880398));
#26930=CARTESIAN_POINT('Ctrl Pts',(1.39823773191259,-1.46206221608812,15.1452190912983));
#26931=CARTESIAN_POINT('Ctrl Pts',(1.35334966028844,-1.36816873641094,15.1513106968528));
#26932=CARTESIAN_POINT('Ctrl Pts',(1.3127998010773,-1.27222758501815,15.1574023024073));
#26933=CARTESIAN_POINT('Ctrl Pts',(1.27676205110674,-1.17467787336532,15.1634939079618));
#26934=CARTESIAN_POINT('Ctrl Pts',(1.24068756600035,-1.07702872426397,15.1695917230038));
#26935=CARTESIAN_POINT('Ctrl Pts',(1.20913452112613,-0.977768141438918,
15.1756895380458));
#26936=CARTESIAN_POINT('Ctrl Pts',(1.18222744528331,-0.877352043536669,
15.1817873530878));
#26937=CARTESIAN_POINT('Ctrl Pts',(1.15530519760434,-0.776879324967353,
15.1878886064466));
#26938=CARTESIAN_POINT('Ctrl Pts',(1.13303422816773,-0.675250209564502,
15.1939898598054));
#26939=CARTESIAN_POINT('Ctrl Pts',(1.11548787895925,-0.572930625471287,
15.2000911131641));
#26940=CARTESIAN_POINT('Ctrl Pts',(1.09791505400747,-0.470456651025431,
15.2062015727239));
#26941=CARTESIAN_POINT('Ctrl Pts',(1.08508113806529,-0.367290549925763,
15.2123120322837));
#26942=CARTESIAN_POINT('Ctrl Pts',(1.07700758983372,-0.263903243208449,
15.2184224918435));
#26943=CARTESIAN_POINT('Ctrl Pts',(1.07262603066434,-0.207794381435347,
15.2217386719598));
#26944=CARTESIAN_POINT('Ctrl Pts',(1.06964563234854,-0.151620379755214,
15.225054852076));
#26945=CARTESIAN_POINT('Ctrl Pts',(1.0680634074785,-0.0954561849645197,
15.2283710321923));
#26946=CARTESIAN_POINT('Ctrl Pts',(1.06513996899317,0.00831703441671776,
15.2344982576959));
#26947=CARTESIAN_POINT('Ctrl Pts',(1.06698351873962,0.112386429627051,15.2406254831995));
#26948=CARTESIAN_POINT('Ctrl Pts',(1.0736259808533,0.216280955405394,15.2467527087032));
#26949=CARTESIAN_POINT('Ctrl Pts',(1.08026006332207,0.320044415440628,15.2528722045468));
#26950=CARTESIAN_POINT('Ctrl Pts',(1.09168099275754,0.423633025198743,15.2589917003904));
#26951=CARTESIAN_POINT('Ctrl Pts',(1.1078686999171,0.526574193651555,15.265111196234));
#26952=CARTESIAN_POINT('Ctrl Pts',(1.12404049789571,0.629414192144985,15.271224677874));
#26953=CARTESIAN_POINT('Ctrl Pts',(1.14496969006219,0.731607598516677,15.277338159514));
#26954=CARTESIAN_POINT('Ctrl Pts',(1.17058433753088,0.83268622506223,15.283451641154));
#26955=CARTESIAN_POINT('Ctrl Pts',(1.19618171898921,0.933696717755195,15.2895610018925));
#26956=CARTESIAN_POINT('Ctrl Pts',(1.22645816970146,1.03359351584041,15.2956703626311));
#26957=CARTESIAN_POINT('Ctrl Pts',(1.26129068445046,1.13191868770221,15.3017797233697));
#26958=CARTESIAN_POINT('Ctrl Pts',(1.29611119508855,1.23020997437724,15.3078869786776));
#26959=CARTESIAN_POINT('Ctrl Pts',(1.33548450685337,1.32693031283058,15.3139942339855));
#26960=CARTESIAN_POINT('Ctrl Pts',(1.37923800531681,1.42163772253867,15.3201014892935));
#26961=CARTESIAN_POINT('Ctrl Pts',(1.42298747046021,1.51633640185244,15.3262081816175));
#26962=CARTESIAN_POINT('Ctrl Pts',(1.47111614124288,1.60902213721648,15.3323148739415));
#26963=CARTESIAN_POINT('Ctrl Pts',(1.52340393979046,1.69927448988912,15.3384215662655));
#26964=CARTESIAN_POINT('Ctrl Pts',(1.57570011738232,1.78954130537107,15.3445292371782));
#26965=CARTESIAN_POINT('Ctrl Pts',(1.63215653474165,1.8773735969273,15.3506369080909));
#26966=CARTESIAN_POINT('Ctrl Pts',(1.69250844011902,1.96237776657714,15.3567445790035));
#26967=CARTESIAN_POINT('Ctrl Pts',(1.75291890778438,2.04746441976471,15.3628581764761));
#26968=CARTESIAN_POINT('Ctrl Pts',(1.81723216529803,2.12971712583411,15.3689717739487));
#26969=CARTESIAN_POINT('Ctrl Pts',(1.88514165812614,2.20877346443409,15.3750853714212));
#26970=CARTESIAN_POINT('Ctrl Pts',(1.95308777961948,2.28787244402635,15.3812022664139));
#26971=CARTESIAN_POINT('Ctrl Pts',(2.02463371065202,2.36377131310707,15.3873191614065));
#26972=CARTESIAN_POINT('Ctrl Pts',(2.09943561816621,2.43614412519072,15.3934360563991));
#26973=CARTESIAN_POINT('Ctrl Pts',(2.17434565711162,2.50862155727688,15.3995617937948));
#26974=CARTESIAN_POINT('Ctrl Pts',(2.25252075476105,2.5775624729625,15.4056875311904));
#26975=CARTESIAN_POINT('Ctrl Pts',(2.33358354254727,2.64268082561201,15.411813268586));
#26976=CARTESIAN_POINT('Ctrl Pts',(2.3753341480884,2.67621940390675,15.4149682704387));
#26977=CARTESIAN_POINT('Ctrl Pts',(2.41785027223247,2.70874467938232,15.4181232722915));
#26978=CARTESIAN_POINT('Ctrl Pts',(2.46107751393011,2.74022215448416,15.4212782741442));
#26979=CARTESIAN_POINT('Ctrl Pts',(2.54498702904448,2.80132389424574,15.427402529712));
#26980=CARTESIAN_POINT('Ctrl Pts',(2.63183486823323,2.85866212129903,15.4335267852798));
#26981=CARTESIAN_POINT('Ctrl Pts',(2.72125043459067,2.91194457779249,15.4396510408476));
#26982=CARTESIAN_POINT('Ctrl Pts',(2.81055518966647,2.96516100218959,15.4457677067234));
#26983=CARTESIAN_POINT('Ctrl Pts',(2.90242098265036,3.01433143556791,15.4518843725992));
#26984=CARTESIAN_POINT('Ctrl Pts',(2.9964465891759,3.05920566687324,15.458001038475));
#26985=CARTESIAN_POINT('Ctrl Pts',(3.09038192539221,3.10403681618329,15.464111831979));
#26986=CARTESIAN_POINT('Ctrl Pts',(3.18647257007655,3.14457978562317,15.470222625483));
#26987=CARTESIAN_POINT('Ctrl Pts',(3.28429165528187,3.18062966816578,15.476333418987));
#26988=CARTESIAN_POINT('Ctrl Pts',(3.38204828979246,3.21665653536117,15.4824403111737));
#26989=CARTESIAN_POINT('Ctrl Pts',(3.48153077341354,3.24819587466238,15.4885472033603));
#26990=CARTESIAN_POINT('Ctrl Pts',(3.58229186616218,3.27509071866231,15.4946540955469));
#26991=CARTESIAN_POINT('Ctrl Pts',(3.683020481052,3.30197689377107,15.500759019327));
#26992=CARTESIAN_POINT('Ctrl Pts',(3.78502647661581,3.32422144061892,15.5068639431072));
#26993=CARTESIAN_POINT('Ctrl Pts',(3.8878477862843,3.34171735145518,15.5129688668874));
#26994=CARTESIAN_POINT('Ctrl Pts',(3.99066195666558,3.35921204748166,15.5190733667788));
#26995=CARTESIAN_POINT('Ctrl Pts',(4.09429091070886,3.37195869258122,15.5251778666701));
#26996=CARTESIAN_POINT('Ctrl Pts',(4.19826358574929,3.37990162160075,15.5312823665615));
#26997=CARTESIAN_POINT('Ctrl Pts',(4.30225533447414,3.38784600774275,15.5373879863173));
#26998=CARTESIAN_POINT('Ctrl Pts',(4.40659050696824,3.3909848943031,15.5434936060731));
#26999=CARTESIAN_POINT('Ctrl Pts',(4.51079499737456,3.38931464459264,15.5495992258289));
#27000=CARTESIAN_POINT('Ctrl Pts',(4.61510446294567,3.38764271227964,15.5557109963604));
#27001=CARTESIAN_POINT('Ctrl Pts',(4.71928255921592,3.38115197747714,15.5618227668918));
#27002=CARTESIAN_POINT('Ctrl Pts',(4.82285732306245,3.36989090877698,15.5679345374233));
#27003=CARTESIAN_POINT('Ctrl Pts',(4.92649008825309,3.35862353393528,15.5740497305153));
#27004=CARTESIAN_POINT('Ctrl Pts',(5.02951842934428,3.34258056854254,15.5801649236074));
#27005=CARTESIAN_POINT('Ctrl Pts',(5.13147947861677,3.3218618363283,15.5862801166994));
#27006=CARTESIAN_POINT('Ctrl Pts',(5.23359142989047,3.30111244046186,15.5924043602562));
#27007=CARTESIAN_POINT('Ctrl Pts',(5.33463252415536,3.27567356157461,15.5985286038129));
#27008=CARTESIAN_POINT('Ctrl Pts',(5.43415391523411,3.24569522240146,15.6046528473696));
#27009=CARTESIAN_POINT('Ctrl Pts',(5.48579046667504,3.23014099796741,15.6078304036118));
#27010=CARTESIAN_POINT('Ctrl Pts',(5.5370182091448,3.2133655359543,15.611007959854));
#27011=CARTESIAN_POINT('Ctrl Pts',(5.58777668886605,3.19539484507684,15.6141855160962));
#27012=CARTESIAN_POINT('Ctrl Pts',(5.68459211532516,3.16111800876059,15.6202463056308));
#27013=CARTESIAN_POINT('Ctrl Pts',(5.78001811340089,3.12237696064005,15.6263070951653));
#27014=CARTESIAN_POINT('Ctrl Pts',(5.87361055453002,3.0793043334456,15.6323678846999));
#27015=CARTESIAN_POINT('Ctrl Pts',(5.967083541579,3.03628668078754,15.6384209387162));
#27016=CARTESIAN_POINT('Ctrl Pts',(6.05872723190476,2.98894861657474,15.6444739927325));
#27017=CARTESIAN_POINT('Ctrl Pts',(6.14811421064749,2.93747202593669,15.6505270467488));
#27018=CARTESIAN_POINT('Ctrl Pts',(6.23741355706659,2.8860459014103,15.6565741665318));
#27019=CARTESIAN_POINT('Ctrl Pts',(6.32446021598998,2.83048953163787,15.6626212863147));
#27020=CARTESIAN_POINT('Ctrl Pts',(6.40884914271364,2.77103180342527,15.6686684060977));
#27021=CARTESIAN_POINT('Ctrl Pts',(6.49318591791259,2.71161081950249,15.6747117888203));
#27022=CARTESIAN_POINT('Ctrl Pts',(6.57486787119696,2.64829351790517,15.6807551715428));
#27023=CARTESIAN_POINT('Ctrl Pts',(6.65351760202964,2.58135293393851,15.6867985542654));
#27024=CARTESIAN_POINT('Ctrl Pts',(6.73214331204496,2.51443279463865,15.6928400912475));
#27025=CARTESIAN_POINT('Ctrl Pts',(6.8077383092479,2.44389185254269,15.6988816282296));
#27026=CARTESIAN_POINT('Ctrl Pts',(6.87995779939702,2.37004380055194,15.7049231652116));
#27027=CARTESIAN_POINT('Ctrl Pts',(6.95217457789299,2.29619852136258,15.7109644753498));
#27028=CARTESIAN_POINT('Ctrl Pts',(7.02101579796853,2.21904668959344,15.7170057854879));
#27029=CARTESIAN_POINT('Ctrl Pts',(7.0861738280999,2.13893855409952,15.7230470956261));
#27030=CARTESIAN_POINT('Ctrl Pts',(7.15134686593554,2.05881196747679,15.7290897972457));
#27031=CARTESIAN_POINT('Ctrl Pts',(7.21283475474115,1.97572806112051,15.7351324988654));
#27032=CARTESIAN_POINT('Ctrl Pts',(7.27037105363037,1.89006901801239,15.7411752004851));
#27033=CARTESIAN_POINT('Ctrl Pts',(7.32797339400618,1.80431165348532,15.7472248380566));
#27034=CARTESIAN_POINT('Ctrl Pts',(7.38161484736974,1.71597361231948,15.7532744756282));
#27035=CARTESIAN_POINT('Ctrl Pts',(7.43107318596542,1.62546474315855,15.7593241131997));
#27036=CARTESIAN_POINT('Ctrl Pts',(7.48056239692778,1.53489937749825,15.7653775270127));
#27037=CARTESIAN_POINT('Ctrl Pts',(7.5258631056482,1.44216087624684,15.7714309408257));
#27038=CARTESIAN_POINT('Ctrl Pts',(7.56680071099599,1.34768036671191,15.7774843546387));
#27039=CARTESIAN_POINT('Ctrl Pts',(7.60780727671575,1.2530407025067,15.7835479655715));
#27040=CARTESIAN_POINT('Ctrl Pts',(7.64443591059099,1.15665357617439,15.7896115765044));
#27041=CARTESIAN_POINT('Ctrl Pts',(7.676561438148,1.05896668330369,15.7956751874372));
#27042=CARTESIAN_POINT('Ctrl Pts',(7.69672519224084,0.997652998028258,15.7994810443075));
#27043=CARTESIAN_POINT('Ctrl Pts',(7.71511595455904,0.93582753295867,15.8032869011778));
#27044=CARTESIAN_POINT('Ctrl Pts',(7.73171311583309,0.87360273579135,15.8070927580481));
#27045=CARTESIAN_POINT('Ctrl Pts',(7.76750271846708,0.739423117492312,15.8152995894948));
#27046=CARTESIAN_POINT('Ctrl Pts',(7.79504513129767,0.603033542451122,15.8235064209414));
#27047=CARTESIAN_POINT('Ctrl Pts',(7.81413184432017,0.465302052071446,15.8317132523881));
#27048=CARTESIAN_POINT('Ctrl Pts',(7.83277876971196,0.330744110000419,15.839730985641));
#27049=CARTESIAN_POINT('Ctrl Pts',(7.84335525746938,0.194904947860224,15.8477487188939));
#27050=CARTESIAN_POINT('Ctrl Pts',(7.84571229878143,0.0586143682396561,
15.8557664521468));
#27051=CARTESIAN_POINT('Ctrl Pts',(7.84602728349793,0.0404010898538724,
15.8568379070351));
#27052=CARTESIAN_POINT('Ctrl Pts',(7.84619554872783,0.0221797858149499,
15.8579093619233));
#27053=CARTESIAN_POINT('Ctrl Pts',(7.84621680191345,0.00395247126457767,
15.8589808168116));
#27054=CARTESIAN_POINT('Ctrl Pts',(7.63534113152507,-1.17693572858576,14.3356579957882));
#27055=CARTESIAN_POINT('Ctrl Pts',(7.58665830007405,-1.30842675843014,14.3432073630502));
#27056=CARTESIAN_POINT('Ctrl Pts',(7.52981495633585,-1.43690350974026,14.3508698715488));
#27057=CARTESIAN_POINT('Ctrl Pts',(7.43034157789848,-1.62855023279599,14.3630352623339));
#27058=CARTESIAN_POINT('Ctrl Pts',(7.39337400048291,-1.69430864236812,14.3673500024656));
#27059=CARTESIAN_POINT('Ctrl Pts',(7.3171048693977,-1.81997040719947,14.3759065961932));
#27060=CARTESIAN_POINT('Ctrl Pts',(7.27803684851843,-1.87996904659493,14.3801387631629));
#27061=CARTESIAN_POINT('Ctrl Pts',(7.1697796117886,-2.03524121704058,14.3915056785217));
#27062=CARTESIAN_POINT('Ctrl Pts',(7.09748081369061,-2.12821834469454,14.3987479684427));
#27063=CARTESIAN_POINT('Ctrl Pts',(6.90572744719545,-2.34996308525917,14.4171216305944));
#27064=CARTESIAN_POINT('Ctrl Pts',(6.78082891353199,-2.47356780965724,14.4284001614553));
#27065=CARTESIAN_POINT('Ctrl Pts',(6.54513791918609,-2.67313672004542,14.448146401));
#27066=CARTESIAN_POINT('Ctrl Pts',(6.43833404809872,-2.75325515800436,14.4566174958412));
#27067=CARTESIAN_POINT('Ctrl Pts',(6.28614368746979,-2.85396311487142,14.467810967368));
#27068=CARTESIAN_POINT('Ctrl Pts',(6.24462221213434,-2.88016033644655,14.4707809031204));
#27069=CARTESIAN_POINT('Ctrl Pts',(6.16712095307125,-2.92673594625997,14.4761517285764));
#27070=CARTESIAN_POINT('Ctrl Pts',(6.13131182239407,-2.94737425722543,14.4785656933484));
#27071=CARTESIAN_POINT('Ctrl Pts',(6.02910052406289,-3.00381848249485,14.4852875006851));
#27072=CARTESIAN_POINT('Ctrl Pts',(5.96186458046848,-3.03807193768808,14.4895144352655));
#27073=CARTESIAN_POINT('Ctrl Pts',(5.79041986550873,-3.11832382280282,14.4999455924316));
#27074=CARTESIAN_POINT('Ctrl Pts',(5.68493106863429,-3.16136864905155,14.5060552710834));
#27075=CARTESIAN_POINT('Ctrl Pts',(5.36434262180131,-3.27370930169096,14.5242198963593));
#27076=CARTESIAN_POINT('Ctrl Pts',(5.14430083175794,-3.32690333446928,14.5362052077099));
#27077=CARTESIAN_POINT('Ctrl Pts',(4.84118412000192,-3.36880224647428,14.5533268161884));
#27078=CARTESIAN_POINT('Ctrl Pts',(4.76139765575346,-3.37695889736455,14.5578841101741));
#27079=CARTESIAN_POINT('Ctrl Pts',(4.61169672140212,-3.386914471621,14.5665701949982));
#27080=CARTESIAN_POINT('Ctrl Pts',(4.54186975807453,-3.38939389127869,14.5706763849023));
#27081=CARTESIAN_POINT('Ctrl Pts',(4.3710570939619,-3.39017749914986,14.5808734183801));
#27082=CARTESIAN_POINT('Ctrl Pts',(4.27013270249032,-3.38612971543642,14.5870296703624));
#27083=CARTESIAN_POINT('Ctrl Pts',(3.89507564888938,-3.35426895289127,14.6103964485958));
#27084=CARTESIAN_POINT('Ctrl Pts',(3.62447768362533,-3.29758189131736,14.6283357623796));
#27085=CARTESIAN_POINT('Ctrl Pts',(3.28423225754883,-3.18171737751498,14.6509980102216));
#27086=CARTESIAN_POINT('Ctrl Pts',(3.20572417750778,-3.15168270766108,14.6562251345375));
#27087=CARTESIAN_POINT('Ctrl Pts',(3.08939687548366,-3.10214706804349,14.6638902516287));
#27088=CARTESIAN_POINT('Ctrl Pts',(3.0506974745338,-3.08480301837545,14.6664261899912));
#27089=CARTESIAN_POINT('Ctrl Pts',(2.96993186230833,-3.04677014599326,14.6716749052445));
#27090=CARTESIAN_POINT('Ctrl Pts',(2.92794978728981,-3.02592638411615,14.6743793807556));
#27091=CARTESIAN_POINT('Ctrl Pts',(2.77233647371357,-2.9446000788038,14.684362339319));
#27092=CARTESIAN_POINT('Ctrl Pts',(2.66173957348852,-2.87852809822419,14.6913749023029));
#27093=CARTESIAN_POINT('Ctrl Pts',(2.32034767048848,-2.64723185885417,14.7135618886605));
#27094=CARTESIAN_POINT('Ctrl Pts',(2.10644564829221,-2.45931597448323,14.7284149760165));
#27095=CARTESIAN_POINT('Ctrl Pts',(1.86824108031662,-2.19025487106494,14.7486522756236));
#27096=CARTESIAN_POINT('Ctrl Pts',(1.81995673141202,-2.1318869563682,14.7529830975558));
#27097=CARTESIAN_POINT('Ctrl Pts',(1.72999089231061,-2.01539774554924,14.7615476289362));
#27098=CARTESIAN_POINT('Ctrl Pts',(1.68811383121299,-1.95747783878978,14.7657707974927));
#27099=CARTESIAN_POINT('Ctrl Pts',(1.58294498875684,-1.80188817326071,14.7770438672238));
#27100=CARTESIAN_POINT('Ctrl Pts',(1.52280149843369,-1.70221379493733,14.7841975758383));
#27101=CARTESIAN_POINT('Ctrl Pts',(1.38710717112199,-1.44870179233611,14.8022070655818));
#27102=CARTESIAN_POINT('Ctrl Pts',(1.31786626984022,-1.29185342656602,14.8132009644796));
#27103=CARTESIAN_POINT('Ctrl Pts',(1.21353971397055,-0.996932400158895,
14.8332140649252));
#27104=CARTESIAN_POINT('Ctrl Pts',(1.17471713020541,-0.860566842966036,
14.8422223309456));
#27105=CARTESIAN_POINT('Ctrl Pts',(1.13421693637355,-0.674827950371699,
14.8538717916236));
#27106=CARTESIAN_POINT('Ctrl Pts',(1.12491086327081,-0.627273830276235,
14.8568004474482));
#27107=CARTESIAN_POINT('Ctrl Pts',(1.10952079673458,-0.538581191569215,
14.8621432926503));
#27108=CARTESIAN_POINT('Ctrl Pts',(1.1031684688041,-0.497501378902117,14.8645688951387));
#27109=CARTESIAN_POINT('Ctrl Pts',(1.08714444288074,-0.379549574504474,
14.8714155560912));
#27110=CARTESIAN_POINT('Ctrl Pts',(1.07934971595382,-0.302444835208961,
14.8757501548422));
#27111=CARTESIAN_POINT('Ctrl Pts',(1.05884368415505,0.00562206874243125,
14.8927376340647));
#27112=CARTESIAN_POINT('Ctrl Pts',(1.06713816428454,0.237355099552328,14.9048160444102));
#27113=CARTESIAN_POINT('Ctrl Pts',(1.11719527366864,0.597667210703678,14.9244786301573));
#27114=CARTESIAN_POINT('Ctrl Pts',(1.14310031675231,0.727693949935586,14.9317520085179));
#27115=CARTESIAN_POINT('Ctrl Pts',(1.19500238578548,0.926597992621719,14.9433829339954));
#27116=CARTESIAN_POINT('Ctrl Pts',(1.21574190170364,0.996712133932492,14.9475820310902));
#27117=CARTESIAN_POINT('Ctrl Pts',(1.2617824576632,1.13567357929309,14.9561332479691));
#27118=CARTESIAN_POINT('Ctrl Pts',(1.28708340665714,1.2044792870784,14.9604834579008));
#27119=CARTESIAN_POINT('Ctrl Pts',(1.36505824067115,1.39701767719163,14.9730082906015));
#27120=CARTESIAN_POINT('Ctrl Pts',(1.42288665691261,1.51850272654646,14.9813390990154));
#27121=CARTESIAN_POINT('Ctrl Pts',(1.60426636518422,1.84759095634546,15.0050575059857));
#27122=CARTESIAN_POINT('Ctrl Pts',(1.74299680962739,2.04590208162645,15.0207635131366));
#27123=CARTESIAN_POINT('Ctrl Pts',(1.94730839967958,2.28020908736534,15.0402064664162));
#27124=CARTESIAN_POINT('Ctrl Pts',(1.9946167381705,2.33120680529413,15.044495683185));
#27125=CARTESIAN_POINT('Ctrl Pts',(2.07200824219159,2.40964796146776,15.0511392392657));
#27126=CARTESIAN_POINT('Ctrl Pts',(2.10107235135283,2.43806555070188,15.053555381949));
#27127=CARTESIAN_POINT('Ctrl Pts',(2.16795749864627,2.50114983282787,15.0589326165445));
#27128=CARTESIAN_POINT('Ctrl Pts',(2.20606680305857,2.53549323590168,15.0618732435799));
#27129=CARTESIAN_POINT('Ctrl Pts',(2.29227548982036,2.60970720895876,15.0682953773071));
#27130=CARTESIAN_POINT('Ctrl Pts',(2.34072739422313,2.64914014221746,15.0717541803964));
#27131=CARTESIAN_POINT('Ctrl Pts',(2.5056517970391,2.77595218334675,15.0831359743811));
#27132=CARTESIAN_POINT('Ctrl Pts',(2.62666148457519,2.85716751379135,15.090867503483));
#27133=CARTESIAN_POINT('Ctrl Pts',(2.91504857675248,3.02485934193698,15.1086988718904));
#27134=CARTESIAN_POINT('Ctrl Pts',(3.08514059464031,3.10567235453147,15.118813556833));
#27135=CARTESIAN_POINT('Ctrl Pts',(3.33323004691758,3.19917015252111,15.1337102988387));
#27136=CARTESIAN_POINT('Ctrl Pts',(3.40631725950975,3.22390066125,15.1381120743341));
#27137=CARTESIAN_POINT('Ctrl Pts',(3.5479582078042,3.26650001131454,15.146703113605));
#27138=CARTESIAN_POINT('Ctrl Pts',(3.61635348425968,3.28475555331739,15.1508777403627));
#27139=CARTESIAN_POINT('Ctrl Pts',(3.7924795844436,3.32590514944427,15.1617130095826));
#27140=CARTESIAN_POINT('Ctrl Pts',(3.90083988234605,3.34571360508594,15.1684612664841));
#27141=CARTESIAN_POINT('Ctrl Pts',(4.1989099542007,3.38532115905227,15.1872315736512));
#27142=CARTESIAN_POINT('Ctrl Pts',(4.3896267794975,3.39444526709788,15.199485802204));
#27143=CARTESIAN_POINT('Ctrl Pts',(4.71063843488363,3.38273124638337,15.2200182019993));
#27144=CARTESIAN_POINT('Ctrl Pts',(4.84082033104307,3.37042310054339,15.2283105864281));
#27145=CARTESIAN_POINT('Ctrl Pts',(5.01882257874528,3.34314309902446,15.2393598723331));
#27146=CARTESIAN_POINT('Ctrl Pts',(5.06750369496389,3.33458910640888,15.2423508945855));
#27147=CARTESIAN_POINT('Ctrl Pts',(5.15658138557914,3.31692039853889,15.2477465933055));
#27148=CARTESIAN_POINT('Ctrl Pts',(5.19702846418774,3.30812485669626,15.2501648877283));
#27149=CARTESIAN_POINT('Ctrl Pts',(5.31052830341169,3.28125736917216,15.2568816765116));
#27150=CARTESIAN_POINT('Ctrl Pts',(5.38315857167098,3.26148972639281,15.2611001485773));
#27151=CARTESIAN_POINT('Ctrl Pts',(5.56339371484462,3.20592745947531,15.2714988217269));
#27152=CARTESIAN_POINT('Ctrl Pts',(5.66997433634521,3.16712178894913,15.2775857755976));
#27153=CARTESIAN_POINT('Ctrl Pts',(5.98255982154462,3.03520876974245,15.2957402386209));
#27154=CARTESIAN_POINT('Ctrl Pts',(6.18138621916954,2.926789627391,15.307736739289));
#27155=CARTESIAN_POINT('Ctrl Pts',(6.43414839274631,2.75419969122762,15.3248694910294));
#27156=CARTESIAN_POINT('Ctrl Pts',(6.49872275389224,2.7066639871127,15.3294274881923));
#27157=CARTESIAN_POINT('Ctrl Pts',(6.61647908348397,2.61336440861976,15.3381283550049));
#27158=CARTESIAN_POINT('Ctrl Pts',(6.67004371982324,2.56815167529463,15.3422491055993));
#27159=CARTESIAN_POINT('Ctrl Pts',(6.79794085571625,2.45322105327304,15.3525174249781));
#27160=CARTESIAN_POINT('Ctrl Pts',(6.87060127560662,2.38175277996041,15.3587321617202));
#27161=CARTESIAN_POINT('Ctrl Pts',(7.13101337127555,2.10143745365094,15.3824962629268));
#27162=CARTESIAN_POINT('Ctrl Pts',(7.29577961548857,1.87283606016177,15.4008007176375));
#27163=CARTESIAN_POINT('Ctrl Pts',(7.4687210491343,1.55662984957034,15.4234755609165));
#27164=CARTESIAN_POINT('Ctrl Pts',(7.50449258466896,1.48536627018671,15.4284225009341));
#27165=CARTESIAN_POINT('Ctrl Pts',(7.55515400789082,1.3748841065386,15.4357803426442));
#27166=CARTESIAN_POINT('Ctrl Pts',(7.57188376927471,1.33654275360874,15.4382781052162));
#27167=CARTESIAN_POINT('Ctrl Pts',(7.60607147938297,1.25405821995434,15.4435206211345));
#27168=CARTESIAN_POINT('Ctrl Pts',(7.62332024031651,1.20983946454218,15.4462547959012));
#27169=CARTESIAN_POINT('Ctrl Pts',(7.68853669589925,1.03168785497911,15.4570220163268));
#27170=CARTESIAN_POINT('Ctrl Pts',(7.72898510253545,0.895146443451765,15.464723959605));
#27171=CARTESIAN_POINT('Ctrl Pts',(7.81671710716394,0.511925485432159,15.4857933823505));
#27172=CARTESIAN_POINT('Ctrl Pts',(7.84537866092038,0.261953575955565,15.4989885251966));
#27173=CARTESIAN_POINT('Ctrl Pts',(7.84646533925544,-0.0695636817773458,
15.51751063256));
#27174=CARTESIAN_POINT('Ctrl Pts',(7.84384964399876,-0.150217268898216,
15.5220897220954));
#27175=CARTESIAN_POINT('Ctrl Pts',(7.83364721216822,-0.299779499649458,
15.5307589005805));
#27176=CARTESIAN_POINT('Ctrl Pts',(7.82681933920101,-0.36869771872418,15.5348241423345));
#27177=CARTESIAN_POINT('Ctrl Pts',(7.80525540834102,-0.534433442984226,
15.5447895926238));
#27178=CARTESIAN_POINT('Ctrl Pts',(7.78842605609443,-0.630911194058193,
15.5507490720102));
#27179=CARTESIAN_POINT('Ctrl Pts',(7.74079236167246,-0.847993049410495,
15.5645217296209));
#27180=CARTESIAN_POINT('Ctrl Pts',(7.7074747316849,-0.967899760807301,15.5723917826965));
#27181=CARTESIAN_POINT('Ctrl Pts',(7.65731059974537,-1.11627074897095,15.5823947841524));
#27182=CARTESIAN_POINT('Ctrl Pts',(7.6465404989509,-1.14668653131824,15.5844594627058));
#27183=CARTESIAN_POINT('Ctrl Pts',(7.63534118765004,-1.1769355769937,15.5865253037982));
#27184=CARTESIAN_POINT('Origin',(4.45646910621825,3.5527136788005E-15,11.));
#27185=CARTESIAN_POINT('',(1.91109182286968,-2.23862894377631,16.));
#27186=CARTESIAN_POINT('Ctrl Pts',(7.63534118765004,-1.1769355769937,15.5865253037982));
#27187=CARTESIAN_POINT('Ctrl Pts',(7.57287868542809,-1.34564515492739,15.5980472269201));
#27188=CARTESIAN_POINT('Ctrl Pts',(7.49706535147243,-1.50916707843466,15.609622999056));
#27189=CARTESIAN_POINT('Ctrl Pts',(7.38299228721335,-1.71130966053183,15.6239307665769));
#27190=CARTESIAN_POINT('Ctrl Pts',(7.35634675334713,-1.75608341487065,15.6270983971135));
#27191=CARTESIAN_POINT('Ctrl Pts',(7.30731325697073,-1.83431488249896,15.6326072562216));
#27192=CARTESIAN_POINT('Ctrl Pts',(7.28534509373262,-1.86801613048383,15.6349694244418));
#27193=CARTESIAN_POINT('Ctrl Pts',(7.22605793113205,-1.95552266151023,15.6410851910244));
#27194=CARTESIAN_POINT('Ctrl Pts',(7.187771701958,-2.00865088652369,15.6447831805304));
#27195=CARTESIAN_POINT('Ctrl Pts',(7.09317533200132,-2.13220766450349,15.6534293053547));
#27196=CARTESIAN_POINT('Ctrl Pts',(7.03554688153645,-2.20156505412838,15.6583206365791));
#27197=CARTESIAN_POINT('Ctrl Pts',(6.78504263841076,-2.4796981632243,15.6784523425935));
#27198=CARTESIAN_POINT('Ctrl Pts',(6.56908494627282,-2.6660843509193,15.6933318109013));
#27199=CARTESIAN_POINT('Ctrl Pts',(6.2690541879617,-2.8654364258646,15.7136158457069));
#27200=CARTESIAN_POINT('Ctrl Pts',(6.2043060658752,-2.90538385109082,15.7179651487505));
#27201=CARTESIAN_POINT('Ctrl Pts',(6.07601642730848,-2.97869316118489,15.7265625524124));
#27202=CARTESIAN_POINT('Ctrl Pts',(6.01265104129785,-3.0122820496391,15.7307999191233));
#27203=CARTESIAN_POINT('Ctrl Pts',(5.84334705324833,-3.09525898965031,15.7421167677686));
#27204=CARTESIAN_POINT('Ctrl Pts',(5.73584343432221,-3.14121880076511,15.7493004664225));
#27205=CARTESIAN_POINT('Ctrl Pts',(5.46402481317999,-3.24115548378397,15.7674347008708));
#27206=CARTESIAN_POINT('Ctrl Pts',(5.29754601618224,-3.28828838792893,15.7785252537061));
#27207=CARTESIAN_POINT('Ctrl Pts',(4.99426819976438,-3.34960470921569,15.7982985254542));
#27208=CARTESIAN_POINT('Ctrl Pts',(4.85879821671769,-3.36856295242495,15.8069772564395));
#27209=CARTESIAN_POINT('Ctrl Pts',(4.67331741345244,-3.3831671935792,15.8183833240157));
#27210=CARTESIAN_POINT('Ctrl Pts',(4.62400801301181,-3.38596732532963,15.8213695487727));
#27211=CARTESIAN_POINT('Ctrl Pts',(4.53210569139429,-3.38917343707562,15.8268290512374));
#27212=CARTESIAN_POINT('Ctrl Pts',(4.48953469607301,-3.38985608390243,15.8293138195986));
#27213=CARTESIAN_POINT('Ctrl Pts',(4.36599785529308,-3.38950956413695,15.836421574768));
#27214=CARTESIAN_POINT('Ctrl Pts',(4.28506305037642,-3.38638183531605,15.840951438062));
#27215=CARTESIAN_POINT('Ctrl Pts',(3.95145715744809,-3.36149664033698,15.8593677203472));
#27216=CARTESIAN_POINT('Ctrl Pts',(3.70151064721115,-3.31432439675801,15.8726173148998));
#27217=CARTESIAN_POINT('Ctrl Pts',(3.3530882847967,-3.20706589827191,15.8925709104828));
#27218=CARTESIAN_POINT('Ctrl Pts',(3.24869857339809,-3.16922833422206,15.89874304801));
#27219=CARTESIAN_POINT('Ctrl Pts',(3.08026511340122,-3.09864535013521,15.9091548543334));
#27220=CARTESIAN_POINT('Ctrl Pts',(3.01507087895972,-3.06886143883022,15.9133012205377));
#27221=CARTESIAN_POINT('Ctrl Pts',(2.88006749071585,-3.0019341215573,15.9221615100324));
#27222=CARTESIAN_POINT('Ctrl Pts',(2.81051621535204,-2.96436976939012,15.9268873165097));
#27223=CARTESIAN_POINT('Ctrl Pts',(2.56913471593602,-2.82288562411376,15.9438927047818));
#27224=CARTESIAN_POINT('Ctrl Pts',(2.40530800731997,-2.70618437371263,15.9565884738196));
#27225=CARTESIAN_POINT('Ctrl Pts',(2.13105570550647,-2.47154271046629,15.9796856731913));
#27226=CARTESIAN_POINT('Ctrl Pts',(2.0168726413096,-2.35890438871753,15.9899931553525));
#27227=CARTESIAN_POINT('Ctrl Pts',(1.91109182286968,-2.23862894377631,16.));
#27228=CARTESIAN_POINT('',(7.02970353323295,-2.20655152809223,16.));
#27229=CARTESIAN_POINT('Origin',(4.45646910621825,4.66293670342566E-15,
16.));
#27230=CARTESIAN_POINT('Ctrl Pts',(7.63534122786842,-1.17693546836491,15.9331819277137));
#27231=CARTESIAN_POINT('Ctrl Pts',(7.60150329790276,-1.26833083804343,15.9386824302914));
#27232=CARTESIAN_POINT('Ctrl Pts',(7.56373832442186,-1.35822782981906,15.9440894988472));
#27233=CARTESIAN_POINT('Ctrl Pts',(7.41799056413079,-1.66714887260322,15.9628796855318));
#27234=CARTESIAN_POINT('Ctrl Pts',(7.29029618195467,-1.87600691097348,15.975933202696));
#27235=CARTESIAN_POINT('Ctrl Pts',(7.1216017376502,-2.09487803078569,15.9916272221289));
#27236=CARTESIAN_POINT('Ctrl Pts',(7.1015435677313,-2.12014784525936,15.9934733811096));
#27237=CARTESIAN_POINT('Ctrl Pts',(7.06422882167378,-2.16580411711061,15.9968789069984));
#27238=CARTESIAN_POINT('Ctrl Pts',(7.04708601173215,-2.18628044376383,15.9984327879153));
#27239=CARTESIAN_POINT('Ctrl Pts',(7.02970353323297,-2.20655152809224,16.));
#27240=CARTESIAN_POINT('Origin',(4.45646910621825,2.93978508838399E-15,
8.23961502859548));
#27241=CARTESIAN_POINT('',(8.54146786266509,-0.00318744843224361,15.0103849714045));
#27242=CARTESIAN_POINT('Ctrl Pts',(7.70074909849077,2.48902547716684,14.8803008071898));
#27243=CARTESIAN_POINT('Ctrl Pts',(8.23604156339096,1.78066392614847,14.9236620772348));
#27244=CARTESIAN_POINT('Ctrl Pts',(8.53482634894621,0.886500306172487,14.9670233472798));
#27245=CARTESIAN_POINT('Ctrl Pts',(8.54231068068493,-0.00318084115196966,
15.0103846173248));
#27246=CARTESIAN_POINT('',(5.51582329814257,3.94524950998694,16.));
#27247=CARTESIAN_POINT('Ctrl Pts',(8.54146786266509,-0.00318744843224361,
15.0103849714045));
#27248=CARTESIAN_POINT('Ctrl Pts',(8.5413411088023,-0.16563380102107,15.0183039705911));
#27249=CARTESIAN_POINT('Ctrl Pts',(8.5315207628645,-0.327697487422329,15.0262229697777));
#27250=CARTESIAN_POINT('Ctrl Pts',(8.5121651071872,-0.488420871507605,15.0341419689643));
#27251=CARTESIAN_POINT('Ctrl Pts',(8.49838784829654,-0.602822972332438,
15.0397786729731));
#27252=CARTESIAN_POINT('Ctrl Pts',(8.47978051169544,-0.716546691674619,
15.0454153769818));
#27253=CARTESIAN_POINT('Ctrl Pts',(8.45641452956138,-0.829253646525672,
15.0510520809906));
#27254=CARTESIAN_POINT('Ctrl Pts',(8.43220699270667,-0.946019881631264,
15.0568917978597));
#27255=CARTESIAN_POINT('Ctrl Pts',(8.40284581144963,-1.06190116149562,15.0627315147288));
#27256=CARTESIAN_POINT('Ctrl Pts',(8.36841025348841,-1.17641041320381,15.0685712315979));
#27257=CARTESIAN_POINT('Ctrl Pts',(8.33401631542241,-1.2907812654395,15.074403890402));
#27258=CARTESIAN_POINT('Ctrl Pts',(8.29456031716066,-1.40378300303146,15.0802365492062));
#27259=CARTESIAN_POINT('Ctrl Pts',(8.25017254001739,-1.51493869723509,15.0860692080103));
#27260=CARTESIAN_POINT('Ctrl Pts',(8.20582704431374,-1.62598851042653,15.0918963109334));
#27261=CARTESIAN_POINT('Ctrl Pts',(8.15655926661547,-1.7351954043223,15.0977234138565));
#27262=CARTESIAN_POINT('Ctrl Pts',(8.10254912597376,-1.84209812158294,15.1035505167796));
#27263=CARTESIAN_POINT('Ctrl Pts',(8.04832335640828,-1.94942763495255,15.109400883703));
#27264=CARTESIAN_POINT('Ctrl Pts',(7.98931739859561,-2.05443413914575,15.1152512506265));
#27265=CARTESIAN_POINT('Ctrl Pts',(7.92576215543467,-2.15667121709787,15.1211016175499));
#27266=CARTESIAN_POINT('Ctrl Pts',(7.86252503512946,-2.2583965520437,15.12692270073));
#27267=CARTESIAN_POINT('Ctrl Pts',(7.79478429093661,-2.35737977853133,15.13274378391));
#27268=CARTESIAN_POINT('Ctrl Pts',(7.72281287859392,-2.45320675049259,15.1385648670901));
#27269=CARTESIAN_POINT('Ctrl Pts',(7.65085054814479,-2.54902163028654,15.1443852157221));
#27270=CARTESIAN_POINT('Ctrl Pts',(7.57465885507154,-2.64168072367093,15.1502055643542));
#27271=CARTESIAN_POINT('Ctrl Pts',(7.49455278544562,-2.73080071737431,15.1560259129862));
#27272=CARTESIAN_POINT('Ctrl Pts',(7.41443824631905,-2.81993013360768,15.1618468769954));
#27273=CARTESIAN_POINT('Ctrl Pts',(7.33040877887661,-2.90551940457022,15.1676678410046));
#27274=CARTESIAN_POINT('Ctrl Pts',(7.24281775831271,-2.98722047880151,15.1734888050138));
#27275=CARTESIAN_POINT('Ctrl Pts',(7.15445059989371,-3.06964550048889,15.1793613481746));
#27276=CARTESIAN_POINT('Ctrl Pts',(7.06245876169525,-3.1481127873312,15.1852338913353));
#27277=CARTESIAN_POINT('Ctrl Pts',(6.96724001975915,-3.22230576136355,15.191106434496));
#27278=CARTESIAN_POINT('Ctrl Pts',(6.87272504013762,-3.29595037466282,15.1969355736536));
#27279=CARTESIAN_POINT('Ctrl Pts',(6.77503106424927,-3.36538345784704,15.2027647128113));
#27280=CARTESIAN_POINT('Ctrl Pts',(6.67457632515266,-3.43033895778694,15.2085938519689));
#27281=CARTESIAN_POINT('Ctrl Pts',(6.57299960105461,-3.49601994959859,15.2144880971312));
#27282=CARTESIAN_POINT('Ctrl Pts',(6.46860043536605,-3.55712251093729,15.2203823422935));
#27283=CARTESIAN_POINT('Ctrl Pts',(6.36183591102191,-3.6134197568442,15.2262765874557));
#27284=CARTESIAN_POINT('Ctrl Pts',(6.25507138667778,-3.66971700275111,15.232170832618));
#27285=CARTESIAN_POINT('Ctrl Pts',(6.14594190981078,-3.72120880250603,15.2380650777802));
#27286=CARTESIAN_POINT('Ctrl Pts',(6.03492343531498,-3.76771906210581,15.2439593229425));
#27287=CARTESIAN_POINT('Ctrl Pts',(5.92492052612997,-3.81380385912867,15.2497996492327));
#27288=CARTESIAN_POINT('Ctrl Pts',(5.81273256134718,-3.85513637126823,15.2556399755229));
#27289=CARTESIAN_POINT('Ctrl Pts',(5.69880623137363,-3.89150658067803,15.2614803018131));
#27290=CARTESIAN_POINT('Ctrl Pts',(5.58501722399287,-3.92783295077993,15.2673135883896));
#27291=CARTESIAN_POINT('Ctrl Pts',(5.46949440303382,-3.95920879479499,15.2731468749661));
#27292=CARTESIAN_POINT('Ctrl Pts',(5.35270492787875,-3.98547191082465,15.2789801615426));
#27293=CARTESIAN_POINT('Ctrl Pts',(5.23602634221444,-4.01171009050144,15.2848079095192));
#27294=CARTESIAN_POINT('Ctrl Pts',(5.11808388891667,-4.03284511277884,15.2906356574958));
#27295=CARTESIAN_POINT('Ctrl Pts',(4.99935986061935,-4.04876458055856,15.2964634054723));
#27296=CARTESIAN_POINT('Ctrl Pts',(4.88017982787431,-4.06474519306371,15.3023135371149));
#27297=CARTESIAN_POINT('Ctrl Pts',(4.76021259868044,-4.07546998267526,15.3081636687575));
#27298=CARTESIAN_POINT('Ctrl Pts',(4.63995681778763,-4.08087702089915,15.3140138004001));
#27299=CARTESIAN_POINT('Ctrl Pts',(4.52028412955,-4.08625784163686,15.3198355660983));
#27300=CARTESIAN_POINT('Ctrl Pts',(4.40032609066979,-4.0863723552476,15.3256573317965));
#27301=CARTESIAN_POINT('Ctrl Pts',(4.28057873228645,-4.08121153291003,15.3314790974947));
#27302=CARTESIAN_POINT('Ctrl Pts',(4.1608462210599,-4.07605135044911,15.3373001413676));
#27303=CARTESIAN_POINT('Ctrl Pts',(4.0413247433305,-4.06561715068618,15.3431211852406));
#27304=CARTESIAN_POINT('Ctrl Pts',(3.92250866190083,-4.04995200513587,15.3489422291135));
#27305=CARTESIAN_POINT('Ctrl Pts',(3.80367977842117,-4.03428517171659,15.3547639001852));
#27306=CARTESIAN_POINT('Ctrl Pts',(3.68555684430889,-4.01338632485481,15.3605855712569));
#27307=CARTESIAN_POINT('Ctrl Pts',(3.56862684375788,-3.98735013724516,15.3664072423285));
#27308=CARTESIAN_POINT('Ctrl Pts',(3.45069380063571,-3.961090607427,15.3722788525423));
#27309=CARTESIAN_POINT('Ctrl Pts',(3.3339746663379,-3.92960526169728,15.3781504627562));
#27310=CARTESIAN_POINT('Ctrl Pts',(3.21895516564525,-3.89304305741501,15.38402207297));
#27311=CARTESIAN_POINT('Ctrl Pts',(3.10475334874284,-3.85674077707256,15.3898519413882));
#27312=CARTESIAN_POINT('Ctrl Pts',(2.99222744075082,-3.81543378496055,15.3956818098063));
#27313=CARTESIAN_POINT('Ctrl Pts',(2.88183347553818,-3.76931659994123,15.4015116782245));
#27314=CARTESIAN_POINT('Ctrl Pts',(2.77025388090635,-3.72270411709305,15.4074041593362));
#27315=CARTESIAN_POINT('Ctrl Pts',(2.66085267758504,-3.67117769267325,15.4132966404478));
#27316=CARTESIAN_POINT('Ctrl Pts',(2.55407500616508,-3.61498571063325,15.4191891215595));
#27317=CARTESIAN_POINT('Ctrl Pts',(2.44729733474513,-3.55879372859326,15.4250816026711));
#27318=CARTESIAN_POINT('Ctrl Pts',(2.3431435318916,-3.49793644933757,15.4309740837828));
#27319=CARTESIAN_POINT('Ctrl Pts',(2.24202757610946,-3.43270647008001,15.4368665648944));
#27320=CARTESIAN_POINT('Ctrl Pts',(2.14194567540971,-3.36814356053517,15.4426987869699));
#27321=CARTESIAN_POINT('Ctrl Pts',(2.04453658637758,-3.29910139922817,15.4485310090453));
#27322=CARTESIAN_POINT('Ctrl Pts',(1.95022553558227,-3.22582829125258,15.4543632311207));
#27323=CARTESIAN_POINT('Ctrl Pts',(1.85602877352911,-3.15264397765764,15.460188385548));
#27324=CARTESIAN_POINT('Ctrl Pts',(1.7649229002841,-3.07523916397955,15.4660135399753));
#27325=CARTESIAN_POINT('Ctrl Pts',(1.67730536800752,-2.99390613016078,15.4718386944026));
#27326=CARTESIAN_POINT('Ctrl Pts',(1.58977140288305,-2.91265066951524,15.4776582929604));
#27327=CARTESIAN_POINT('Ctrl Pts',(1.50571945568293,-2.82747471837483,15.4834778915183));
#27328=CARTESIAN_POINT('Ctrl Pts',(1.42551452648788,-2.73871125451575,15.4892974900762));
#27329=CARTESIAN_POINT('Ctrl Pts',(1.34484678420236,-2.64943559155067,15.4951506699416));
#27330=CARTESIAN_POINT('Ctrl Pts',(1.26807092816672,-2.55653113690343,15.5010038498071));
#27331=CARTESIAN_POINT('Ctrl Pts',(1.19552151049901,-2.46037512952245,15.5068570296725));
#27332=CARTESIAN_POINT('Ctrl Pts',(1.1234623353685,-2.36486888290511,15.5126706574941));
#27333=CARTESIAN_POINT('Ctrl Pts',(1.05557289281068,-2.26615522929675,15.5184842853157));
#27334=CARTESIAN_POINT('Ctrl Pts',(0.992140699584164,-2.16463708066453,
15.5242979131372));
#27335=CARTESIAN_POINT('Ctrl Pts',(0.928716171215153,-2.06313119902331,
15.5301108384665));
#27336=CARTESIAN_POINT('Ctrl Pts',(0.869748036305858,-1.95882184132671,
15.5359237637958));
#27337=CARTESIAN_POINT('Ctrl Pts',(0.81547991001562,-1.85214002525064,15.541736689125));
#27338=CARTESIAN_POINT('Ctrl Pts',(0.761205659274564,-1.7454461695561,15.5475502704743));
#27339=CARTESIAN_POINT('Ctrl Pts',(0.711632656193029,-1.63637968566105,
15.5533638518235));
#27340=CARTESIAN_POINT('Ctrl Pts',(0.666957787042784,-1.52539469051153,
15.5591774331728));
#27341=CARTESIAN_POINT('Ctrl Pts',(0.621749226162056,-1.41308385434119,
15.5650604643122));
#27342=CARTESIAN_POINT('Ctrl Pts',(0.581556761098714,-1.29880876174253,
15.5709434954517));
#27343=CARTESIAN_POINT('Ctrl Pts',(0.546533210655599,-1.18305802587635,
15.5768265265912));
#27344=CARTESIAN_POINT('Ctrl Pts',(0.511873454813608,-1.06850960937103,
15.5826484498492));
#27345=CARTESIAN_POINT('Ctrl Pts',(0.482275781891699,-0.952516472742291,
15.5884703731073));
#27346=CARTESIAN_POINT('Ctrl Pts',(0.457837045881869,-0.835563669656465,
15.5942922963654));
#27347=CARTESIAN_POINT('Ctrl Pts',(0.433013540273867,-0.716769532263069,
15.6002058814455));
#27348=CARTESIAN_POINT('Ctrl Pts',(0.413512868062081,-0.596985686145653,
15.6061194665257));
#27349=CARTESIAN_POINT('Ctrl Pts',(0.399381823433392,-0.476726105709688,
15.6120330516059));
#27350=CARTESIAN_POINT('Ctrl Pts',(0.385250778804703,-0.356466525273724,
15.617946636686));
#27351=CARTESIAN_POINT('Ctrl Pts',(0.376489335374794,-0.235731647345663,
15.6238602217662));
#27352=CARTESIAN_POINT('Ctrl Pts',(0.373089128535008,-0.11503459416781,
15.6297738068464));
#27353=CARTESIAN_POINT('Ctrl Pts',(0.369726628840985,0.00432396944400208,
15.6356218122648));
#27354=CARTESIAN_POINT('Ctrl Pts',(0.371596773978119,0.124007618084114,
15.6414698176831));
#27355=CARTESIAN_POINT('Ctrl Pts',(0.378734248619421,0.243522958102947,
15.6473178231015));
#27356=CARTESIAN_POINT('Ctrl Pts',(0.385863086186289,0.362893672334705,
15.6531587518351));
#27357=CARTESIAN_POINT('Ctrl Pts',(0.398246548617625,0.482096082697366,
15.6589996805687));
#27358=CARTESIAN_POINT('Ctrl Pts',(0.41586733996857,0.600634969494553,15.6648406093023));
#27359=CARTESIAN_POINT('Ctrl Pts',(0.433471282366683,0.719060509730135,
15.6706759529557));
#27360=CARTESIAN_POINT('Ctrl Pts',(0.456302529571249,0.836823391003327,
15.6765112966091));
#27361=CARTESIAN_POINT('Ctrl Pts',(0.48429187559633,0.953432246427892,15.6823466402625));
#27362=CARTESIAN_POINT('Ctrl Pts',(0.512338412306017,1.07027936895118,15.6881939072848));
#27363=CARTESIAN_POINT('Ctrl Pts',(0.545564109953098,1.18596733781551,15.6940411743072));
#27364=CARTESIAN_POINT('Ctrl Pts',(0.583847487984841,1.30001030841721,15.6998884413295));
#27365=CARTESIAN_POINT('Ctrl Pts',(0.622012563543342,1.41370086587849,15.7057176392528));
#27366=CARTESIAN_POINT('Ctrl Pts',(0.665203977606165,1.52575619181223,15.711546837176));
#27367=CARTESIAN_POINT('Ctrl Pts',(0.713251241136526,1.63570933069809,15.7173760350993));
#27368=CARTESIAN_POINT('Ctrl Pts',(0.761291932672498,1.74564742998837,15.7232044356939));
#27369=CARTESIAN_POINT('Ctrl Pts',(0.814186990406992,1.85348354396727,15.7290328362886));
#27370=CARTESIAN_POINT('Ctrl Pts',(0.871717914306646,1.95877101573617,15.7348612368833));
#27371=CARTESIAN_POINT('Ctrl Pts',(0.929254198221601,2.06406829688099,15.7406901804958));
#27372=CARTESIAN_POINT('Ctrl Pts',(0.991427013163506,2.16681610898482,15.7465191241083));
#27373=CARTESIAN_POINT('Ctrl Pts',(1.05797235982619,2.26659322878243,15.7523480677208));
#27374=CARTESIAN_POINT('Ctrl Pts',(1.12488460726435,2.36692047423816,15.7582091494772));
#27375=CARTESIAN_POINT('Ctrl Pts',(1.19621752800744,2.46424382093391,15.7640702312337));
#27376=CARTESIAN_POINT('Ctrl Pts',(1.27165979670493,2.55816626942758,15.7699313129902));
#27377=CARTESIAN_POINT('Ctrl Pts',(1.34679040001563,2.65170070763547,15.7757681815788));
#27378=CARTESIAN_POINT('Ctrl Pts',(1.42599615792973,2.74186202032279,15.7816050501675));
#27379=CARTESIAN_POINT('Ctrl Pts',(1.50893111671808,2.8282936199152,15.7874419187561));
#27380=CARTESIAN_POINT('Ctrl Pts',(1.59238213597053,2.91526303772144,15.7933151070965));
#27381=CARTESIAN_POINT('Ctrl Pts',(1.67960862327778,2.99845588218391,15.7991882954368));
#27382=CARTESIAN_POINT('Ctrl Pts',(1.77022349490056,3.07754927103958,15.8050614837772));
#27383=CARTESIAN_POINT('Ctrl Pts',(1.86083836652335,3.15664265989526,15.8109346721176));
#27384=CARTESIAN_POINT('Ctrl Pts',(1.95484126823265,3.23163637683839,15.816807860458));
#27385=CARTESIAN_POINT('Ctrl Pts',(2.05181547261778,3.30225164129141,15.8226810487983));
#27386=CARTESIAN_POINT('Ctrl Pts',(2.14726457977139,3.37175635119023,15.8284618704796));
#27387=CARTESIAN_POINT('Ctrl Pts',(2.2458864851227,3.43723342380028,15.8342426921609));
#27388=CARTESIAN_POINT('Ctrl Pts',(2.34730393370927,3.49837780622319,15.8400235138421));
#27389=CARTESIAN_POINT('Ctrl Pts',(2.44859973993677,3.55944885070449,15.8457974018764));
#27390=CARTESIAN_POINT('Ctrl Pts',(2.55268406939279,3.61619732635631,15.8515712899107));
#27391=CARTESIAN_POINT('Ctrl Pts',(2.65914838909259,3.66835974786971,15.857345177945));
#27392=CARTESIAN_POINT('Ctrl Pts',(2.76874848648944,3.72205855038348,15.863289128864));
#27393=CARTESIAN_POINT('Ctrl Pts',(2.88087060154035,3.7708966766293,15.8692330797829));
#27394=CARTESIAN_POINT('Ctrl Pts',(2.99503843076587,3.81463568127372,15.8751770307019));
#27395=CARTESIAN_POINT('Ctrl Pts',(3.10576537254859,3.85705644247896,15.8809418377568));
#27396=CARTESIAN_POINT('Ctrl Pts',(3.21841607103216,3.89468086910897,15.8867066448117));
#27397=CARTESIAN_POINT('Ctrl Pts',(3.33253362675537,3.92733930772531,15.8924714518666));
#27398=CARTESIAN_POINT('Ctrl Pts',(3.4466163765667,3.95998778550146,15.8982345006525));
#27399=CARTESIAN_POINT('Ctrl Pts',(3.56216469559778,3.98767317264522,15.9039975494383));
#27400=CARTESIAN_POINT('Ctrl Pts',(3.6787058761839,4.01027547158625,15.9097605982242));
#27401=CARTESIAN_POINT('Ctrl Pts',(3.7952400504662,4.03287641170654,15.9155233005431));
#27402=CARTESIAN_POINT('Ctrl Pts',(3.91276656017482,4.05039479318396,15.9212860028619));
#27403=CARTESIAN_POINT('Ctrl Pts',(4.03080256205276,4.0627617445745,15.9270487051808));
#27404=CARTESIAN_POINT('Ctrl Pts',(4.14886037304497,4.07513098096496,15.9328124722548));
#27405=CARTESIAN_POINT('Ctrl Pts',(4.26742745071431,4.08234685297824,15.9385762393288));
#27406=CARTESIAN_POINT('Ctrl Pts',(4.38601662049575,4.08439242082042,15.9443400064027));
#27407=CARTESIAN_POINT('Ctrl Pts',(4.50471413997829,4.08643985760784,15.9501090395768));
#27408=CARTESIAN_POINT('Ctrl Pts',(4.62343337673524,4.08330755509177,15.9558780727509));
#27409=CARTESIAN_POINT('Ctrl Pts',(4.74168797811218,4.07503069867153,15.9616471059249));
#27410=CARTESIAN_POINT('Ctrl Pts',(4.86000791660193,4.06674926918693,15.9674193265604));
#27411=CARTESIAN_POINT('Ctrl Pts',(4.97786229705627,4.05331767293681,15.9731915471958));
#27412=CARTESIAN_POINT('Ctrl Pts',(5.09477231469533,4.0348226744242,15.9789637678312));
#27413=CARTESIAN_POINT('Ctrl Pts',(5.21183125092389,4.01630411720253,15.9847433410526));
#27414=CARTESIAN_POINT('Ctrl Pts',(5.32794301877643,3.99270937000933,15.990522914274));
#27415=CARTESIAN_POINT('Ctrl Pts',(5.442641425784,3.96417572215487,15.9963024874954));
#27416=CARTESIAN_POINT('Ctrl Pts',(5.46710106308048,3.95809087149762,15.9975349916636));
#27417=CARTESIAN_POINT('Ctrl Pts',(5.49149649048049,3.95178159512065,15.9987674958318));
#27418=CARTESIAN_POINT('Ctrl Pts',(5.51582329814257,3.94524950998694,16.));
#27419=CARTESIAN_POINT('',(3.39856468324527,3.94563850749836,16.));
#27420=CARTESIAN_POINT('Origin',(4.45646910621825,4.66293670342566E-15,
16.));
#27421=CARTESIAN_POINT('',(8.53632693677507,0.0015752080993986,15.1146150285955));
#27422=CARTESIAN_POINT('Ctrl Pts',(8.53632693677507,0.0015752080993986,
15.1146150285955));
#27423=CARTESIAN_POINT('Ctrl Pts',(8.53325914244515,-0.779403576318215,
15.1525336964611));
#27424=CARTESIAN_POINT('Ctrl Pts',(7.94795211119873,-2.88890213248947,15.2547547783107));
#27425=CARTESIAN_POINT('Ctrl Pts',(4.59757515362052,-4.78052237191921,15.4212782741442));
#27426=CARTESIAN_POINT('Ctrl Pts',(0.59094744836049,-2.82224505491953,15.6141855160961));
#27427=CARTESIAN_POINT('Ctrl Pts',(-0.0515142140919883,1.59610399861122,
15.8070927580481));
#27428=CARTESIAN_POINT('Ctrl Pts',(2.12325861577974,3.60370350081894,15.935697586016));
#27429=CARTESIAN_POINT('Ctrl Pts',(3.39856468324527,3.94563850749837,16.));
#27430=CARTESIAN_POINT('Ctrl Pts',(7.69668968132748,2.48593167737241,14.9842676783293));
#27431=CARTESIAN_POINT('Ctrl Pts',(7.91254316798409,2.20967240609126,15.0013330489663));
#27432=CARTESIAN_POINT('Ctrl Pts',(8.37131842804349,1.43864013141511,15.0447821657217));
#27433=CARTESIAN_POINT('Ctrl Pts',(8.53846150297425,0.544978949099729,15.0882312824771));
#27434=CARTESIAN_POINT('Ctrl Pts',(8.53632693677507,0.0015752080993986,
15.1146150285955));
#27435=CARTESIAN_POINT('Ctrl Pts',(1.88874933522258,-2.20462348696943,11.0030161694783));
#27436=CARTESIAN_POINT('Ctrl Pts',(1.17566490599146,-1.37417471128399,11.0673602442838));
#27437=CARTESIAN_POINT('Ctrl Pts',(0.626876868360273,1.01685904464542,11.1960067330733));
#27438=CARTESIAN_POINT('Ctrl Pts',(3.13358816217676,3.73802129086872,11.3889556358469));
#27439=CARTESIAN_POINT('Ctrl Pts',(6.78925200599098,3.20274742655601,11.5818628777988));
#27440=CARTESIAN_POINT('Ctrl Pts',(8.41799749193089,-0.111210130011926,
11.7747701197507));
#27441=CARTESIAN_POINT('Ctrl Pts',(6.60488546490453,-3.33054749553302,11.9676773617027));
#27442=CARTESIAN_POINT('Ctrl Pts',(2.92512050779011,-3.65517177063915,12.1605846036546));
#27443=CARTESIAN_POINT('Ctrl Pts',(0.575862327608668,-0.804564055767342,
12.3534918456065));
#27444=CARTESIAN_POINT('Ctrl Pts',(1.59820716428631,2.74533767611897,12.5463990875585));
#27445=CARTESIAN_POINT('Ctrl Pts',(5.10391712761201,3.90985954717001,12.7393063295104));
#27446=CARTESIAN_POINT('Ctrl Pts',(8.04709879850609,1.67742102317504,12.9322135714623));
#27447=CARTESIAN_POINT('Ctrl Pts',(7.87061306779546,-2.01245497181881,13.1251208134143));
#27448=CARTESIAN_POINT('Ctrl Pts',(4.72779527045753,-3.9538206853119,13.3180280553662));
#27449=CARTESIAN_POINT('Ctrl Pts',(1.349240122848,-2.45997262452168,13.5109352973181));
#27450=CARTESIAN_POINT('Ctrl Pts',(0.670356745591222,1.171191815988,13.70384253927));
#27451=CARTESIAN_POINT('Ctrl Pts',(3.28098566906297,3.78478215455868,13.896749781222));
#27452=CARTESIAN_POINT('Ctrl Pts',(6.91291436436904,3.11001488625209,14.0896570231739));
#27453=CARTESIAN_POINT('Ctrl Pts',(8.41059997631734,-0.26683902657174,14.2825642651258));
#27454=CARTESIAN_POINT('Ctrl Pts',(6.47278403753293,-3.41186708033681,14.4754715070778));
#27455=CARTESIAN_POINT('Ctrl Pts',(2.783140900988,-3.59251490415614,14.6683787490297));
#27456=CARTESIAN_POINT('Ctrl Pts',(0.547306324484669,-0.651909986519413,
14.8612859909816));
#27457=CARTESIAN_POINT('Ctrl Pts',(1.70797095253967,2.85520405387232,15.0541932329336));
#27458=CARTESIAN_POINT('Ctrl Pts',(5.25647654433333,3.88140403742585,15.2471004748855));
#27459=CARTESIAN_POINT('Ctrl Pts',(8.11020963540048,1.53571469214933,15.4400077168373));
#27460=CARTESIAN_POINT('Ctrl Pts',(7.78884317528094,-2.14507759945015,15.6329149587894));
#27461=CARTESIAN_POINT('Ctrl Pts',(4.5733715585354,-3.96053038776695,15.8258222007413));
#27462=CARTESIAN_POINT('Ctrl Pts',(1.25399146895312,-2.33815186545114,16.0187294426932));
#27463=CARTESIAN_POINT('Ctrl Pts',(0.72172977469463,1.32232795848172,16.2116366846452));
#27464=CARTESIAN_POINT('Ctrl Pts',(2.52346883354543,2.98556854525621,16.3402415126131));
#27465=CARTESIAN_POINT('Ctrl Pts',(3.58002459062539,3.26885222834281,16.4045439265971));
#27466=CARTESIAN_POINT('Ctrl Pts',(1.71092191398567,-2.35730467668278,10.8676966229016));
#27467=CARTESIAN_POINT('Ctrl Pts',(0.948452825802773,-1.46934317475766,
10.9320406977071));
#27468=CARTESIAN_POINT('Ctrl Pts',(0.361658475084007,1.0872816132268,11.0606871864966));
#27469=CARTESIAN_POINT('Ctrl Pts',(3.04197204832368,3.99689793862148,11.2536360892702));
#27470=CARTESIAN_POINT('Ctrl Pts',(6.95080887526387,3.42455368523382,11.4465433312221));
#27471=CARTESIAN_POINT('Ctrl Pts',(8.69235312253574,-0.118911987067678,
11.639450573174));
#27472=CARTESIAN_POINT('Ctrl Pts',(6.75367403020043,-3.5612045474153,11.832357815126));
#27473=CARTESIAN_POINT('Ctrl Pts',(2.81906696746642,-3.90831067523958,12.0252650570779));
#27474=CARTESIAN_POINT('Ctrl Pts',(0.307110922541194,-0.860284135845062,
12.2181722990298));
#27475=CARTESIAN_POINT('Ctrl Pts',(1.40025824630285,2.93546602457946,12.4110795409818));
#27476=CARTESIAN_POINT('Ctrl Pts',(5.14875613743306,4.18063685259307,12.6039867829337));
#27477=CARTESIAN_POINT('Ctrl Pts',(8.29576784175946,1.79359080862017,12.7968940248856));
#27478=CARTESIAN_POINT('Ctrl Pts',(8.10705959255911,-2.15182753187632,12.9898012668376));
#27479=CARTESIAN_POINT('Ctrl Pts',(4.74658596274637,-4.22764251916004,13.1827085087895));
#27480=CARTESIAN_POINT('Ctrl Pts',(1.13404899352509,-2.63033801761223,13.3756157507414));
#27481=CARTESIAN_POINT('Ctrl Pts',(0.408149551017793,1.25230269995729,13.5685229926933));
#27482=CARTESIAN_POINT('Ctrl Pts',(3.19957756888897,4.0468972257168,13.7614302346453));
#27483=CARTESIAN_POINT('Ctrl Pts',(7.0830354697174,3.32539895326659,13.9543374765972));
#27484=CARTESIAN_POINT('Ctrl Pts',(8.68444329201153,-0.285318962161525,
14.1472447185491));
#27485=CARTESIAN_POINT('Ctrl Pts',(6.61242391906804,-3.64815591970037,14.3401519605011));
#27486=CARTESIAN_POINT('Ctrl Pts',(2.6672545636313,-3.84131450774899,14.533059202453));
#27487=CARTESIAN_POINT('Ctrl Pts',(0.276577273548778,-0.697058009715255,
14.7259664444049));
#27488=CARTESIAN_POINT('Ctrl Pts',(1.51762372521994,3.05294119783193,14.9188736863569));
#27489=CARTESIAN_POINT('Ctrl Pts',(5.31188105587596,4.15021065664908,15.1117809283088));
#27490=CARTESIAN_POINT('Ctrl Pts',(8.36324941938022,1.64207060627412,15.3046881702608));
#27491=CARTESIAN_POINT('Ctrl Pts',(8.01962672650482,-2.29363493899012,15.4975954122127));
#27492=CARTESIAN_POINT('Ctrl Pts',(4.5814676373469,-4.23481690202856,15.6905026541646));
#27493=CARTESIAN_POINT('Ctrl Pts',(1.03220389453143,-2.50008056241803,15.8834098961165));
#27494=CARTESIAN_POINT('Ctrl Pts',(0.463080419021611,1.41390577532233,16.0763171380685));
#27495=CARTESIAN_POINT('Ctrl Pts',(2.38959890832132,3.19233408148256,16.2049219660364));
#27496=CARTESIAN_POINT('Ctrl Pts',(3.51932642962448,3.49523657477221,16.2692243800204));
#27497=CARTESIAN_POINT('Ctrl Pts',(1.53309449274875,-2.50998586639613,10.7323770763249));
#27498=CARTESIAN_POINT('Ctrl Pts',(0.721240745614079,-1.56451163823132,
10.7967211511304));
#27499=CARTESIAN_POINT('Ctrl Pts',(0.0964400818077463,1.1577041818082,10.9253676399199));
#27500=CARTESIAN_POINT('Ctrl Pts',(2.95035593447059,4.25577458637424,11.1183165426935));
#27501=CARTESIAN_POINT('Ctrl Pts',(7.11236574453675,3.64635994391164,11.3112237846454));
#27502=CARTESIAN_POINT('Ctrl Pts',(8.96670875314062,-0.126613844123434,
11.5041310265973));
#27503=CARTESIAN_POINT('Ctrl Pts',(6.90246259549634,-3.79186159929757,11.6970382685493));
#27504=CARTESIAN_POINT('Ctrl Pts',(2.71301342714273,-4.16144957984,11.8899455105012));
#27505=CARTESIAN_POINT('Ctrl Pts',(0.0383595174737219,-0.91600421592278,
12.0828527524531));
#27506=CARTESIAN_POINT('Ctrl Pts',(1.20230932831938,3.12559437303996,12.2757599944051));
#27507=CARTESIAN_POINT('Ctrl Pts',(5.19359514725411,4.45141415801615,12.468667236357));
#27508=CARTESIAN_POINT('Ctrl Pts',(8.54443688501279,1.9097605940653,12.6615744783089));
#27509=CARTESIAN_POINT('Ctrl Pts',(8.34350611732276,-2.29120009193381,12.8544817202609));
#27510=CARTESIAN_POINT('Ctrl Pts',(4.76537665503522,-4.50146435300819,13.0473889622128));
#27511=CARTESIAN_POINT('Ctrl Pts',(0.91885786420218,-2.8007034107028,13.2402962041647));
#27512=CARTESIAN_POINT('Ctrl Pts',(0.145942356444369,1.3334135839266,13.4332034461166));
#27513=CARTESIAN_POINT('Ctrl Pts',(3.11816946871495,4.30901229687492,13.6261106880686));
#27514=CARTESIAN_POINT('Ctrl Pts',(7.25315657506574,3.54078302028111,13.8190179300205));
#27515=CARTESIAN_POINT('Ctrl Pts',(8.95828660770572,-0.303798897751314,
14.0119251719725));
#27516=CARTESIAN_POINT('Ctrl Pts',(6.75206380060314,-3.88444475906391,14.2048324139244));
#27517=CARTESIAN_POINT('Ctrl Pts',(2.5513682262746,-4.09011411134184,14.3977396558763));
#27518=CARTESIAN_POINT('Ctrl Pts',(0.00584822261288385,-0.742206032911097,
14.5906468978282));
#27519=CARTESIAN_POINT('Ctrl Pts',(1.32727649790022,3.25067834179152,14.7835541397802));
#27520=CARTESIAN_POINT('Ctrl Pts',(5.36728556741858,4.4190172758723,14.9764613817321));
#27521=CARTESIAN_POINT('Ctrl Pts',(8.61628920335996,1.74842652039892,15.1693686236841));
#27522=CARTESIAN_POINT('Ctrl Pts',(8.2504102777287,-2.44219227853008,15.3622758656359));
#27523=CARTESIAN_POINT('Ctrl Pts',(4.58956371615841,-4.50910341629017,15.5551831075879));
#27524=CARTESIAN_POINT('Ctrl Pts',(0.810416320109747,-2.66200925938492,
15.7480903495398));
#27525=CARTESIAN_POINT('Ctrl Pts',(0.204431063348593,1.50548359216295,15.9409975914918));
#27526=CARTESIAN_POINT('Ctrl Pts',(2.25572898309721,3.39909961770891,16.0696024194597));
#27527=CARTESIAN_POINT('Ctrl Pts',(3.45862826862358,3.72162092120162,16.1339048334437));
#27528=CARTESIAN_POINT('Ctrl Pts',(1.35526707151184,-2.66266705610948,10.5970575297482));
#27529=CARTESIAN_POINT('Ctrl Pts',(0.494028665425391,-1.65968010170499,
10.6614016045537));
#27530=CARTESIAN_POINT('Ctrl Pts',(-0.168778311468517,1.22812675038958,
10.7900480933432));
#27531=CARTESIAN_POINT('Ctrl Pts',(2.85873982061751,4.514651234127,10.9829969961168));
#27532=CARTESIAN_POINT('Ctrl Pts',(7.27392261380964,3.86816620258945,11.1759042380687));
#27533=CARTESIAN_POINT('Ctrl Pts',(9.24106438374548,-0.134315701179191,
11.3688114800206));
#27534=CARTESIAN_POINT('Ctrl Pts',(7.05125116079224,-4.02251865117984,11.5617187219726));
#27535=CARTESIAN_POINT('Ctrl Pts',(2.60695988681904,-4.41458848444044,11.7546259639245));
#27536=CARTESIAN_POINT('Ctrl Pts',(-0.23039188759375,-0.971724296000493,
11.9475332058764));
#27537=CARTESIAN_POINT('Ctrl Pts',(1.00436041033591,3.31572272150045,12.1404404478284));
#27538=CARTESIAN_POINT('Ctrl Pts',(5.23843415707517,4.72219146343922,12.3333476897803));
#27539=CARTESIAN_POINT('Ctrl Pts',(8.79310592826617,2.02593037951044,12.5262549317322));
#27540=CARTESIAN_POINT('Ctrl Pts',(8.57995264208641,-2.43057265199133,12.7191621736841));
#27541=CARTESIAN_POINT('Ctrl Pts',(4.78416734732407,-4.77528618685632,12.9120694156361));
#27542=CARTESIAN_POINT('Ctrl Pts',(0.703666734879273,-2.97106880379335,
13.104976657588));
#27543=CARTESIAN_POINT('Ctrl Pts',(-0.11626483812906,1.41452446789591,13.29788389954));
#27544=CARTESIAN_POINT('Ctrl Pts',(3.03676136854093,4.57112736803304,13.4907911414919));
#27545=CARTESIAN_POINT('Ctrl Pts',(7.42327768041408,3.75616708729562,13.6836983834438));
#27546=CARTESIAN_POINT('Ctrl Pts',(9.23212992339991,-0.3222788333411,13.8766056253958));
#27547=CARTESIAN_POINT('Ctrl Pts',(6.89170368213823,-4.12073359842746,14.0695128673477));
#27548=CARTESIAN_POINT('Ctrl Pts',(2.4354818889179,-4.3389137149347,14.2624201092996));
#27549=CARTESIAN_POINT('Ctrl Pts',(-0.264880828323011,-0.787354056106939,
14.4553273512515));
#27550=CARTESIAN_POINT('Ctrl Pts',(1.1369292705805,3.44841548575112,14.6482345932035));
#27551=CARTESIAN_POINT('Ctrl Pts',(5.4226900789612,4.68782389509552,14.8411418351554));
#27552=CARTESIAN_POINT('Ctrl Pts',(8.8693289873397,1.85478243452371,15.0340490771074));
#27553=CARTESIAN_POINT('Ctrl Pts',(8.48119382895259,-2.59074961807004,15.2269563190593));
#27554=CARTESIAN_POINT('Ctrl Pts',(4.59765979496991,-4.78338993055177,15.4198635610112));
#27555=CARTESIAN_POINT('Ctrl Pts',(0.588628745688067,-2.8239379563518,15.6127708029631));
#27556=CARTESIAN_POINT('Ctrl Pts',(-0.0542182923244291,1.59706140900356,
15.8056780449151));
#27557=CARTESIAN_POINT('Ctrl Pts',(2.12185905787311,3.60586515393528,15.934282872883));
#27558=CARTESIAN_POINT('Ctrl Pts',(3.39793010762267,3.94800526763103,15.998585286867));
#27559=CARTESIAN_POINT('',(1.88073622819142,-2.20722158127997,16.0013706388591));
#27560=CARTESIAN_POINT('Ctrl Pts',(3.39856468324527,3.94563850749837,16.));
#27561=CARTESIAN_POINT('Ctrl Pts',(3.28202030975535,3.90360924880686,16.));
#27562=CARTESIAN_POINT('Ctrl Pts',(3.16786744659433,3.85598433920628,16.));
#27563=CARTESIAN_POINT('Ctrl Pts',(3.05633992967595,3.80312375344169,16.));
#27564=CARTESIAN_POINT('Ctrl Pts',(2.94320845217846,3.74950294008397,16.));
#27565=CARTESIAN_POINT('Ctrl Pts',(2.83277776842474,3.69049416048462,16.));
#27566=CARTESIAN_POINT('Ctrl Pts',(2.72531960853723,3.62642595238742,16.));
#27567=CARTESIAN_POINT('Ctrl Pts',(2.61747630627299,3.56212811648006,16.));
#27568=CARTESIAN_POINT('Ctrl Pts',(2.51262629745618,3.49273382302628,16.));
#27569=CARTESIAN_POINT('Ctrl Pts',(2.41108080109129,3.41853797691784,16.));
#27570=CARTESIAN_POINT('Ctrl Pts',(2.31970398669266,3.35177204143373,16.));
#27571=CARTESIAN_POINT('Ctrl Pts',(2.23100318802705,3.28111721609057,16.));
#27572=CARTESIAN_POINT('Ctrl Pts',(2.14523612212338,3.2067697882004,16.));
#27573=CARTESIAN_POINT('Ctrl Pts',(2.12553341153843,3.18969043683141,16.));
#27574=CARTESIAN_POINT('Ctrl Pts',(2.10598565701931,3.17241615849946,16.));
#27575=CARTESIAN_POINT('Ctrl Pts',(2.08659623083789,3.15494923869773,16.));
#27576=CARTESIAN_POINT('Ctrl Pts',(2.07346743197746,3.14312219056115,16.));
#27577=CARTESIAN_POINT('Ctrl Pts',(2.06041075551566,3.13120630250859,16.));
#27578=CARTESIAN_POINT('Ctrl Pts',(2.04743902034581,3.11921338474378,16.));
#27579=CARTESIAN_POINT('Ctrl Pts',(1.95695137795596,3.03555373245333,16.));
#27580=CARTESIAN_POINT('Ctrl Pts',(1.87045372604639,2.94802365738912,16.));
#27581=CARTESIAN_POINT('Ctrl Pts',(1.78820622702511,2.85693355462572,16.));
#27582=CARTESIAN_POINT('Ctrl Pts',(1.70636656276958,2.7662951338121,16.));
#27583=CARTESIAN_POINT('Ctrl Pts',(1.62873453532577,2.67213117469647,16.));
#27584=CARTESIAN_POINT('Ctrl Pts',(1.55560880797602,2.57471863739693,16.));
#27585=CARTESIAN_POINT('Ctrl Pts',(1.48414674748959,2.47952231067405,16.));
#27586=CARTESIAN_POINT('Ctrl Pts',(1.41698799538791,2.38122284820218,16.));
#27587=CARTESIAN_POINT('Ctrl Pts',(1.35445714150433,2.2800616594694,16.));
#27588=CARTESIAN_POINT('Ctrl Pts',(1.30322496354497,2.19717924699847,16.));
#27589=CARTESIAN_POINT('Ctrl Pts',(1.25510007876846,2.11237539198043,16.));
#27590=CARTESIAN_POINT('Ctrl Pts',(1.21028684180597,2.02577869828326,16.));
#27591=CARTESIAN_POINT('Ctrl Pts',(1.19940037733246,2.00474179282054,16.));
#27592=CARTESIAN_POINT('Ctrl Pts',(1.18870946405183,1.98359907557885,16.));
#27593=CARTESIAN_POINT('Ctrl Pts',(1.17821725735083,1.96235238134681,16.));
#27594=CARTESIAN_POINT('Ctrl Pts',(1.17068532266993,1.94710023108889,16.));
#27595=CARTESIAN_POINT('Ctrl Pts',(1.16325564947536,1.93179406050165,16.));
#27596=CARTESIAN_POINT('Ctrl Pts',(1.1559358887606,1.91644852551603,16.));
#27597=CARTESIAN_POINT('Ctrl Pts',(1.10479654173714,1.80923728330855,16.));
#27598=CARTESIAN_POINT('Ctrl Pts',(1.05893622144905,1.69994266655825,16.));
#27599=CARTESIAN_POINT('Ctrl Pts',(1.01863595797368,1.58882409063619,16.));
#27600=CARTESIAN_POINT('Ctrl Pts',(0.978335694498304,1.47770551471412,16.));
#27601=CARTESIAN_POINT('Ctrl Pts',(0.943595041491022,1.36476231430696,16.));
#27602=CARTESIAN_POINT('Ctrl Pts',(0.914749671847378,1.25024175865813,16.));
#27603=CARTESIAN_POINT('Ctrl Pts',(0.885779102083194,1.1352241392674,16.));
#27604=CARTESIAN_POINT('Ctrl Pts',(0.86275565775235,1.01861437498697,16.));
#27605=CARTESIAN_POINT('Ctrl Pts',(0.845598658915959,0.90085030095086,16.));
#27606=CARTESIAN_POINT('Ctrl Pts',(0.831120401325252,0.801472862327414,
16.));
#27607=CARTESIAN_POINT('Ctrl Pts',(0.820820742045749,0.70127314279097,16.));
#27608=CARTESIAN_POINT('Ctrl Pts',(0.814678949007698,0.60052222210086,16.));
#27609=CARTESIAN_POINT('Ctrl Pts',(0.813612852730977,0.583033814276209,
16.));
#27610=CARTESIAN_POINT('Ctrl Pts',(0.812672011048267,0.565527040601622,
16.));
#27611=CARTESIAN_POINT('Ctrl Pts',(0.811856646346995,0.548008964376364,
16.));
#27612=CARTESIAN_POINT('Ctrl Pts',(0.806452329785345,0.431897450933631,
16.));
#27613=CARTESIAN_POINT('Ctrl Pts',(0.806572191820612,0.315663183512141,
16.));
#27614=CARTESIAN_POINT('Ctrl Pts',(0.812080775670422,0.199712141557808,
16.));
#27615=CARTESIAN_POINT('Ctrl Pts',(0.817610950513495,0.0833066274135428,
16.));
#27616=CARTESIAN_POINT('Ctrl Pts',(0.828572461873298,-0.0328143597299322,
16.));
#27617=CARTESIAN_POINT('Ctrl Pts',(0.844880372876002,-0.148231554630927,
16.));
#27618=CARTESIAN_POINT('Ctrl Pts',(0.860929151250057,-0.261814770851201,
16.));
#27619=CARTESIAN_POINT('Ctrl Pts',(0.882156183196351,-0.374717177214322,
16.));
#27620=CARTESIAN_POINT('Ctrl Pts',(0.908525430112972,-0.48651830323896,
16.));
#27621=CARTESIAN_POINT('Ctrl Pts',(0.934174610638338,-0.595266470124897,
16.));
#27622=CARTESIAN_POINT('Ctrl Pts',(0.964689424390745,-0.702973283207877,
16.));
#27623=CARTESIAN_POINT('Ctrl Pts',(1.00007335372366,-0.809221818042884,
16.));
#27624=CARTESIAN_POINT('Ctrl Pts',(1.00618513661092,-0.827573877558135,
16.));
#27625=CARTESIAN_POINT('Ctrl Pts',(1.01244299210376,-0.845884215742526,
16.));
#27626=CARTESIAN_POINT('Ctrl Pts',(1.01884102638095,-0.864133973362507,
16.));
#27627=CARTESIAN_POINT('Ctrl Pts',(1.05633935617679,-0.971094236511956,
16.));
#27628=CARTESIAN_POINT('Ctrl Pts',(1.09868814478405,-1.07609606771823,16.));
#27629=CARTESIAN_POINT('Ctrl Pts',(1.14583717685756,-1.17872972024771,16.));
#27630=CARTESIAN_POINT('Ctrl Pts',(1.19194649734206,-1.27910013653954,16.));
#27631=CARTESIAN_POINT('Ctrl Pts',(1.24264710795939,-1.37720628510166,16.));
#27632=CARTESIAN_POINT('Ctrl Pts',(1.29792934727226,-1.47263173604749,16.));
#27633=CARTESIAN_POINT('Ctrl Pts',(1.30556674318026,-1.48581502886686,16.));
#27634=CARTESIAN_POINT('Ctrl Pts',(1.31329163876066,-1.49894709614249,16.));
#27635=CARTESIAN_POINT('Ctrl Pts',(1.32110405940516,-1.51202677853915,16.));
#27636=CARTESIAN_POINT('Ctrl Pts',(1.33325253512357,-1.53236595524647,16.));
#27637=CARTESIAN_POINT('Ctrl Pts',(1.34561265097563,-1.55257846553154,16.));
#27638=CARTESIAN_POINT('Ctrl Pts',(1.35818455886885,-1.57265987081225,16.));
#27639=CARTESIAN_POINT('Ctrl Pts',(1.37208187483147,-1.59485838169298,16.));
#27640=CARTESIAN_POINT('Ctrl Pts',(1.38623418537527,-1.61689039162208,16.));
#27641=CARTESIAN_POINT('Ctrl Pts',(1.40063305058271,-1.63873806372697,16.));
#27642=CARTESIAN_POINT('Ctrl Pts',(1.45988719596097,-1.72864550576699,16.));
#27643=CARTESIAN_POINT('Ctrl Pts',(1.52335388710929,-1.81549818378269,16.));
#27644=CARTESIAN_POINT('Ctrl Pts',(1.5910140471,-1.89891001383453,16.));
#27645=CARTESIAN_POINT('Ctrl Pts',(1.62378066270062,-1.93930488390621,16.));
#27646=CARTESIAN_POINT('Ctrl Pts',(1.65753128028433,-1.97889221644688,16.));
#27647=CARTESIAN_POINT('Ctrl Pts',(1.69226646643322,-2.01762466210545,16.));
#27648=CARTESIAN_POINT('Ctrl Pts',(1.75164790813293,-2.08383960777761,16.));
#27649=CARTESIAN_POINT('Ctrl Pts',(1.81390655502903,-2.14755714347611,16.));
#27650=CARTESIAN_POINT('Ctrl Pts',(1.87883962139859,-2.20868246298984,16.));
#27651=CARTESIAN_POINT('Ctrl Pts',(1.8825077481285,-2.20570351352142,16.0013706388591));
#27652=CARTESIAN_POINT('Ctrl Pts',(1.89196505514197,-2.21673978501259,16.0009137592394));
#27653=CARTESIAN_POINT('Ctrl Pts',(1.90149334280166,-2.22771523108277,16.0004568796197));
#27654=CARTESIAN_POINT('Ctrl Pts',(1.91109182286969,-2.23862894377632,16.));
#27655=CARTESIAN_POINT('Ctrl Pts',(1.88323467920355,-2.20655152809223,11.));
#27656=CARTESIAN_POINT('Ctrl Pts',(1.8055137100667,-2.1325841428619,11.));
#27657=CARTESIAN_POINT('Ctrl Pts',(1.73182315237859,-2.05488482981754,11.));
#27658=CARTESIAN_POINT('Ctrl Pts',(1.66216469772015,-1.97388508600905,11.));
#27659=CARTESIAN_POINT('Ctrl Pts',(1.59146480714577,-1.89167434717063,11.));
#27660=CARTESIAN_POINT('Ctrl Pts',(1.52491811166235,-1.80606324837128,11.));
#27661=CARTESIAN_POINT('Ctrl Pts',(1.46255293502529,-1.71745376975123,11.));
#27662=CARTESIAN_POINT('Ctrl Pts',(1.39865578991978,-1.62666764489089,11.));
#27663=CARTESIAN_POINT('Ctrl Pts',(1.33914763251816,-1.5327334914365,11.));
#27664=CARTESIAN_POINT('Ctrl Pts',(1.28409326921549,-1.43604026288558,11.));
#27665=CARTESIAN_POINT('Ctrl Pts',(1.23405340579292,-1.34815411435317,11.));
#27666=CARTESIAN_POINT('Ctrl Pts',(1.18769316738891,-1.25798767430718,11.));
#27667=CARTESIAN_POINT('Ctrl Pts',(1.14508996980559,-1.16580920606479,11.));
#27668=CARTESIAN_POINT('Ctrl Pts',(1.13772430980523,-1.1498724854677,11.));
#27669=CARTESIAN_POINT('Ctrl Pts',(1.13047102256546,-1.13387557920784,11.));
#27670=CARTESIAN_POINT('Ctrl Pts',(1.12333059959275,-1.11781982161107,11.));
#27671=CARTESIAN_POINT('Ctrl Pts',(1.1093173856833,-1.0863100964111,11.));
#27672=CARTESIAN_POINT('Ctrl Pts',(1.09575724481632,-1.05461492748262,11.));
#27673=CARTESIAN_POINT('Ctrl Pts',(1.08265349496083,-1.02275315280833,11.));
#27674=CARTESIAN_POINT('Ctrl Pts',(1.03921335903622,-0.917128439431273,
11.));
#27675=CARTESIAN_POINT('Ctrl Pts',(1.00077582995783,-0.809652557756684,
11.));
#27676=CARTESIAN_POINT('Ctrl Pts',(0.967380509038817,-0.700750791635124,
11.));
#27677=CARTESIAN_POINT('Ctrl Pts',(0.933548627493637,-0.590425406218982,
11.));
#27678=CARTESIAN_POINT('Ctrl Pts',(0.90489119584359,-0.478635880663496,
11.));
#27679=CARTESIAN_POINT('Ctrl Pts',(0.881490105760335,-0.36578973307862,
11.));
#27680=CARTESIAN_POINT('Ctrl Pts',(0.858871819872059,-0.256718471082503,
11.));
#27681=CARTESIAN_POINT('Ctrl Pts',(0.841163991177834,-0.14665923747458,
11.));
#27682=CARTESIAN_POINT('Ctrl Pts',(0.828481862514581,-0.0359599154309225,
11.));
#27683=CARTESIAN_POINT('Ctrl Pts',(0.818670645382047,0.0496798942440594,
11.));
#27684=CARTESIAN_POINT('Ctrl Pts',(0.811868056471992,0.135703290008098,
11.));
#27685=CARTESIAN_POINT('Ctrl Pts',(0.808146029432485,0.22195316305556,11.));
#27686=CARTESIAN_POINT('Ctrl Pts',(0.807335597792087,0.240733151850913,
11.));
#27687=CARTESIAN_POINT('Ctrl Pts',(0.806671594065359,0.259518119692736,
11.));
#27688=CARTESIAN_POINT('Ctrl Pts',(0.806154744915036,0.278294214256977,
11.));
#27689=CARTESIAN_POINT('Ctrl Pts',(0.804681400009178,0.33181788409534,11.));
#27690=CARTESIAN_POINT('Ctrl Pts',(0.804402399157995,0.385298168137166,
11.));
#27691=CARTESIAN_POINT('Ctrl Pts',(0.805323214301196,0.43869557367965,11.));
#27692=CARTESIAN_POINT('Ctrl Pts',(0.807360297208648,0.556824541188471,
11.));
#27693=CARTESIAN_POINT('Ctrl Pts',(0.815266164429257,0.674546218612187,
11.));
#27694=CARTESIAN_POINT('Ctrl Pts',(0.829134191190566,0.79144570807364,11.));
#27695=CARTESIAN_POINT('Ctrl Pts',(0.835863260857388,0.84816789516926,11.));
#27696=CARTESIAN_POINT('Ctrl Pts',(0.843996786224402,0.90469679144366,11.));
#27697=CARTESIAN_POINT('Ctrl Pts',(0.853549724724196,0.960986131300249,
11.));
#27698=CARTESIAN_POINT('Ctrl Pts',(0.872837652710683,1.07463752072187,11.));
#27699=CARTESIAN_POINT('Ctrl Pts',(0.897908375714622,1.18731256566191,11.));
#27700=CARTESIAN_POINT('Ctrl Pts',(0.928459425596507,1.2987388881876,11.));
#27701=CARTESIAN_POINT('Ctrl Pts',(0.957176084404771,1.40347478756261,11.));
#27702=CARTESIAN_POINT('Ctrl Pts',(0.9907354529883,1.50710789260008,11.));
#27703=CARTESIAN_POINT('Ctrl Pts',(1.02892793312368,1.60940652439971,11.));
#27704=CARTESIAN_POINT('Ctrl Pts',(1.03665250767009,1.63009681223991,11.));
#27705=CARTESIAN_POINT('Ctrl Pts',(1.0445684264762,1.6507365362987,11.));
#27706=CARTESIAN_POINT('Ctrl Pts',(1.05266336388591,1.67129710445659,11.));
#27707=CARTESIAN_POINT('Ctrl Pts',(1.09577961016135,1.78080931874445,11.));
#27708=CARTESIAN_POINT('Ctrl Pts',(1.14401878611999,1.88821224790122,11.));
#27709=CARTESIAN_POINT('Ctrl Pts',(1.19702431226012,1.99323454026449,11.));
#27710=CARTESIAN_POINT('Ctrl Pts',(1.25115069340324,2.10047763431377,11.));
#27711=CARTESIAN_POINT('Ctrl Pts',(1.31024736452932,2.2052390278035,11.));
#27712=CARTESIAN_POINT('Ctrl Pts',(1.37398970441365,2.30722679719885,11.));
#27713=CARTESIAN_POINT('Ctrl Pts',(1.43857455109351,2.41056257780515,11.));
#27714=CARTESIAN_POINT('Ctrl Pts',(1.50792902729321,2.51105169954105,11.));
#27715=CARTESIAN_POINT('Ctrl Pts',(1.58176693495046,2.60837638822974,11.));
#27716=CARTESIAN_POINT('Ctrl Pts',(1.64789425380196,2.69553786023291,11.));
#27717=CARTESIAN_POINT('Ctrl Pts',(1.71761843767981,2.78016148526227,11.));
#27718=CARTESIAN_POINT('Ctrl Pts',(1.79076460061867,2.86200179764899,11.));
#27719=CARTESIAN_POINT('Ctrl Pts',(1.80462848786612,2.87751354587526,11.));
#27720=CARTESIAN_POINT('Ctrl Pts',(1.81861712160808,2.89292712905613,11.));
#27721=CARTESIAN_POINT('Ctrl Pts',(1.83272383982852,2.9082347498518,11.));
#27722=CARTESIAN_POINT('Ctrl Pts',(1.9176255829498,3.00036416424024,11.));
#27723=CARTESIAN_POINT('Ctrl Pts',(2.00660734119473,3.08844926408247,11.));
#27724=CARTESIAN_POINT('Ctrl Pts',(2.09934472813356,3.17216685573294,11.));
#27725=CARTESIAN_POINT('Ctrl Pts',(2.19205925921466,3.25586381452509,11.));
#27726=CARTESIAN_POINT('Ctrl Pts',(2.28852807468961,3.33519619747782,11.));
#27727=CARTESIAN_POINT('Ctrl Pts',(2.38847157608717,3.40981510006956,11.));
#27728=CARTESIAN_POINT('Ctrl Pts',(2.43485484325298,3.44444535062247,11.));
#27729=CARTESIAN_POINT('Ctrl Pts',(2.48198708286726,3.47805995493347,11.));
#27730=CARTESIAN_POINT('Ctrl Pts',(2.52984313993709,3.5106214115124,11.));
#27731=CARTESIAN_POINT('Ctrl Pts',(2.54582219495995,3.52149362577652,11.));
#27732=CARTESIAN_POINT('Ctrl Pts',(2.56188067251407,3.53224747826245,11.));
#27733=CARTESIAN_POINT('Ctrl Pts',(2.57800967088885,3.54287650131378,11.));
#27734=CARTESIAN_POINT('Ctrl Pts',(2.68352851526793,3.61241350560839,11.));
#27735=CARTESIAN_POINT('Ctrl Pts',(2.79215458366025,3.67667351075176,11.));
#27736=CARTESIAN_POINT('Ctrl Pts',(2.90358985517431,3.73531289711206,11.));
#27737=CARTESIAN_POINT('Ctrl Pts',(2.96812460751363,3.76927232687497,11.));
#27738=CARTESIAN_POINT('Ctrl Pts',(3.0336022952464,3.80134613570095,11.));
#27739=CARTESIAN_POINT('Ctrl Pts',(3.09997070871193,3.83146190442578,11.));
#27740=CARTESIAN_POINT('Ctrl Pts',(3.1966268929033,3.87532125162025,11.));
#27741=CARTESIAN_POINT('Ctrl Pts',(3.29517172468862,3.91502891889752,11.));
#27742=CARTESIAN_POINT('Ctrl Pts',(3.39535148502737,3.95064487077574,11.));
#27743=CARTESIAN_POINT('Ctrl Pts',(5.51501591064331,3.94803438082956,11.0014321153293));
#27744=CARTESIAN_POINT('Ctrl Pts',(6.7910963703372,3.60589174413995,11.0657345293133));
#27745=CARTESIAN_POINT('Ctrl Pts',(8.9671832501964,1.59703309973906,11.1943393572812));
#27746=CARTESIAN_POINT('Ctrl Pts',(8.324343605749,-2.82394025518247,11.3872465992332));
#27747=CARTESIAN_POINT('Ctrl Pts',(4.31527680253589,-4.78343972057373,11.5801538411851));
#27748=CARTESIAN_POINT('Ctrl Pts',(0.431711818820576,-2.59076364645739,
11.773061083137));
#27749=CARTESIAN_POINT('Ctrl Pts',(0.0435744797231438,1.85479343530947,
11.9659683250889));
#27750=CARTESIAN_POINT('Ctrl Pts',(3.49023997463891,4.68786353054347,12.1588755670409));
#27751=CARTESIAN_POINT('Ctrl Pts',(7.77603578183676,3.44844184087651,12.3517828089928));
#27752=CARTESIAN_POINT('Ctrl Pts',(9.1778565836221,-0.787359679550689,12.5446900509448));
#27753=CARTESIAN_POINT('Ctrl Pts',(6.47747259983249,-4.33894876625295,12.7375972928967));
#27754=CARTESIAN_POINT('Ctrl Pts',(2.0212149918786,-4.1207663374878,12.9305045348486));
#27755=CARTESIAN_POINT('Ctrl Pts',(-0.319229843460022,-0.32228151621117,
13.1234117768006));
#27756=CARTESIAN_POINT('Ctrl Pts',(1.48963679342153,3.75619716622437,13.3163190187525));
#27757=CARTESIAN_POINT('Ctrl Pts',(5.87618820434026,4.57116388545287,13.5092262607044));
#27758=CARTESIAN_POINT('Ctrl Pts',(9.02923959854263,1.41453577360683,13.7021335026564));
#27759=CARTESIAN_POINT('Ctrl Pts',(8.20930147313774,-2.97109252818595,13.8950407446083));
#27760=CARTESIAN_POINT('Ctrl Pts',(4.12876825682516,-4.77532441590242,14.0879479865602));
#27761=CARTESIAN_POINT('Ctrl Pts',(0.332952583473522,-2.43059196910973,
14.2808552285121));
#27762=CARTESIAN_POINT('Ctrl Pts',(0.11979767247544,2.02594636783405,14.4737624704641));
#27763=CARTESIAN_POINT('Ctrl Pts',(3.67449769713561,4.72222958280794,14.666669712416));
#27764=CARTESIAN_POINT('Ctrl Pts',(7.9086056122021,3.31574856115804,14.8595769543679));
#27765=CARTESIAN_POINT('Ctrl Pts',(9.14336713327734,-0.97173089265201,15.0524841963199));
#27766=CARTESIAN_POINT('Ctrl Pts',(6.30599397187691,-4.41462580373721,15.2453914382718));
#27767=CARTESIAN_POINT('Ctrl Pts',(1.8616645866995,-4.02254734934239,15.4382986802237));
#27768=CARTESIAN_POINT('Ctrl Pts',(-0.328160969075848,-0.134322510611719,
15.6312059221757));
#27769=CARTESIAN_POINT('Ctrl Pts',(1.63898615201173,3.8682063840671,15.8241131641276));
#27770=CARTESIAN_POINT('Ctrl Pts',(6.05422526983221,4.51467240789339,16.0170204060795));
#27771=CARTESIAN_POINT('Ctrl Pts',(9.08106892242169,1.22887483102134,16.2099276480315));
#27772=CARTESIAN_POINT('Ctrl Pts',(8.41936777485122,-1.65782202753229,16.3385324759994));
#27773=CARTESIAN_POINT('Ctrl Pts',(7.55936623237133,-2.66073791153538,16.4028348899834));
#27774=CARTESIAN_POINT('Ctrl Pts',(5.45442072271799,3.72203409039186,10.8663421353436));
#27775=CARTESIAN_POINT('Ctrl Pts',(6.6574535524538,3.39947698103161,10.9306445493276));
#27776=CARTESIAN_POINT('Ctrl Pts',(8.70897306044462,1.50561293730781,11.0592493772955));
#27777=CARTESIAN_POINT('Ctrl Pts',(8.10293196746261,-2.66228732709529,11.2521566192475));
#27778=CARTESIAN_POINT('Ctrl Pts',(4.32335917937504,-4.50961769627978,11.4450638611994));
#27779=CARTESIAN_POINT('Ctrl Pts',(0.662104016089638,-2.44245862170941,
11.6379711031513));
#27780=CARTESIAN_POINT('Ctrl Pts',(0.296185113536645,1.74861810484191,11.8308783451033));
#27781=CARTESIAN_POINT('Ctrl Pts',(3.54555055284121,4.41951264571341,12.0237855870552));
#27782=CARTESIAN_POINT('Ctrl Pts',(7.58601133917742,3.25104010056242,12.216692829007));
#27783=CARTESIAN_POINT('Ctrl Pts',(8.90758666238144,-0.742288259422881,
12.4096000709591));
#27784=CARTESIAN_POINT('Ctrl Pts',(6.36178278245141,-4.09057107072706,12.602507312911));
#27785=CARTESIAN_POINT('Ctrl Pts',(2.16061806795178,-3.88487822222208,12.7954145548629));
#27786=CARTESIAN_POINT('Ctrl Pts',(-0.0458509299148173,-0.303832913883873,
12.9883217968149));
#27787=CARTESIAN_POINT('Ctrl Pts',(1.65946939863585,3.54117835721147,13.1812290387668));
#27788=CARTESIAN_POINT('Ctrl Pts',(5.79491816017005,4.30949332585313,13.3741362807187));
#27789=CARTESIAN_POINT('Ctrl Pts',(8.76747707074188,1.33356244236586,13.5670435226706));
#27790=CARTESIAN_POINT('Ctrl Pts',(7.99447527785278,-2.80101605226979,13.7599507646226));
#27791=CARTESIAN_POINT('Ctrl Pts',(4.14752708210266,-4.50196694207479,13.9528580065745));
#27792=CARTESIAN_POINT('Ctrl Pts',(0.568998129654688,-2.29145577170941,
14.1457652485264));
#27793=CARTESIAN_POINT('Ctrl Pts',(0.368045004949992,1.90997360180016,14.3386724904784));
#27794=CARTESIAN_POINT('Ctrl Pts',(3.71926067245942,4.45191145629663,14.5315797324303));
#27795=CARTESIAN_POINT('Ctrl Pts',(7.71099237540476,3.12594268168577,14.7244869743822));
#27796=CARTESIAN_POINT('Ctrl Pts',(8.87507151748671,-0.916105373017984,
14.9173942163342));
#27797=CARTESIAN_POINT('Ctrl Pts',(6.20012023408976,-4.16191607084762,15.1103014582861));
#27798=CARTESIAN_POINT('Ctrl Pts',(2.01020092617208,-3.7922816572134,15.303208700238));
#27799=CARTESIAN_POINT('Ctrl Pts',(-0.0542708044146682,-0.126633386485045,
15.49611594219));
#27800=CARTESIAN_POINT('Ctrl Pts',(1.8002694399805,3.64677574746549,15.6890231841419));
#27801=CARTESIAN_POINT('Ctrl Pts',(5.96276371651375,4.25623563227429,15.8819304260938));
#27802=CARTESIAN_POINT('Ctrl Pts',(8.81633948979692,1.15852942823789,16.0748376680458));
#27803=CARTESIAN_POINT('Ctrl Pts',(8.19251659684855,-1.56292207895646,16.2034424960137));
#27804=CARTESIAN_POINT('Ctrl Pts',(7.38174476708876,-2.50842729749781,16.2677449099977));
#27805=CARTESIAN_POINT('Ctrl Pts',(5.39382553479269,3.49603379995416,10.7312521553578));
#27806=CARTESIAN_POINT('Ctrl Pts',(6.52381073457038,3.19306221792327,10.7955545693418));
#27807=CARTESIAN_POINT('Ctrl Pts',(8.45076287069287,1.41419277487655,10.9241593973097));
#27808=CARTESIAN_POINT('Ctrl Pts',(7.8815203291762,-2.50063439900812,11.1170666392617));
#27809=CARTESIAN_POINT('Ctrl Pts',(4.33144155621419,-4.23579567198583,11.3099738812136));
#27810=CARTESIAN_POINT('Ctrl Pts',(0.892496213358695,-2.29415359696143,
11.5028811231655));
#27811=CARTESIAN_POINT('Ctrl Pts',(0.548795747350148,1.64244277437436,11.6957883651175));
#27812=CARTESIAN_POINT('Ctrl Pts',(3.60086113104353,4.15116176088335,11.8886956070694));
#27813=CARTESIAN_POINT('Ctrl Pts',(7.39598689651807,3.05363836024834,12.0816028490213));
#27814=CARTESIAN_POINT('Ctrl Pts',(8.6373167411408,-0.69721683929508,12.2745100909733));
#27815=CARTESIAN_POINT('Ctrl Pts',(6.24609296507032,-3.84219337520115,12.4674173329252));
#27816=CARTESIAN_POINT('Ctrl Pts',(2.30002114402498,-3.64899010695637,12.6603245748771));
#27817=CARTESIAN_POINT('Ctrl Pts',(0.227527983630383,-0.285384311556572,
12.8532318168291));
#27818=CARTESIAN_POINT('Ctrl Pts',(1.82930200385018,3.32615954819857,13.046139058781));
#27819=CARTESIAN_POINT('Ctrl Pts',(5.71364811599984,4.04782276625339,13.2390463007329));
#27820=CARTESIAN_POINT('Ctrl Pts',(8.50571454294112,1.25258911112488,13.4319535426849));
#27821=CARTESIAN_POINT('Ctrl Pts',(7.77964908256783,-2.63093957635364,13.6248607846368));
#27822=CARTESIAN_POINT('Ctrl Pts',(4.16628590738015,-4.22860946824717,13.8177680265887));
#27823=CARTESIAN_POINT('Ctrl Pts',(0.805043675835859,-2.15231957430909,
14.0106752685406));
#27824=CARTESIAN_POINT('Ctrl Pts',(0.616292337424535,1.79400083576627,14.2035825104926));
#27825=CARTESIAN_POINT('Ctrl Pts',(3.76402364778324,4.18159332978533,14.3964897524445));
#27826=CARTESIAN_POINT('Ctrl Pts',(7.51337913860741,2.93613680221351,14.5893969943964));
#27827=CARTESIAN_POINT('Ctrl Pts',(8.6067759016961,-0.860479853383961,14.7823042363484));
#27828=CARTESIAN_POINT('Ctrl Pts',(6.09424649630261,-3.90920633795803,14.9752114783003));
#27829=CARTESIAN_POINT('Ctrl Pts',(2.15873726564465,-3.56201596508441,15.1681187202522));
#27830=CARTESIAN_POINT('Ctrl Pts',(0.219619360246509,-0.11894426235837,
15.3610259622042));
#27831=CARTESIAN_POINT('Ctrl Pts',(1.96155272794927,3.42534511086389,15.5539332041561));
#27832=CARTESIAN_POINT('Ctrl Pts',(5.87130216319528,3.99779885665519,15.746840446108));
#27833=CARTESIAN_POINT('Ctrl Pts',(8.55161005717215,1.08818402545442,15.93974768806));
#27834=CARTESIAN_POINT('Ctrl Pts',(7.96566541884588,-1.46802213038064,16.0683525160279));
#27835=CARTESIAN_POINT('Ctrl Pts',(7.2041233018062,-2.35611668346024,16.1326549300119));
#27836=CARTESIAN_POINT('Ctrl Pts',(5.33323034686737,3.27003350951646,10.5961621753721));
#27837=CARTESIAN_POINT('Ctrl Pts',(6.39016791668697,2.98664745481493,10.6604645893561));
#27838=CARTESIAN_POINT('Ctrl Pts',(8.1925526809411,1.32277261244528,10.789069417324));
#27839=CARTESIAN_POINT('Ctrl Pts',(7.66010869088979,-2.33898147092094,10.981976659276));
#27840=CARTESIAN_POINT('Ctrl Pts',(4.33952393305334,-3.96197364769188,11.1748839012279));
#27841=CARTESIAN_POINT('Ctrl Pts',(1.12288841062775,-2.14584857221345,11.3677911431798));
#27842=CARTESIAN_POINT('Ctrl Pts',(0.801406381163646,1.53626744390679,11.5606983851318));
#27843=CARTESIAN_POINT('Ctrl Pts',(3.65617170924584,3.88281087605329,11.7536056270837));
#27844=CARTESIAN_POINT('Ctrl Pts',(7.20596245385872,2.85623661993425,11.9465128690356));
#27845=CARTESIAN_POINT('Ctrl Pts',(8.36704681990015,-0.652145419167273,
12.1394201109876));
#27846=CARTESIAN_POINT('Ctrl Pts',(6.13040314768924,-3.59381567967527,12.3323273529395));
#27847=CARTESIAN_POINT('Ctrl Pts',(2.43942422009817,-3.41310199169066,12.5252345948914));
#27848=CARTESIAN_POINT('Ctrl Pts',(0.50090689717559,-0.266935709229276,
12.7181418368434));
#27849=CARTESIAN_POINT('Ctrl Pts',(1.9991346090645,3.11114073918567,12.9110490787953));
#27850=CARTESIAN_POINT('Ctrl Pts',(5.63237807182963,3.78615220665366,13.1039563207472));
#27851=CARTESIAN_POINT('Ctrl Pts',(8.24395201514036,1.17161577988392,13.2968635626992));
#27852=CARTESIAN_POINT('Ctrl Pts',(7.56482288728288,-2.46086310043749,13.4897708046511));
#27853=CARTESIAN_POINT('Ctrl Pts',(4.18504473265764,-3.95525199441954,13.682678046603));
#27854=CARTESIAN_POINT('Ctrl Pts',(1.04108922201703,-2.01318337690878,13.875585288555));
#27855=CARTESIAN_POINT('Ctrl Pts',(0.864539669899084,1.67802806973238,14.0684925305069));
#27856=CARTESIAN_POINT('Ctrl Pts',(3.80878662310705,3.91127520327401,14.2613997724588));
#27857=CARTESIAN_POINT('Ctrl Pts',(7.31576590181006,2.74633092274124,14.4543070144107));
#27858=CARTESIAN_POINT('Ctrl Pts',(8.33848028590547,-0.804854333749936,
14.6472142563627));
#27859=CARTESIAN_POINT('Ctrl Pts',(5.98837275851547,-3.65649660506842,14.8401214983146));
#27860=CARTESIAN_POINT('Ctrl Pts',(2.30727360511723,-3.33175027295542,15.0330287402665));
#27861=CARTESIAN_POINT('Ctrl Pts',(0.493509524907691,-0.111255138231699,
15.2259359822185));
#27862=CARTESIAN_POINT('Ctrl Pts',(2.12283601591804,3.20391447426228,15.4188432241704));
#27863=CARTESIAN_POINT('Ctrl Pts',(5.77984060987681,3.73936208103607,15.6117504661223));
#27864=CARTESIAN_POINT('Ctrl Pts',(8.28688062454738,1.01783862267097,15.8046577080743));
#27865=CARTESIAN_POINT('Ctrl Pts',(7.73881424084322,-1.37312218180482,15.9332625360422));
#27866=CARTESIAN_POINT('Ctrl Pts',(7.02650183652363,-2.20380606942267,15.9975649500262));
#27867=CARTESIAN_POINT('Ctrl Pts',(7.02970353323295,-2.20655152809223,16.));
#27868=CARTESIAN_POINT('Ctrl Pts',(7.10742409212087,-2.13258453329759,16.));
#27869=CARTESIAN_POINT('Ctrl Pts',(7.18111417197279,-2.05488553445653,16.));
#27870=CARTESIAN_POINT('Ctrl Pts',(7.25077210344875,-1.97388604470357,16.));
#27871=CARTESIAN_POINT('Ctrl Pts',(7.32147126694797,-1.89167579171358,16.));
#27872=CARTESIAN_POINT('Ctrl Pts',(7.38801721163101,-1.80606513563107,16.));
#27873=CARTESIAN_POINT('Ctrl Pts',(7.45038163639419,-1.71745606959295,16.));
#27874=CARTESIAN_POINT('Ctrl Pts',(7.51427823638975,-1.62667004743177,16.));
#27875=CARTESIAN_POINT('Ctrl Pts',(7.57378581658663,-1.53273594286479,16.));
#27876=CARTESIAN_POINT('Ctrl Pts',(7.62883959427087,-1.43604272751087,16.));
#27877=CARTESIAN_POINT('Ctrl Pts',(7.67887899544011,-1.34815646798496,16.));
#27878=CARTESIAN_POINT('Ctrl Pts',(7.72523875431879,-1.25798988106563,16.));
#27879=CARTESIAN_POINT('Ctrl Pts',(7.76784147269646,-1.16581124461548,16.));
#27880=CARTESIAN_POINT('Ctrl Pts',(7.77520040295186,-1.14988887668907,16.));
#27881=CARTESIAN_POINT('Ctrl Pts',(7.78244716317746,-1.13390643103832,16.));
#27882=CARTESIAN_POINT('Ctrl Pts',(7.78958126330047,-1.11786523846045,16.));
#27883=CARTESIAN_POINT('Ctrl Pts',(7.80313988594662,-1.08737835529271,16.));
#27884=CARTESIAN_POINT('Ctrl Pts',(7.81627446676007,-1.05671763945313,16.));
#27885=CARTESIAN_POINT('Ctrl Pts',(7.82898177222437,-1.02590068301593,16.));
#27886=CARTESIAN_POINT('Ctrl Pts',(7.87265766117147,-0.91998066945996,16.));
#27887=CARTESIAN_POINT('Ctrl Pts',(7.91129968617478,-0.81219338233902,16.));
#27888=CARTESIAN_POINT('Ctrl Pts',(7.94486820109317,-0.702968480620349,
16.));
#27889=CARTESIAN_POINT('Ctrl Pts',(7.97877903504909,-0.592629744604231,
16.));
#27890=CARTESIAN_POINT('Ctrl Pts',(8.00751278739246,-0.480823171231237,
16.));
#27891=CARTESIAN_POINT('Ctrl Pts',(8.03098780517625,-0.367956851668526,
16.));
#27892=CARTESIAN_POINT('Ctrl Pts',(8.05439261017491,-0.255428110493012,
16.));
#27893=CARTESIAN_POINT('Ctrl Pts',(8.07257044534417,-0.14184511283469,16.));
#27894=CARTESIAN_POINT('Ctrl Pts',(8.08539428970214,-0.0275899139920535,
16.));
#27895=CARTESIAN_POINT('Ctrl Pts',(8.09322391903155,0.0421688752543764,
16.));
#27896=CARTESIAN_POINT('Ctrl Pts',(8.09905679884552,0.112178628330393,16.));
#27897=CARTESIAN_POINT('Ctrl Pts',(8.10285465082102,0.182354458664573,16.));
#27898=CARTESIAN_POINT('Ctrl Pts',(8.10369946176583,0.197964679892289,16.));
#27899=CARTESIAN_POINT('Ctrl Pts',(8.10444354709245,0.213583121772062,16.));
#27900=CARTESIAN_POINT('Ctrl Pts',(8.10508643441639,0.229208853518113,16.));
#27901=CARTESIAN_POINT('Ctrl Pts',(8.10577156413731,0.245861310071144,16.));
#27902=CARTESIAN_POINT('Ctrl Pts',(8.10634136964572,0.262512917881839,16.));
#27903=CARTESIAN_POINT('Ctrl Pts',(8.10679559189551,0.279159317031458,16.));
#27904=CARTESIAN_POINT('Ctrl Pts',(8.11003015880494,0.397700167629527,16.));
#27905=CARTESIAN_POINT('Ctrl Pts',(8.10740937540428,0.516026514847005,16.));
#27906=CARTESIAN_POINT('Ctrl Pts',(8.09886096480419,0.633712628060252,16.));
#27907=CARTESIAN_POINT('Ctrl Pts',(8.09088811444019,0.743474993775358,16.));
#27908=CARTESIAN_POINT('Ctrl Pts',(8.07775879624769,0.852681296150461,16.));
#27909=CARTESIAN_POINT('Ctrl Pts',(8.05937589245818,0.960999918180078,16.));
#27910=CARTESIAN_POINT('Ctrl Pts',(8.04008786670114,1.07465184148869,16.));
#27911=CARTESIAN_POINT('Ctrl Pts',(8.01501711848052,1.18732729300118,16.));
#27912=CARTESIAN_POINT('Ctrl Pts',(7.98446609980978,1.29875391107274,16.));
#27913=CARTESIAN_POINT('Ctrl Pts',(7.95574948852459,1.40349002191967,16.));
#27914=CARTESIAN_POINT('Ctrl Pts',(7.92219022346647,1.50712324170997,16.));
#27915=CARTESIAN_POINT('Ctrl Pts',(7.88399788919389,1.60942190462676,16.));
#27916=CARTESIAN_POINT('Ctrl Pts',(7.87627365071178,1.63011137762757,16.));
#27917=CARTESIAN_POINT('Ctrl Pts',(7.86835808505052,1.65075028704105,16.));
#27918=CARTESIAN_POINT('Ctrl Pts',(7.86026351666319,1.67131004319933,16.));
#27919=CARTESIAN_POINT('Ctrl Pts',(7.81704144668225,1.78109171121952,16.));
#27920=CARTESIAN_POINT('Ctrl Pts',(7.768671274096,1.88875360806527,16.));
#27921=CARTESIAN_POINT('Ctrl Pts',(7.71551213318849,1.99402239348199,16.));
#27922=CARTESIAN_POINT('Ctrl Pts',(7.66139636386624,2.10118554945464,16.));
#27923=CARTESIAN_POINT('Ctrl Pts',(7.60231745646377,2.2058693703916,16.));
#27924=CARTESIAN_POINT('Ctrl Pts',(7.53859928916297,2.30778248722832,16.));
#27925=CARTESIAN_POINT('Ctrl Pts',(7.47388703380901,2.41128558406915,16.));
#27926=CARTESIAN_POINT('Ctrl Pts',(7.40438930838696,2.51193162848434,16.));
#27927=CARTESIAN_POINT('Ctrl Pts',(7.33039364440775,2.60940116917617,16.));
#27928=CARTESIAN_POINT('Ctrl Pts',(7.28117391940481,2.67423502201329,16.));
#27929=CARTESIAN_POINT('Ctrl Pts',(7.22996301121353,2.73766311775236,16.));
#27930=CARTESIAN_POINT('Ctrl Pts',(7.17683430579202,2.79958539364976,16.));
#27931=CARTESIAN_POINT('Ctrl Pts',(7.15825036575696,2.82124524500472,16.));
#27932=CARTESIAN_POINT('Ctrl Pts',(7.13943170136375,2.84272080122415,16.));
#27933=CARTESIAN_POINT('Ctrl Pts',(7.12038121960424,2.8640075976673,16.));
#27934=CARTESIAN_POINT('Ctrl Pts',(7.10831155266906,2.8774941092647,16.));
#27935=CARTESIAN_POINT('Ctrl Pts',(7.09614841307943,2.89090530562956,16.));
#27936=CARTESIAN_POINT('Ctrl Pts',(7.08389379300337,2.90423864090636,16.));
#27937=CARTESIAN_POINT('Ctrl Pts',(6.99912039327998,2.99647423483355,16.));
#27938=CARTESIAN_POINT('Ctrl Pts',(6.91026281916338,3.08467093810845,16.));
#27939=CARTESIAN_POINT('Ctrl Pts',(6.81764603140261,3.16850597662426,16.));
#27940=CARTESIAN_POINT('Ctrl Pts',(6.72503476769201,3.25233601486993,16.));
#27941=CARTESIAN_POINT('Ctrl Pts',(6.6286642334695,3.33180568902751,16.));
#27942=CARTESIAN_POINT('Ctrl Pts',(6.52881466382487,3.40656649734515,16.));
#27943=CARTESIAN_POINT('Ctrl Pts',(6.48102994982806,3.44234455684349,16.));
#27944=CARTESIAN_POINT('Ctrl Pts',(6.43244783477714,3.47704370933109,16.));
#27945=CARTESIAN_POINT('Ctrl Pts',(6.38309593333529,3.51062285916835,16.));
#27946=CARTESIAN_POINT('Ctrl Pts',(6.36711687140756,3.52149505049339,16.));
#27947=CARTESIAN_POINT('Ctrl Pts',(6.35105838482246,3.53224887980621,16.));
#27948=CARTESIAN_POINT('Ctrl Pts',(6.33492937498319,3.54287787969292,16.));
#27949=CARTESIAN_POINT('Ctrl Pts',(6.22941110326806,3.61241430562871,16.));
#27950=CARTESIAN_POINT('Ctrl Pts',(6.12078554312154,3.67667379633101,16.));
#27951=CARTESIAN_POINT('Ctrl Pts',(6.00935069340048,3.73531275389524,16.));
#27952=CARTESIAN_POINT('Ctrl Pts',(5.94481649130472,3.76927177432383,16.));
#27953=CARTESIAN_POINT('Ctrl Pts',(5.87933933376081,3.80134522041433,16.));
#27954=CARTESIAN_POINT('Ctrl Pts',(5.81297142537859,3.83146067830186,16.));
#27955=CARTESIAN_POINT('Ctrl Pts',(5.71640347400647,3.87527986959057,16.));
#27956=CARTESIAN_POINT('Ctrl Pts',(5.61795023769426,3.91495500013133,16.));
#27957=CARTESIAN_POINT('Ctrl Pts',(5.51786475809797,3.95054587342593,16.));
#27958=CARTESIAN_POINT('Ctrl Pts',(5.51437352919122,3.94563850749837,11.));
#27959=CARTESIAN_POINT('Ctrl Pts',(5.62948494275764,3.90412601543845,11.));
#27960=CARTESIAN_POINT('Ctrl Pts',(5.74226321989584,3.85715435981311,11.));
#27961=CARTESIAN_POINT('Ctrl Pts',(5.8524831871461,3.80507072374339,11.));
#27962=CARTESIAN_POINT('Ctrl Pts',(5.96574275745869,3.75155074556939,11.));
#27963=CARTESIAN_POINT('Ctrl Pts',(6.07630162648715,3.69263244652674,11.));
#27964=CARTESIAN_POINT('Ctrl Pts',(6.18388799726991,3.62864544490519,11.));
#27965=CARTESIAN_POINT('Ctrl Pts',(6.29199231516529,3.56435039420182,11.));
#27966=CARTESIAN_POINT('Ctrl Pts',(6.39709603311487,3.49493702502777,11.));
#27967=CARTESIAN_POINT('Ctrl Pts',(6.49888670834379,3.42070219646027,11.));
#27968=CARTESIAN_POINT('Ctrl Pts',(6.59974286575969,3.34714890153508,11.));
#27969=CARTESIAN_POINT('Ctrl Pts',(6.69734700891971,3.26886154066444,11.));
#27970=CARTESIAN_POINT('Ctrl Pts',(6.79135148512373,3.18610284976544,11.));
#27971=CARTESIAN_POINT('Ctrl Pts',(6.80306946864777,3.17578669232714,11.));
#27972=CARTESIAN_POINT('Ctrl Pts',(6.81473145720267,3.16540103189161,11.));
#27973=CARTESIAN_POINT('Ctrl Pts',(6.82633672351556,3.15494635733385,11.));
#27974=CARTESIAN_POINT('Ctrl Pts',(6.83946660504027,3.14311822391392,11.));
#27975=CARTESIAN_POINT('Ctrl Pts',(6.85252435343711,3.13120123394603,11.));
#27976=CARTESIAN_POINT('Ctrl Pts',(6.86549714655421,3.11920720081751,11.));
#27977=CARTESIAN_POINT('Ctrl Pts',(6.95598471534232,3.03554665925432,11.));
#27978=CARTESIAN_POINT('Ctrl Pts',(7.04248228827934,2.94801566268217,11.));
#27979=CARTESIAN_POINT('Ctrl Pts',(7.12472970854843,2.85692463994827,11.));
#27980=CARTESIAN_POINT('Ctrl Pts',(7.20656942414708,2.76628516007472,11.));
#27981=CARTESIAN_POINT('Ctrl Pts',(7.28420148981919,2.67212013219767,11.));
#27982=CARTESIAN_POINT('Ctrl Pts',(7.35732724633003,2.57470655107058,11.));
#27983=CARTESIAN_POINT('Ctrl Pts',(7.42878936891669,2.47950915950476,11.));
#27984=CARTESIAN_POINT('Ctrl Pts',(7.49594817041181,2.38120865303378,11.));
#27985=CARTESIAN_POINT('Ctrl Pts',(7.55847906409492,2.28004647451056,11.));
#27986=CARTESIAN_POINT('Ctrl Pts',(7.60971100281839,2.19716369088204,11.));
#27987=CARTESIAN_POINT('Ctrl Pts',(7.65783567486646,2.11235952148364,11.));
#27988=CARTESIAN_POINT('Ctrl Pts',(7.70264873051723,2.02576258719893,11.));
#27989=CARTESIAN_POINT('Ctrl Pts',(7.71353509918498,2.00472572331116,11.));
#27990=CARTESIAN_POINT('Ctrl Pts',(7.72422592037529,1.98358305300933,11.));
#27991=CARTESIAN_POINT('Ctrl Pts',(7.73471803882108,1.96233641130778,11.));
#27992=CARTESIAN_POINT('Ctrl Pts',(7.74225005556775,1.94708400428115,11.));
#27993=CARTESIAN_POINT('Ctrl Pts',(7.74967980897516,1.93177757747585,11.));
#27994=CARTESIAN_POINT('Ctrl Pts',(7.75699964776382,1.91643178757063,11.));
#27995=CARTESIAN_POINT('Ctrl Pts',(7.808138962757,1.80921997506486,11.));
#27996=CARTESIAN_POINT('Ctrl Pts',(7.85399926743267,1.69992489457679,11.));
#27997=CARTESIAN_POINT('Ctrl Pts',(7.89429953689311,1.5888059933625,11.));
#27998=CARTESIAN_POINT('Ctrl Pts',(7.93459980635355,1.47768709214822,11.));
#27999=CARTESIAN_POINT('Ctrl Pts',(7.96934048693593,1.36474370484422,11.));
#28000=CARTESIAN_POINT('Ctrl Pts',(7.99818591109683,1.25022313396199,11.));
#28001=CARTESIAN_POINT('Ctrl Pts',(8.027156518052,1.13520556899906,11.));
#28002=CARTESIAN_POINT('Ctrl Pts',(8.05018003397215,1.01859603432461,11.));
#28003=CARTESIAN_POINT('Ctrl Pts',(8.0673371330803,0.900832334980842,11.));
#28004=CARTESIAN_POINT('Ctrl Pts',(8.08181548590596,0.801455139663204,11.));
#28005=CARTESIAN_POINT('Ctrl Pts',(8.09211525472638,0.701255765578224,11.));
#28006=CARTESIAN_POINT('Ctrl Pts',(8.09825716826101,0.60050527517124,11.));
#28007=CARTESIAN_POINT('Ctrl Pts',(8.09932328478395,0.583016953020385,11.));
#28008=CARTESIAN_POINT('Ctrl Pts',(8.10026414720376,0.565510267575662,11.));
#28009=CARTESIAN_POINT('Ctrl Pts',(8.1010795331039,0.547992282113394,11.));
#28010=CARTESIAN_POINT('Ctrl Pts',(8.10648399092696,0.431881354074675,11.));
#28011=CARTESIAN_POINT('Ctrl Pts',(8.10636428859241,0.315647778133886,11.));
#28012=CARTESIAN_POINT('Ctrl Pts',(8.10085587731003,0.199697504383908,11.));
#28013=CARTESIAN_POINT('Ctrl Pts',(8.0953258767411,0.0832927831430958,11.));
#28014=CARTESIAN_POINT('Ctrl Pts',(8.08436455465527,-0.0328273338256495,
11.));
#28015=CARTESIAN_POINT('Ctrl Pts',(8.06805684234805,-0.148243610557007,
11.));
#28016=CARTESIAN_POINT('Ctrl Pts',(8.05200822940878,-0.261826136251509,
11.));
#28017=CARTESIAN_POINT('Ctrl Pts',(8.03078135261771,-0.374727803014246,
11.));
#28018=CARTESIAN_POINT('Ctrl Pts',(8.00441224541771,-0.486528165984565,
11.));
#28019=CARTESIAN_POINT('Ctrl Pts',(7.97876322263963,-0.59527549803015,11.));
#28020=CARTESIAN_POINT('Ctrl Pts',(7.94824856031495,-0.702981455818624,
11.));
#28021=CARTESIAN_POINT('Ctrl Pts',(7.91286477097122,-0.809229140047758,
11.));
#28022=CARTESIAN_POINT('Ctrl Pts',(7.90675311367846,-0.827580748120317,
11.));
#28023=CARTESIAN_POINT('Ctrl Pts',(7.90049538834023,-0.845890636222599,
11.));
#28024=CARTESIAN_POINT('Ctrl Pts',(7.89409748850863,-0.864139946124484,
11.));
#28025=CARTESIAN_POINT('Ctrl Pts',(7.85663138122071,-0.971007921665021,
11.));
#28026=CARTESIAN_POINT('Ctrl Pts',(7.81432308576492,-1.07592082129095,11.));
#28027=CARTESIAN_POINT('Ctrl Pts',(7.76722270160403,-1.17846998810213,11.));
#28028=CARTESIAN_POINT('Ctrl Pts',(7.72124936093314,-1.27856530293484,11.));
#28029=CARTESIAN_POINT('Ctrl Pts',(7.6707100968929,-1.3764092536002,11.));
#28030=CARTESIAN_POINT('Ctrl Pts',(7.61561456328355,-1.47158897695947,11.));
#28031=CARTESIAN_POINT('Ctrl Pts',(7.59591034615304,-1.505628794938,11.));
#28032=CARTESIAN_POINT('Ctrl Pts',(7.57562304223414,-1.53932749284057,11.));
#28033=CARTESIAN_POINT('Ctrl Pts',(7.55475205970316,-1.57266491022023,11.));
#28034=CARTESIAN_POINT('Ctrl Pts',(7.54414531802266,-1.58960715881424,11.));
#28035=CARTESIAN_POINT('Ctrl Pts',(7.53338923224129,-1.60645371256413,11.));
#28036=CARTESIAN_POINT('Ctrl Pts',(7.52248968612946,-1.62319323259679,11.));
#28037=CARTESIAN_POINT('Ctrl Pts',(7.46367863799964,-1.71351522474309,11.));
#28038=CARTESIAN_POINT('Ctrl Pts',(7.40064685851406,-1.8007992593941,11.));
#28039=CARTESIAN_POINT('Ctrl Pts',(7.33341540428026,-1.88466061294003,11.));
#28040=CARTESIAN_POINT('Ctrl Pts',(7.29706350713731,-1.93000425949821,11.));
#28041=CARTESIAN_POINT('Ctrl Pts',(7.25948321883399,-1.974346648915,11.));
#28042=CARTESIAN_POINT('Ctrl Pts',(7.22067388828633,-2.01762194562246,11.));
#28043=CARTESIAN_POINT('Ctrl Pts',(7.16129250757508,-2.08383661186161,11.));
#28044=CARTESIAN_POINT('Ctrl Pts',(7.09903390488877,-2.14755395179585,11.));
#28045=CARTESIAN_POINT('Ctrl Pts',(7.03410086753636,-2.20867914885338,11.));
#28046=CARTESIAN_POINT('Origin',(4.45646910621825,4.66293670342566E-15,
11.));
#28047=CARTESIAN_POINT('',(-2.54353089378178,4.0414518843274,11.));
#28048=CARTESIAN_POINT('',(-2.54353089378178,-4.04145188432739,11.));
#28049=CARTESIAN_POINT('',(-2.54353089378178,4.0414518843274,11.));
#28050=CARTESIAN_POINT('',(4.45646910621825,8.0829037686548,11.));
#28051=CARTESIAN_POINT('',(4.45646910621825,8.0829037686548,11.));
#28052=CARTESIAN_POINT('',(11.4564691062183,4.0414518843274,11.));
#28053=CARTESIAN_POINT('',(11.4564691062183,4.0414518843274,11.));
#28054=CARTESIAN_POINT('',(11.4564691062183,-4.04145188432739,11.));
#28055=CARTESIAN_POINT('',(11.4564691062183,-4.04145188432739,11.));
#28056=CARTESIAN_POINT('',(4.45646910621825,-8.08290376865479,11.));
#28057=CARTESIAN_POINT('',(4.45646910621825,-8.08290376865479,11.));
#28058=CARTESIAN_POINT('',(-2.54353089378178,-4.04145188432739,11.));
#28059=CARTESIAN_POINT('Origin',(4.45646910621825,-8.08290376865479,11.));
#28060=CARTESIAN_POINT('',(4.45646910621825,-8.08290376865479,16.));
#28061=CARTESIAN_POINT('',(4.45646910621825,-8.08290376865479,11.));
#28062=CARTESIAN_POINT('',(-2.54353089378178,-4.04145188432739,16.));
#28063=CARTESIAN_POINT('',(-2.54353089378178,-4.04145188432739,16.));
#28064=CARTESIAN_POINT('',(-2.54353089378178,-4.04145188432739,11.));
#28065=CARTESIAN_POINT('Origin',(11.4564691062183,-4.04145188432739,11.));
#28066=CARTESIAN_POINT('',(11.4564691062183,-4.04145188432739,16.));
#28067=CARTESIAN_POINT('',(11.4564691062183,-4.04145188432739,11.));
#28068=CARTESIAN_POINT('',(4.45646910621825,-8.08290376865479,16.));
#28069=CARTESIAN_POINT('Origin',(11.4564691062183,4.0414518843274,11.));
#28070=CARTESIAN_POINT('',(11.4564691062183,4.0414518843274,16.));
#28071=CARTESIAN_POINT('',(11.4564691062183,4.0414518843274,11.));
#28072=CARTESIAN_POINT('',(11.4564691062183,-4.04145188432739,16.));
#28073=CARTESIAN_POINT('Origin',(4.45646910621825,8.0829037686548,11.));
#28074=CARTESIAN_POINT('',(4.45646910621825,8.0829037686548,16.));
#28075=CARTESIAN_POINT('',(4.45646910621825,8.0829037686548,11.));
#28076=CARTESIAN_POINT('',(11.4564691062183,4.0414518843274,16.));
#28077=CARTESIAN_POINT('Origin',(-2.54353089378178,4.0414518843274,11.));
#28078=CARTESIAN_POINT('',(-2.54353089378178,4.0414518843274,16.));
#28079=CARTESIAN_POINT('',(-2.54353089378178,4.0414518843274,11.));
#28080=CARTESIAN_POINT('',(4.45646910621825,8.0829037686548,16.));
#28081=CARTESIAN_POINT('Origin',(-2.54353089378178,-4.04145188432739,11.));
#28082=CARTESIAN_POINT('',(-2.54353089378178,4.0414518843274,16.));
#28083=CARTESIAN_POINT('Origin',(4.45646910621825,5.77315972805081E-15,
16.));
#28084=CARTESIAN_POINT('',(0.,0.,0.));
#28085=CARTESIAN_POINT('Origin',(206.833344075386,0.,0.));
#28086=CARTESIAN_POINT('',(206.833344075386,-5.,-6.12323399573677E-16));
#28087=CARTESIAN_POINT('Origin',(206.833344075386,0.,0.));
#28088=CARTESIAN_POINT('',(25.8804751042881,-5.,-6.12323399573677E-16));
#28089=CARTESIAN_POINT('',(206.833344075386,-5.,6.12323399573677E-16));
#28090=CARTESIAN_POINT('Origin',(25.8804751042881,0.,0.));
#28091=CARTESIAN_POINT('Origin',(117.321733117655,0.,0.));
#28092=CARTESIAN_POINT('',(204.333344075386,-1.29063339878982E-15,10.5388214764323));
#28093=CARTESIAN_POINT('Origin',(204.333344075386,0.,0.));
#28094=CARTESIAN_POINT('',(30.3101221599236,-1.29063339878982E-15,10.5388214764323));
#28095=CARTESIAN_POINT('',(117.321733117655,-1.29063339878982E-15,10.5388214764323));
#28096=CARTESIAN_POINT('Origin',(30.3101221599236,0.,0.));
#28097=CARTESIAN_POINT('Origin',(204.333344075386,0.,0.));
#28098=CARTESIAN_POINT('',(206.833344075386,-9.8447169900298E-16,8.03882147643229));
#28099=CARTESIAN_POINT('Origin',(206.833344075386,0.,0.));
#28100=CARTESIAN_POINT('Origin',(204.333344075386,-9.84471699002983E-16,
8.03882147643231));
#28101=CARTESIAN_POINT('Origin',(206.833344075386,0.,0.));
#28102=CARTESIAN_POINT('Origin',(25.8804751042881,0.,-5.78096926885272));
#28103=CARTESIAN_POINT('',(25.8804751042881,-7.0796455110697E-16,5.78096926885272));
#28104=CARTESIAN_POINT('Origin',(25.8804751042881,0.,0.));
#28105=CARTESIAN_POINT('Origin',(30.9381335663634,0.,0.));
#28106=CARTESIAN_POINT('',(27.0054474704383,-1.09743090720644E-15,8.96120340959139));
#28107=CARTESIAN_POINT('Origin',(27.0054474704383,0.,0.));
#28108=CARTESIAN_POINT('Origin',(30.9381335663634,-7.07964551106969E-16,
5.78096926885271));
#28109=CARTESIAN_POINT('Origin',(30.3101221599236,0.,0.));
#28110=CARTESIAN_POINT('Origin',(30.3101221599236,-7.70158509152195E-16,
6.2888214764323));
#28111=CARTESIAN_POINT('',(0.,0.,0.));
#28112=CARTESIAN_POINT('Origin',(370.834317853224,-8.23961502859548,0.));
#28113=CARTESIAN_POINT('',(373.320592904309,-15.4531286062585,-3.24124379989413));
#28114=CARTESIAN_POINT('',(373.320108995548,-15.5571531246989,-3.24059684932977));
#28115=CARTESIAN_POINT('',(373.320592904309,-8.23961502859548,-3.24124379989413));
#28116=CARTESIAN_POINT('',(371.892222276197,-16.,3.94563850749836));
#28117=CARTESIAN_POINT('Ctrl Pts',(373.320108995548,-15.5571531246989,-3.24059684932998));
#28118=CARTESIAN_POINT('Ctrl Pts',(373.632190344584,-15.5761639218313,-3.0053442006562));
#28119=CARTESIAN_POINT('Ctrl Pts',(374.850886074702,-15.6594771329477,-1.78563323199014));
#28120=CARTESIAN_POINT('Ctrl Pts',(375.341784615062,-15.8070927580481,1.59206573694299));
#28121=CARTESIAN_POINT('Ctrl Pts',(373.167528343663,-15.935697586016,3.60370350081893));
#28122=CARTESIAN_POINT('Ctrl Pts',(371.892222276197,-16.,3.94563850749836));
#28123=CARTESIAN_POINT('',(369.775300062574,-16.,3.94533982301726));
#28124=CARTESIAN_POINT('Origin',(370.834317853224,-16.,0.));
#28125=CARTESIAN_POINT('Ctrl Pts',(373.320592904309,-15.4531286062585,-3.2412437998941));
#28126=CARTESIAN_POINT('Ctrl Pts',(373.415273543652,-15.4589570255755,-3.16861670796533));
#28127=CARTESIAN_POINT('Ctrl Pts',(373.506888457287,-15.4647854448925,-3.09174615098767));
#28128=CARTESIAN_POINT('Ctrl Pts',(373.595037865624,-15.4706138642095,-3.01092178794732));
#28129=CARTESIAN_POINT('Ctrl Pts',(373.683101628257,-15.4764366206516,-2.93017595361797));
#28130=CARTESIAN_POINT('Ctrl Pts',(373.767706286925,-15.4822593770937,-2.84548422952368));
#28131=CARTESIAN_POINT('Ctrl Pts',(373.848484213075,-15.4880821335358,-2.75717720778772));
#28132=CARTESIAN_POINT('Ctrl Pts',(373.930386713752,-15.493985953257,-2.66764079292362));
#28133=CARTESIAN_POINT('Ctrl Pts',(374.008354785899,-15.4998897729783,-2.57438791056201));
#28134=CARTESIAN_POINT('Ctrl Pts',(374.082042785605,-15.5057935926996,-2.47780301145807));
#28135=CARTESIAN_POINT('Ctrl Pts',(374.154641056606,-15.511610104286,-2.38264644990447));
#28136=CARTESIAN_POINT('Ctrl Pts',(374.223084739107,-15.5174266158724,-2.28425609165628));
#28137=CARTESIAN_POINT('Ctrl Pts',(374.287083509277,-15.5232431274588,-2.18303328521979));
#28138=CARTESIAN_POINT('Ctrl Pts',(374.351073491281,-15.5290588403349,-2.08182437847084));
#28139=CARTESIAN_POINT('Ctrl Pts',(374.410619558004,-15.5348745532111,-1.97778414053954));
#28140=CARTESIAN_POINT('Ctrl Pts',(374.465475094,-15.5406902660872,-1.87134232377645));
#28141=CARTESIAN_POINT('Ctrl Pts',(374.520335880489,-15.5465065356138,-1.76489031894469));
#28142=CARTESIAN_POINT('Ctrl Pts',(374.570505057529,-15.5523228051403,-1.65603663942584));
#28143=CARTESIAN_POINT('Ctrl Pts',(374.615782577735,-15.5581390746669,-1.54523446029321));
#28144=CARTESIAN_POINT('Ctrl Pts',(374.662253415828,-15.5641086356818,-1.43151201914736));
#28145=CARTESIAN_POINT('Ctrl Pts',(374.703570979475,-15.5700781966968,-1.31573735489747));
#28146=CARTESIAN_POINT('Ctrl Pts',(374.739572660431,-15.5760477577118,-1.19841974732692));
#28147=CARTESIAN_POINT('Ctrl Pts',(374.774699352152,-15.5818722337892,-1.08395344116946));
#28148=CARTESIAN_POINT('Ctrl Pts',(374.80476554543,-15.5876967098667,-0.968018744102296));
#28149=CARTESIAN_POINT('Ctrl Pts',(374.829671745781,-15.5935211859442,-0.851100624619647));
#28150=CARTESIAN_POINT('Ctrl Pts',(374.855508548595,-15.5995632894279,-0.729813942756243));
#28151=CARTESIAN_POINT('Ctrl Pts',(374.875792168291,-15.6056053929116,-0.60746939833637));
#28152=CARTESIAN_POINT('Ctrl Pts',(374.890470404658,-15.6116474963953,-0.484614774322597));
#28153=CARTESIAN_POINT('Ctrl Pts',(374.905148641026,-15.617689599879,-0.361760150308814));
#28154=CARTESIAN_POINT('Ctrl Pts',(374.914221521336,-15.6237317033627,-0.238395931624845));
#28155=CARTESIAN_POINT('Ctrl Pts',(374.917696855934,-15.6297738068464,-0.115069197545622));
#28156=CARTESIAN_POINT('Ctrl Pts',(374.921059702466,-15.6356203422434,0.00426575230112755));
#28157=CARTESIAN_POINT('Ctrl Pts',(374.919191970017,-15.6414668776404,0.123925603645873));
#28158=CARTESIAN_POINT('Ctrl Pts',(374.912059029124,-15.6473134130375,0.243417136549867));
#28159=CARTESIAN_POINT('Ctrl Pts',(374.90493468769,-15.6531528998641,0.362764610721632));
#28160=CARTESIAN_POINT('Ctrl Pts',(374.892557790066,-15.6589923866908,0.48194376948902));
#28161=CARTESIAN_POINT('Ctrl Pts',(374.874945688179,-15.6648318735175,0.600459573481934));
#28162=CARTESIAN_POINT('Ctrl Pts',(374.857350341039,-15.6706658051229,0.718862631006505));
#28163=CARTESIAN_POINT('Ctrl Pts',(374.834529758843,-15.6764997367283,0.836603191362777));
#28164=CARTESIAN_POINT('Ctrl Pts',(374.806553203294,-15.6823336683337,0.953190077398779));
#28165=CARTESIAN_POINT('Ctrl Pts',(374.778510105951,-15.688181475853,1.07005426349758));
#28166=CARTESIAN_POINT('Ctrl Pts',(374.745286515245,-15.6940292833724,1.18575887267738));
#28167=CARTESIAN_POINT('Ctrl Pts',(374.707004094485,-15.6998770908917,1.29981778597958));
#28168=CARTESIAN_POINT('Ctrl Pts',(374.66885220236,-15.7057049595901,1.4134878013487));
#28169=CARTESIAN_POINT('Ctrl Pts',(374.625676053758,-15.7115328282884,1.52552294033343));
#28170=CARTESIAN_POINT('Ctrl Pts',(374.577646205178,-15.7173606969868,1.63545646516599));
#28171=CARTESIAN_POINT('Ctrl Pts',(374.529622648448,-15.7231878022419,1.74537558884905));
#28172=CARTESIAN_POINT('Ctrl Pts',(374.476746818621,-15.7290149074969,1.8531932755489));
#28173=CARTESIAN_POINT('Ctrl Pts',(374.419237275813,-15.734842012752,1.95846310497352));
#28174=CARTESIAN_POINT('Ctrl Pts',(374.361722022948,-15.7406696965738,2.06374338652139));
#28175=CARTESIAN_POINT('Ctrl Pts',(374.299572336272,-15.7464973803957,2.1664749528619));
#28176=CARTESIAN_POINT('Ctrl Pts',(374.233052264084,-15.7523250642175,2.26623683767535));
#28177=CARTESIAN_POINT('Ctrl Pts',(374.166129090197,-15.7581880629326,2.36660326460515));
#28178=CARTESIAN_POINT('Ctrl Pts',(374.094782607174,-15.7640510616476,2.46396354777857));
#28179=CARTESIAN_POINT('Ctrl Pts',(374.019324687262,-15.7699140603627,2.55792034026346));
#28180=CARTESIAN_POINT('Ctrl Pts',(373.944218004903,-15.7757497682999,2.65143978761619));
#28181=CARTESIAN_POINT('Ctrl Pts',(373.86503838664,-15.7815854762372,2.741587089664));
#28182=CARTESIAN_POINT('Ctrl Pts',(373.782131823879,-15.7874211841744,2.82800597496021));
#28183=CARTESIAN_POINT('Ctrl Pts',(373.698643690396,-15.7932978282784,2.91503106912336));
#28184=CARTESIAN_POINT('Ctrl Pts',(373.611376425383,-15.7991744723824,2.99827494940356));
#28185=CARTESIAN_POINT('Ctrl Pts',(373.520718043089,-15.8050511164864,3.07741433997664));
#28186=CARTESIAN_POINT('Ctrl Pts',(373.430059660795,-15.8109277605903,3.15655373054971));
#28187=CARTESIAN_POINT('Ctrl Pts',(373.336010517313,-15.8168044046943,3.23158841461434));
#28188=CARTESIAN_POINT('Ctrl Pts',(373.23898831715,-15.8226810487983,3.30223938561709));
#28189=CARTESIAN_POINT('Ctrl Pts',(373.14367593233,-15.8284541292206,3.37164527957541));
#28190=CARTESIAN_POINT('Ctrl Pts',(373.045197520102,-15.8342272096428,3.43703669014109));
#28191=CARTESIAN_POINT('Ctrl Pts',(372.943929058018,-15.8400002900651,3.49810885545434));
#28192=CARTESIAN_POINT('Ctrl Pts',(372.842781908308,-15.84576645475,3.55910786068212));
#28193=CARTESIAN_POINT('Ctrl Pts',(372.738851707931,-15.8515326194349,3.61579769575302));
#28194=CARTESIAN_POINT('Ctrl Pts',(372.632545764179,-15.8572987841198,3.66791512718899));
#28195=CARTESIAN_POINT('Ctrl Pts',(372.52292648619,-15.8632446681148,3.72165695011128));
#28196=CARTESIAN_POINT('Ctrl Pts',(372.410781293761,-15.8691905521098,3.77053639578871));
#28197=CARTESIAN_POINT('Ctrl Pts',(372.296587589712,-15.8751364361048,3.81431412153638));
#28198=CARTESIAN_POINT('Ctrl Pts',(372.186018218221,-15.8808936068855,3.85670240959074));
#28199=CARTESIAN_POINT('Ctrl Pts',(372.073528818251,-15.8866507776661,3.89430774825955));
#28200=CARTESIAN_POINT('Ctrl Pts',(371.959575171876,-15.8924079484468,3.92696077989325));
#28201=CARTESIAN_POINT('Ctrl Pts',(371.845655452231,-15.8981634051798,3.95960408993736));
#28202=CARTESIAN_POINT('Ctrl Pts',(371.730272752571,-15.9039188619129,3.98729790965033));
#28203=CARTESIAN_POINT('Ctrl Pts',(371.61389866535,-15.9096743186459,4.00992253757668));
#28204=CARTESIAN_POINT('Ctrl Pts',(371.497530543038,-15.9154294803753,4.03254600584747));
#28205=CARTESIAN_POINT('Ctrl Pts',(371.38017154287,-15.9211846421047,4.05010072040834));
#28206=CARTESIAN_POINT('Ctrl Pts',(371.262303377542,-15.9269398038341,4.06251810961796));
#28207=CARTESIAN_POINT('Ctrl Pts',(371.1444122023,-15.932696089071,4.07493792291771));
#28208=CARTESIAN_POINT('Ctrl Pts',(371.026012078188,-15.938452374308,4.08221837474753));
#28209=CARTESIAN_POINT('Ctrl Pts',(370.907589015783,-15.944208659545,4.08434282801249));
#28210=CARTESIAN_POINT('Ctrl Pts',(370.789055146843,-15.9499703308444,4.08646926909384));
#28211=CARTESIAN_POINT('Ctrl Pts',(370.670498713169,-15.9557320021439,4.08343007586418));
#28212=CARTESIAN_POINT('Ctrl Pts',(370.552404864861,-15.9614936734434,4.07526073607468));
#28213=CARTESIAN_POINT('Ctrl Pts',(370.434244414927,-15.9672585941643,4.06708678900614));
#28214=CARTESIAN_POINT('Ctrl Pts',(370.316547482495,-15.9730235148852,4.05377698180414));
#28215=CARTESIAN_POINT('Ctrl Pts',(370.199791598557,-15.9787884356061,4.03541837138828));
#28216=CARTESIAN_POINT('Ctrl Pts',(370.082884002566,-15.9845608472381,4.01703590587935));
#28217=CARTESIAN_POINT('Ctrl Pts',(369.966920301436,-15.9903332588702,3.9935916289543));
#28218=CARTESIAN_POINT('Ctrl Pts',(369.852365342942,-15.9961056705023,3.96522310438524));
#28219=CARTESIAN_POINT('Ctrl Pts',(369.826604027313,-15.9974037803348,3.9588435419032));
#28220=CARTESIAN_POINT('Ctrl Pts',(369.800913882548,-15.9987018901674,3.95221514738881));
#28221=CARTESIAN_POINT('Ctrl Pts',(369.775300062574,-16.,3.94533982301725));
#28222=CARTESIAN_POINT('Origin',(370.834317853224,-8.23961502859548,0.));
#28223=CARTESIAN_POINT('',(373.320592904309,-14.2030090365224,-3.2412437998941));
#28224=CARTESIAN_POINT('',(373.320592904309,-14.3073933031112,-3.24124379989411));
#28225=CARTESIAN_POINT('',(373.320592904309,-8.23961502859548,-3.24124379989413));
#28226=CARTESIAN_POINT('',(366.750998120586,-15.114615009128,0.00158342508104396));
#28227=CARTESIAN_POINT('Ctrl Pts',(373.320592904309,-14.3073933031112,-3.2412437998941));
#28228=CARTESIAN_POINT('Ctrl Pts',(373.4155069276,-14.3132174492802,-3.16843768511984));
#28229=CARTESIAN_POINT('Ctrl Pts',(373.507298072945,-14.3190415954492,-3.09139940002156));
#28230=CARTESIAN_POINT('Ctrl Pts',(373.59557351228,-14.3248657416181,-3.01043056477479));
#28231=CARTESIAN_POINT('Ctrl Pts',(373.683804553304,-14.3306869585209,-2.92950245296831));
#28232=CARTESIAN_POINT('Ctrl Pts',(373.76852310731,-14.3365081754237,-2.84464799703066));
#28233=CARTESIAN_POINT('Ctrl Pts',(373.849369841393,-14.3423293923265,-2.75620872007897));
#28234=CARTESIAN_POINT('Ctrl Pts',(373.93019681244,-14.3481491862292,-2.66779106216471));
#28235=CARTESIAN_POINT('Ctrl Pts',(374.007153572486,-14.3539689801318,-2.57579062537674));
#28236=CARTESIAN_POINT('Ctrl Pts',(374.079918454935,-14.3597887740345,-2.48058495806416));
#28237=CARTESIAN_POINT('Ctrl Pts',(374.152682438597,-14.3656084960515,-2.385380466724));
#28238=CARTESIAN_POINT('Ctrl Pts',(374.221254401612,-14.3714282180685,-2.28697114614182));
#28239=CARTESIAN_POINT('Ctrl Pts',(374.285354079822,-14.3772479400855,-2.18576621867654));
#28240=CARTESIAN_POINT('Ctrl Pts',(374.349467843428,-14.3830689409403,-2.08453905223224));
#28241=CARTESIAN_POINT('Ctrl Pts',(374.409107150774,-14.388889941795,-1.98051539983543));
#28242=CARTESIAN_POINT('Ctrl Pts',(374.464036361265,-14.3947109426497,-1.87413141278375));
#28243=CARTESIAN_POINT('Ctrl Pts',(374.519020910212,-14.4005378078742,-1.76764024914006));
#28244=CARTESIAN_POINT('Ctrl Pts',(374.569285700624,-14.4063646730986,-1.65878436344289));
#28245=CARTESIAN_POINT('Ctrl Pts',(374.614642079508,-14.4121915383231,-1.548022527023));
#28246=CARTESIAN_POINT('Ctrl Pts',(374.66002376523,-14.4180216546786,-1.43719889043583));
#28247=CARTESIAN_POINT('Ctrl Pts',(374.700491445895,-14.4238517710341,-1.32446756583434));
#28248=CARTESIAN_POINT('Ctrl Pts',(374.735905990116,-14.4296818873896,-1.21030368505693));
#28249=CARTESIAN_POINT('Ctrl Pts',(374.77137150327,-14.4355203945013,-1.09597549858901));
#28250=CARTESIAN_POINT('Ctrl Pts',(374.801769252405,-14.4413589016131,-0.980211030222186));
#28251=CARTESIAN_POINT('Ctrl Pts',(374.827010887024,-14.4471974087248,-0.863497155665468));
#28252=CARTESIAN_POINT('Ctrl Pts',(374.840765699463,-14.4503789606114,-0.799896779631017));
#28253=CARTESIAN_POINT('Ctrl Pts',(374.852990336374,-14.4535605124979,-0.73601461623384));
#28254=CARTESIAN_POINT('Ctrl Pts',(374.863676992061,-14.4567420643845,-0.671930003997587));
#28255=CARTESIAN_POINT('Ctrl Pts',(374.883288111445,-14.4625805414257,-0.554328107007071));
#28256=CARTESIAN_POINT('Ctrl Pts',(374.897776039763,-14.4684190184669,-0.435689439637863));
#28257=CARTESIAN_POINT('Ctrl Pts',(374.907038673679,-14.4742574955081,-0.31649663289538));
#28258=CARTESIAN_POINT('Ctrl Pts',(374.916290115743,-14.4800889180371,-0.197447844379272));
#28259=CARTESIAN_POINT('Ctrl Pts',(374.920328791936,-14.4859203405661,-0.0778466497980785));
#28260=CARTESIAN_POINT('Ctrl Pts',(374.919103830164,-14.4917517630952,0.0418153392558642));
#28261=CARTESIAN_POINT('Ctrl Pts',(374.917880034403,-14.4975776348342,0.161363424959726));
#28262=CARTESIAN_POINT('Ctrl Pts',(374.911402573918,-14.5034035065733,0.280971786323991));
#28263=CARTESIAN_POINT('Ctrl Pts',(374.899672523021,-14.5092293783124,0.400145484495215));
#28264=CARTESIAN_POINT('Ctrl Pts',(374.887892219456,-14.5150802086468,0.519829734259205));
#28265=CARTESIAN_POINT('Ctrl Pts',(374.870814186672,-14.5209310389811,0.639075174990034));
#28266=CARTESIAN_POINT('Ctrl Pts',(374.84849245484,-14.5267818693154,0.757381850679897));
#28267=CARTESIAN_POINT('Ctrl Pts',(374.826288831582,-14.5326017417821,0.875062543012515));
#28268=CARTESIAN_POINT('Ctrl Pts',(374.798896951249,-14.5384216142487,0.991813979705609));
#28269=CARTESIAN_POINT('Ctrl Pts',(374.766421677012,-14.5442414867153,1.10715153386956));
#28270=CARTESIAN_POINT('Ctrl Pts',(374.733950446182,-14.5500606345657,1.22247472767258));
#28271=CARTESIAN_POINT('Ctrl Pts',(374.696397190473,-14.555879782416,1.33638399867441));
#28272=CARTESIAN_POINT('Ctrl Pts',(374.653917103434,-14.5616989302664,1.44840828767009));
#28273=CARTESIAN_POINT('Ctrl Pts',(374.611432441427,-14.5675187048202,1.56044464132213));
#28274=CARTESIAN_POINT('Ctrl Pts',(374.564020036959,-14.5733384793741,1.6705952299558));
#28275=CARTESIAN_POINT('Ctrl Pts',(374.511883617558,-14.579158253928,1.77840800970994));
#28276=CARTESIAN_POINT('Ctrl Pts',(374.459259141037,-14.5850325082954,1.88723004163998));
#28277=CARTESIAN_POINT('Ctrl Pts',(374.401821921722,-14.5909067626628,1.9936698853835));
#28278=CARTESIAN_POINT('Ctrl Pts',(374.339828846594,-14.5967810170301,2.09728817174922));
#28279=CARTESIAN_POINT('Ctrl Pts',(374.278324033849,-14.6026090053037,2.20009035226406));
#28280=CARTESIAN_POINT('Ctrl Pts',(374.212335148662,-14.6084369935772,2.30011495408861));
#28281=CARTESIAN_POINT('Ctrl Pts',(374.142156033178,-14.6142649818508,2.39696298995966));
#28282=CARTESIAN_POINT('Ctrl Pts',(374.071141231333,-14.6201623692651,2.49496428320802));
#28283=CARTESIAN_POINT('Ctrl Pts',(373.995836024069,-14.6260597566794,2.58971253097699));
#28284=CARTESIAN_POINT('Ctrl Pts',(373.916585384865,-14.6319571440936,2.68083044286543));
#28285=CARTESIAN_POINT('Ctrl Pts',(373.83733474566,-14.6378545315079,2.77194835475387));
#28286=CARTESIAN_POINT('Ctrl Pts',(373.754139007523,-14.6437519189222,2.85943566124755));
#28287=CARTESIAN_POINT('Ctrl Pts',(373.667379174618,-14.6496493063365,2.94295575046901));
#28288=CARTESIAN_POINT('Ctrl Pts',(373.581470342212,-14.6554888480927,3.02565661684024));
#28289=CARTESIAN_POINT('Ctrl Pts',(373.491807866047,-14.6613283898488,3.10471728263915));
#28290=CARTESIAN_POINT('Ctrl Pts',(373.398732178978,-14.667167931605,3.1797805216506));
#28291=CARTESIAN_POINT('Ctrl Pts',(373.305768954703,-14.6730004174779,3.25475306220014));
#28292=CARTESIAN_POINT('Ctrl Pts',(373.209401037049,-14.6788329033507,3.32573753190801));
#28293=CARTESIAN_POINT('Ctrl Pts',(373.110005234208,-14.6846653892236,3.39241388159406));
#28294=CARTESIAN_POINT('Ctrl Pts',(373.010704073303,-14.6904923215645,3.45902674390221));
#28295=CARTESIAN_POINT('Ctrl Pts',(372.90838109884,-14.6963192539055,3.52133942339257));
#28296=CARTESIAN_POINT('Ctrl Pts',(372.803445237623,-14.7021461862465,3.57907283301245));
#28297=CARTESIAN_POINT('Ctrl Pts',(372.698086181016,-14.7079966179982,3.63703907545572));
#28298=CARTESIAN_POINT('Ctrl Pts',(372.590093440982,-14.71384704975,3.69038877569886));
#28299=CARTESIAN_POINT('Ctrl Pts',(372.479909696303,-14.7196974815017,3.73888385564343));
#28300=CARTESIAN_POINT('Ctrl Pts',(372.370281772821,-14.7255184007879,3.78713430246696));
#28301=CARTESIAN_POINT('Ctrl Pts',(372.258485276889,-14.731339320074,3.83057883712004));
#28302=CARTESIAN_POINT('Ctrl Pts',(372.144979320168,-14.7371602393601,3.8690297904084));
#28303=CARTESIAN_POINT('Ctrl Pts',(372.031487632652,-14.7429804268795,3.90747590990168));
#28304=CARTESIAN_POINT('Ctrl Pts',(371.916287295908,-14.7488006143988,3.94092956676532));
#28305=CARTESIAN_POINT('Ctrl Pts',(371.799854699615,-14.7546208019182,3.96925227193495));
#28306=CARTESIAN_POINT('Ctrl Pts',(371.683409733934,-14.7604416077537,3.99757798600882));
#28307=CARTESIAN_POINT('Ctrl Pts',(371.565732642494,-14.7662624135892,4.02077156872991));
#28308=CARTESIAN_POINT('Ctrl Pts',(371.447311586607,-14.7720832194248,4.03874531046862));
#28309=CARTESIAN_POINT('Ctrl Pts',(371.327833198053,-14.7779559968301,4.05687953231941));
#28310=CARTESIAN_POINT('Ctrl Pts',(371.207597908311,-14.7838287742354,4.06970016782488));
#28311=CARTESIAN_POINT('Ctrl Pts',(371.087112851483,-14.7897015516407,4.07717054939513));
#28312=CARTESIAN_POINT('Ctrl Pts',(370.967526141216,-14.7955305411314,4.08458523118182));
#28313=CARTESIAN_POINT('Ctrl Pts',(370.847693785369,-14.801359530622,4.0867292250632));
#28314=CARTESIAN_POINT('Ctrl Pts',(370.728111170366,-14.8071885201127,4.08361912285122));
#28315=CARTESIAN_POINT('Ctrl Pts',(370.607181081669,-14.8130831914753,4.08047397557087));
#28316=CARTESIAN_POINT('Ctrl Pts',(370.486506822828,-14.8189778628379,4.07195562526072));
#28317=CARTESIAN_POINT('Ctrl Pts',(370.366593871449,-14.8248725342006,4.05813495054967));
#28318=CARTESIAN_POINT('Ctrl Pts',(370.246680920071,-14.8307672055632,4.04431427583861));
#28319=CARTESIAN_POINT('Ctrl Pts',(370.127529685368,-14.8366618769258,4.0251913982745));
#28320=CARTESIAN_POINT('Ctrl Pts',(370.009632531657,-14.8425565482884,4.00088979108291));
#28321=CARTESIAN_POINT('Ctrl Pts',(369.892848406526,-14.848395569981,3.97681760743967));
#28322=CARTESIAN_POINT('Ctrl Pts',(369.776943225084,-14.8542345916736,3.9475916297344));
#28323=CARTESIAN_POINT('Ctrl Pts',(369.662404075483,-14.8600736133663,3.91329057157011));
#28324=CARTESIAN_POINT('Ctrl Pts',(369.548003167952,-14.8659055877004,3.87903091278187));
#28325=CARTESIAN_POINT('Ctrl Pts',(369.434965397991,-14.8717375620344,3.83970847421784));
#28326=CARTESIAN_POINT('Ctrl Pts',(369.323767765582,-14.8775695363685,3.79545299440327));
#28327=CARTESIAN_POINT('Ctrl Pts',(369.212675849584,-14.8833959662015,3.75123958860044));
#28328=CARTESIAN_POINT('Ctrl Pts',(369.103420965245,-14.8892223960345,3.70210262234209));
#28329=CARTESIAN_POINT('Ctrl Pts',(368.996464494536,-14.8950488258675,3.64822148888457));
#28330=CARTESIAN_POINT('Ctrl Pts',(368.889063897498,-14.900899449383,3.59411661926696));
#28331=CARTESIAN_POINT('Ctrl Pts',(368.783981240067,-14.9067500728986,3.53522821660625));
#28332=CARTESIAN_POINT('Ctrl Pts',(368.681663325772,-14.9126006964141,3.47178678571165));
#28333=CARTESIAN_POINT('Ctrl Pts',(368.579873241038,-14.9184211381959,3.40867263145132));
#28334=CARTESIAN_POINT('Ctrl Pts',(368.480819784953,-14.9242415799778,3.34105253733104));
#28335=CARTESIAN_POINT('Ctrl Pts',(368.384917322237,-14.9300620217596,3.26919899039507));
#28336=CARTESIAN_POINT('Ctrl Pts',(368.289026748465,-14.9358817419864,3.19735435108038));
#28337=CARTESIAN_POINT('Ctrl Pts',(368.196286715538,-14.9417014622132,3.12127754616099));
#28338=CARTESIAN_POINT('Ctrl Pts',(368.107080796817,-14.9475211824399,3.04128312364354));
#28339=CARTESIAN_POINT('Ctrl Pts',(368.01786523648,-14.9533415316777,2.9612800551141));
#28340=CARTESIAN_POINT('Ctrl Pts',(367.93218485183,-14.9591618809154,2.87735879789877));
#28341=CARTESIAN_POINT('Ctrl Pts',(367.850387991427,-14.9649822301532,2.78987232322122));
#28342=CARTESIAN_POINT('Ctrl Pts',(367.767844686665,-14.9708556934938,2.70158748311521));
#28343=CARTESIAN_POINT('Ctrl Pts',(367.689256437514,-14.9767291568344,2.60967232811506));
#28344=CARTESIAN_POINT('Ctrl Pts',(367.614940401454,-14.982602620175,2.51452457196921));
#28345=CARTESIAN_POINT('Ctrl Pts',(367.541192482523,-14.9884311831777,2.42010418333239));
#28346=CARTESIAN_POINT('Ctrl Pts',(367.471651872845,-14.9942597461804,2.32250081356489));
#28347=CARTESIAN_POINT('Ctrl Pts',(367.406584972693,-15.0000883091831,2.22213237673281));
#28348=CARTESIAN_POINT('Ctrl Pts',(367.340766208196,-15.0059842226927,2.12060415744903));
#28349=CARTESIAN_POINT('Ctrl Pts',(367.279525411764,-15.0118801362022,2.01624693487922));
#28350=CARTESIAN_POINT('Ctrl Pts',(367.223090097801,-15.0177760497117,1.90951802779171));
#28351=CARTESIAN_POINT('Ctrl Pts',(367.166654783838,-15.0236719632213,1.80278912070419));
#28352=CARTESIAN_POINT('Ctrl Pts',(367.115025083587,-15.0295678767308,1.69368893601282));
#28353=CARTESIAN_POINT('Ctrl Pts',(367.068377657378,-15.0354637902403,1.58269372947258));
#28354=CARTESIAN_POINT('Ctrl Pts',(367.016191792706,-15.04205972424,1.45852008692533));
#28355=CARTESIAN_POINT('Ctrl Pts',(366.970102395793,-15.0486556582397,1.33164564697758));
#28356=CARTESIAN_POINT('Ctrl Pts',(366.930366771184,-15.0552515922394,1.20265994738413));
#28357=CARTESIAN_POINT('Ctrl Pts',(366.891893348503,-15.061638006427,1.07777147792508));
#28358=CARTESIAN_POINT('Ctrl Pts',(366.859376354993,-15.0680244206146,0.950904109128813));
#28359=CARTESIAN_POINT('Ctrl Pts',(366.833002004882,-15.0744108348021,0.822615634308196));
#28360=CARTESIAN_POINT('Ctrl Pts',(366.805329755343,-15.0811115287079,0.688013997745671));
#28361=CARTESIAN_POINT('Ctrl Pts',(366.784420209559,-15.0878122226137,0.551848059732137));
#28362=CARTESIAN_POINT('Ctrl Pts',(366.770430667765,-15.0945129165194,0.414784213611038));
#28363=CARTESIAN_POINT('Ctrl Pts',(366.757179050395,-15.1008601602717,0.28495025116066));
#28364=CARTESIAN_POINT('Ctrl Pts',(366.750136314589,-15.107207404024,0.154311017285211));
#28365=CARTESIAN_POINT('Ctrl Pts',(366.749385149013,-15.1135546477762,0.0234478584639096));
#28366=CARTESIAN_POINT('Ctrl Pts',(366.749343319898,-15.1139080979298,0.0161606633633095));
#28367=CARTESIAN_POINT('Ctrl Pts',(366.749320987164,-15.1142615480833,0.0088727770423732));
#28368=CARTESIAN_POINT('Ctrl Pts',(366.749318160447,-15.1146149982368,0.00158430095624623));
#28369=CARTESIAN_POINT('Ctrl Pts',(366.75400096471,-15.1146150285955,0.001581859498241));
#28370=CARTESIAN_POINT('Ctrl Pts',(366.757058589183,-15.1525336964611,-0.779441855919802));
#28371=CARTESIAN_POINT('Ctrl Pts',(367.34239529069,-15.2547547783107,-2.88909145754122));
#28372=CARTESIAN_POINT('Ctrl Pts',(370.310628706842,-15.4022674770118,-4.56577064898819));
#28373=CARTESIAN_POINT('Ctrl Pts',(372.576601567184,-15.5118615078473,-3.80106639475913));
#28374=CARTESIAN_POINT('Ctrl Pts',(373.320108995548,-15.5571531246989,-3.24059684932998));
#28375=CARTESIAN_POINT('',(366.749319083349,-15.0103849713759,-0.00317019281932849));
#28376=CARTESIAN_POINT('Ctrl Pts',(366.74931908335,-15.0103849714045,-0.00317019340519376));
#28377=CARTESIAN_POINT('Ctrl Pts',(366.749445164018,-15.0183047899601,-0.165633270565317));
#28378=CARTESIAN_POINT('Ctrl Pts',(366.759266834899,-15.0262246085157,-0.327714073344508));
#28379=CARTESIAN_POINT('Ctrl Pts',(366.778625923479,-15.0341444270713,-0.488454676509938));
#28380=CARTESIAN_POINT('Ctrl Pts',(366.792402197418,-15.0397803117111,-0.602840566793434));
#28381=CARTESIAN_POINT('Ctrl Pts',(366.811007212665,-15.0454161963508,-0.716548464837123));
#28382=CARTESIAN_POINT('Ctrl Pts',(366.83436962688,-15.0510520809906,-0.829240125997579));
#28383=CARTESIAN_POINT('Ctrl Pts',(366.858576260292,-15.0568916227511,-0.946003988899151));
#28384=CARTESIAN_POINT('Ctrl Pts',(366.88793632571,-15.0627311645116,-1.06188295619786));
#28385=CARTESIAN_POINT('Ctrl Pts',(366.922370559218,-15.0685707062721,-1.17638997314475));
#28386=CARTESIAN_POINT('Ctrl Pts',(366.95676318605,-15.0744031921497,-1.29075863195777));
#28387=CARTESIAN_POINT('Ctrl Pts',(366.996217668377,-15.0802356780273,-1.40375825279818));
#28388=CARTESIAN_POINT('Ctrl Pts',(367.04060372864,-15.0860681639049,-1.51491192514104));
#28389=CARTESIAN_POINT('Ctrl Pts',(367.084947525727,-15.091895096251,-1.62595976003662));
#28390=CARTESIAN_POINT('Ctrl Pts',(367.134213407921,-15.0977220285972,-1.73516476894632));
#28391=CARTESIAN_POINT('Ctrl Pts',(367.188221459996,-15.1035489609433,-1.84206571307579));
#28392=CARTESIAN_POINT('Ctrl Pts',(367.242447320851,-15.1093993926933,-1.94939777744238));
#28393=CARTESIAN_POINT('Ctrl Pts',(367.301453561442,-15.1152498244432,-2.0544067577223));
#28394=CARTESIAN_POINT('Ctrl Pts',(367.365009254367,-15.1211002561932,-2.15664620322714));
#28395=CARTESIAN_POINT('Ctrl Pts',(367.428244341091,-15.1269211754856,-2.25836990264289));
#28396=CARTESIAN_POINT('Ctrl Pts',(367.495982863261,-15.1327420947781,-2.35735160143691));
#28397=CARTESIAN_POINT('Ctrl Pts',(367.567951867668,-15.1385630140705,-2.45317717427856));
#28398=CARTESIAN_POINT('Ctrl Pts',(367.63991182462,-15.1443832015965,-2.54899070058106));
#28399=CARTESIAN_POINT('Ctrl Pts',(367.716100962313,-15.1502033891226,-2.64164856601536));
#28400=CARTESIAN_POINT('Ctrl Pts',(367.796204298034,-15.1560235766486,-2.73076747925784));
#28401=CARTESIAN_POINT('Ctrl Pts',(367.876316143657,-15.1618443824913,-2.81989586018564));
#28402=CARTESIAN_POINT('Ctrl Pts',(367.960342742977,-15.1676651883339,-2.90548423976624));
#28403=CARTESIAN_POINT('Ctrl Pts',(368.047930725338,-15.1734859941766,-2.98718458980248));
#28404=CARTESIAN_POINT('Ctrl Pts',(368.136300744367,-15.1793587715737,-3.06961440828514));
#28405=CARTESIAN_POINT('Ctrl Pts',(368.228295756523,-15.1852315489709,-3.14808613079837));
#28406=CARTESIAN_POINT('Ctrl Pts',(368.323517911581,-15.1911043263681,-3.22228314290432));
#28407=CARTESIAN_POINT('Ctrl Pts',(368.41803008263,-15.1969333158669,-3.29592693614968));
#28408=CARTESIAN_POINT('Ctrl Pts',(368.515721068307,-15.2027623053658,-3.36535936023118));
#28409=CARTESIAN_POINT('Ctrl Pts',(368.616172641397,-15.2085912948646,-3.43031439072977));
#28410=CARTESIAN_POINT('Ctrl Pts',(368.717756116491,-15.2144859662109,-3.49600134335739));
#28411=CARTESIAN_POINT('Ctrl Pts',(368.822162406822,-15.2203806375573,-3.55710916142912));
#28412=CARTESIAN_POINT('Ctrl Pts',(368.928934303735,-15.2262753089036,-3.61341092727321));
#28413=CARTESIAN_POINT('Ctrl Pts',(369.035706200648,-15.2321699802499,-3.66971269311731));
#28414=CARTESIAN_POINT('Ctrl Pts',(369.144843297775,-15.2380646515962,-3.72120827599076));
#28415=CARTESIAN_POINT('Ctrl Pts',(369.255869511939,-15.2439593229425,-3.7677215706436));
#28416=CARTESIAN_POINT('Ctrl Pts',(369.365847566344,-15.2497983447529,-3.81379574950711));
#28417=CARTESIAN_POINT('Ctrl Pts',(369.478010271207,-15.2556373665633,-3.8551200400014));
#28418=CARTESIAN_POINT('Ctrl Pts',(369.59191117128,-15.2614763883737,-3.89148437445927));
#28419=CARTESIAN_POINT('Ctrl Pts',(369.705674599643,-15.267308362827,-3.92780481929679));
#28420=CARTESIAN_POINT('Ctrl Pts',(369.821171666416,-15.2731403372803,-3.95917709449356));
#28421=CARTESIAN_POINT('Ctrl Pts',(369.937935431409,-15.2789723117336,-3.98543894117845));
#28422=CARTESIAN_POINT('Ctrl Pts',(370.054588188257,-15.2847987416871,-4.01167582053797));
#28423=CARTESIAN_POINT('Ctrl Pts',(370.172504853425,-15.2906251716406,-4.03281184992711));
#28424=CARTESIAN_POINT('Ctrl Pts',(370.291203339413,-15.2964516015941,-4.0487345708119));
#28425=CARTESIAN_POINT('Ctrl Pts',(370.41039470593,-15.3023022250649,-4.0647234087919));
#28426=CARTESIAN_POINT('Ctrl Pts',(370.530374005577,-15.3081528485358,-4.07545542336444));
#28427=CARTESIAN_POINT('Ctrl Pts',(370.650642323011,-15.3140034720066,-4.0808685717137));
#28428=CARTESIAN_POINT('Ctrl Pts',(370.770290213208,-15.3198239139116,-4.08625379529655));
#28429=CARTESIAN_POINT('Ctrl Pts',(370.890223736736,-15.3256443558165,-4.08637489068034));
#28430=CARTESIAN_POINT('Ctrl Pts',(371.009947045905,-15.3314647977214,-4.08122278081925));
#28431=CARTESIAN_POINT('Ctrl Pts',(371.129655513096,-15.3372845180721,-4.07607130965999));
#28432=CARTESIAN_POINT('Ctrl Pts',(371.249153412593,-15.3431042384227,-4.06564795114866));
#28433=CARTESIAN_POINT('Ctrl Pts',(371.367946560254,-15.3489239587734,-4.0499957287673));
#28434=CARTESIAN_POINT('Ctrl Pts',(371.486752547411,-15.3547443081358,-4.03434181464989));
#28435=CARTESIAN_POINT('Ctrl Pts',(371.604853229119,-15.3605646574981,-4.01345796596198));
#28436=CARTESIAN_POINT('Ctrl Pts',(371.721761797892,-15.3663850068605,-3.9874388076899));
#28437=CARTESIAN_POINT('Ctrl Pts',(371.839737220009,-15.37225847003,-3.9611822106545));
#28438=CARTESIAN_POINT('Ctrl Pts',(371.956498249157,-15.3781319331995,-3.92969618757733));
#28439=CARTESIAN_POINT('Ctrl Pts',(372.071558557242,-15.3840053963689,-3.89312990283148));
#28440=CARTESIAN_POINT('Ctrl Pts',(372.185739279901,-15.389833959497,-3.85684315124237));
#28441=CARTESIAN_POINT('Ctrl Pts',(372.298244830831,-15.395662522625,-3.81555373822405));
#28442=CARTESIAN_POINT('Ctrl Pts',(372.408619367415,-15.4014910857531,-3.76945616003385));
#28443=CARTESIAN_POINT('Ctrl Pts',(372.520269300994,-15.4073869989433,-3.7228259162983));
#28444=CARTESIAN_POINT('Ctrl Pts',(372.629738273915,-15.4132829121335,-3.67127587025088));
#28445=CARTESIAN_POINT('Ctrl Pts',(372.736580287723,-15.4191788253238,-3.61505499685627));
#28446=CARTESIAN_POINT('Ctrl Pts',(372.84342230153,-15.425074738514,-3.55883412346166));
#28447=CARTESIAN_POINT('Ctrl Pts',(372.947637018142,-15.4309706517042,-3.49794268445248));
#28448=CARTESIAN_POINT('Ctrl Pts',(373.04880971793,-15.4368665648944,-3.43267399867086));
#28449=CARTESIAN_POINT('Ctrl Pts',(373.141827518327,-15.4422872453491,-3.37266621397225));
#28450=CARTESIAN_POINT('Ctrl Pts',(373.232535840599,-15.4477079258038,-3.30879011670646));
#28451=CARTESIAN_POINT('Ctrl Pts',(373.320592904309,-15.4531286062585,-3.2412437998941));
#28452=CARTESIAN_POINT('Ctrl Pts',(373.320592904309,-14.2030090365224,-3.2412437998941));
#28453=CARTESIAN_POINT('Ctrl Pts',(373.415661948684,-14.2088303493544,-3.16831877241942));
#28454=CARTESIAN_POINT('Ctrl Pts',(373.507490248051,-14.2146516621864,-3.09123034712973));
#28455=CARTESIAN_POINT('Ctrl Pts',(373.595707336677,-14.2204729750183,-3.01030781161584));
#28456=CARTESIAN_POINT('Ctrl Pts',(373.68401509969,-14.2263002713166,-2.9293020994593));
#28457=CARTESIAN_POINT('Ctrl Pts',(373.768703942294,-14.2321275676148,-2.84445468371928));
#28458=CARTESIAN_POINT('Ctrl Pts',(373.849439872622,-14.237954863913,-2.75613211006633));
#28459=CARTESIAN_POINT('Ctrl Pts',(373.930223816119,-14.243785625669,-2.66775701151394));
#28460=CARTESIAN_POINT('Ctrl Pts',(374.007049904298,-14.249616387425,-2.57590294867633));
#28461=CARTESIAN_POINT('Ctrl Pts',(374.079625113568,-14.255447149181,-2.48096871926246));
#28462=CARTESIAN_POINT('Ctrl Pts',(374.152301446089,-14.2612860352758,-2.38590221247615));
#28463=CARTESIAN_POINT('Ctrl Pts',(374.220714842523,-14.2671249213706,-2.28774730236853));
#28464=CARTESIAN_POINT('Ctrl Pts',(374.284616060351,-14.2729638074654,-2.18693101900744));
#28465=CARTESIAN_POINT('Ctrl Pts',(374.308179772959,-14.2751169093712,-2.14975479595475));
#28466=CARTESIAN_POINT('Ctrl Pts',(374.33113038291,-14.277270011277,-2.11221691717924));
#28467=CARTESIAN_POINT('Ctrl Pts',(374.353457011468,-14.2794231131828,-2.0743395539091));
#28468=CARTESIAN_POINT('Ctrl Pts',(374.414002743556,-14.2852619316506,-1.97162307422052));
#28469=CARTESIAN_POINT('Ctrl Pts',(374.470138951498,-14.2911007501185,-1.86609867768021));
#28470=CARTESIAN_POINT('Ctrl Pts',(374.521596995379,-14.2969395685863,-1.75818017501912));
#28471=CARTESIAN_POINT('Ctrl Pts',(374.572992873776,-14.3027713332887,-1.6503920466457));
#28472=CARTESIAN_POINT('Ctrl Pts',(374.61972165767,-14.3086030979912,-1.54021592911404));
#28473=CARTESIAN_POINT('Ctrl Pts',(374.66155929608,-14.3144348626936,-1.42809241230507));
#28474=CARTESIAN_POINT('Ctrl Pts',(374.703357114699,-14.3202610768998,-1.31607561124884));
#28475=CARTESIAN_POINT('Ctrl Pts',(374.740272909339,-14.326087291106,-1.20211547697434));
#28476=CARTESIAN_POINT('Ctrl Pts',(374.772129915253,-14.3319135053122,-1.08667435974978));
#28477=CARTESIAN_POINT('Ctrl Pts',(374.804120817757,-14.3377642073881,-0.970748037734786));
#28478=CARTESIAN_POINT('Ctrl Pts',(374.831010134972,-14.3436149094641,-0.853328630028726));
#28479=CARTESIAN_POINT('Ctrl Pts',(374.852668752218,-14.34946561154,-0.734902070040746));
#28480=CARTESIAN_POINT('Ctrl Pts',(374.874214503778,-14.3552858248963,-0.617092645251532));
#28481=CARTESIAN_POINT('Ctrl Pts',(374.890583876499,-14.3611060382526,-0.498286944619419));
#28482=CARTESIAN_POINT('Ctrl Pts',(374.901700669401,-14.3669262516088,-0.378974968389545));
#28483=CARTESIAN_POINT('Ctrl Pts',(374.912816075906,-14.372745739115,-0.259677871786943));
#28484=CARTESIAN_POINT('Ctrl Pts',(374.918680168094,-14.3785652266213,-0.139875029038302));
#28485=CARTESIAN_POINT('Ctrl Pts',(374.91926859001,-14.3843847141275,-0.0200618551361105));
#28486=CARTESIAN_POINT('Ctrl Pts',(374.919857075127,-14.3902048266986,0.0997641877711278));
#28487=CARTESIAN_POINT('Ctrl Pts',(374.91516876131,-14.3960249392698,0.219600158360798));
#28488=CARTESIAN_POINT('Ctrl Pts',(374.905231417739,-14.4018450518409,0.338950955513449));
#28489=CARTESIAN_POINT('Ctrl Pts',(374.895202449701,-14.4077188271154,0.459402192965573));
#28490=CARTESIAN_POINT('Ctrl Pts',(374.879827188809,-14.4135926023899,0.579358844228589));
#28491=CARTESIAN_POINT('Ctrl Pts',(374.859187531011,-14.4194663776644,0.698318750165522));
#28492=CARTESIAN_POINT('Ctrl Pts',(374.838707599901,-14.425294696823,0.816358046270801));
#28493=CARTESIAN_POINT('Ctrl Pts',(374.813044612295,-14.4311230159817,0.933415583774485));
#28494=CARTESIAN_POINT('Ctrl Pts',(374.782329488656,-14.4369513351403,1.04901340625064));
#28495=CARTESIAN_POINT('Ctrl Pts',(374.751255035805,-14.4428478384727,1.16596358123228));
#28496=CARTESIAN_POINT('Ctrl Pts',(374.715009612851,-14.4487443418051,1.28141926077883));
#28497=CARTESIAN_POINT('Ctrl Pts',(374.67377953316,-14.4546408451375,1.39490465921606));
#28498=CARTESIAN_POINT('Ctrl Pts',(374.632549453469,-14.4605373484699,1.50839005765328));
#28499=CARTESIAN_POINT('Ctrl Pts',(374.586334930723,-14.4664338518024,1.61990480424541));
#28500=CARTESIAN_POINT('Ctrl Pts',(374.535370478715,-14.4723303551348,1.72899810970076));
#28501=CARTESIAN_POINT('Ctrl Pts',(374.484903841064,-14.4781692621642,1.83702580546745));
#28502=CARTESIAN_POINT('Ctrl Pts',(374.429627465073,-14.4840081691935,1.943005024189));
#28503=CARTESIAN_POINT('Ctrl Pts',(374.369730689474,-14.4898470762229,2.04648016782015));
#28504=CARTESIAN_POINT('Ctrl Pts',(374.309906274741,-14.4956789293105,2.14983030387002));
#28505=CARTESIAN_POINT('Ctrl Pts',(374.245472766137,-14.501510782398,2.2506820344613));
#28506=CARTESIAN_POINT('Ctrl Pts',(374.176666805362,-14.5073426354855,2.34860138851618));
#28507=CARTESIAN_POINT('Ctrl Pts',(374.107926334413,-14.5131689377889,2.44642754248648));
#28508=CARTESIAN_POINT('Ctrl Pts',(374.034821923996,-14.5189952400923,2.54132654307397));
#28509=CARTESIAN_POINT('Ctrl Pts',(373.95763490541,-14.5248215423956,2.63289110893821));
#28510=CARTESIAN_POINT('Ctrl Pts',(373.880125076856,-14.5306722113411,2.72483861425343));
#28511=CARTESIAN_POINT('Ctrl Pts',(373.798498624598,-14.5365228802866,2.81342337494466));
#28512=CARTESIAN_POINT('Ctrl Pts',(373.713083257921,-14.542373549232,2.89826409161019));
#28513=CARTESIAN_POINT('Ctrl Pts',(373.628111252513,-14.548193849403,2.98266442981435));
#28514=CARTESIAN_POINT('Ctrl Pts',(373.539389870294,-14.554014149574,3.06335921760744));
#28515=CARTESIAN_POINT('Ctrl Pts',(373.447280121202,-14.5598344497451,3.14000846911619));
#28516=CARTESIAN_POINT('Ctrl Pts',(373.355181869303,-14.5656540234228,3.21664815322072));
#28517=CARTESIAN_POINT('Ctrl Pts',(373.259696403656,-14.5714735971006,3.28924304615679));
#28518=CARTESIAN_POINT('Ctrl Pts',(373.161218522421,-14.5772931707783,3.35749285564257));
#28519=CARTESIAN_POINT('Ctrl Pts',(373.062730076529,-14.583113368777,3.42574998693326));
#28520=CARTESIAN_POINT('Ctrl Pts',(372.961248910181,-14.5889335667757,3.48966087688044));
#28521=CARTESIAN_POINT('Ctrl Pts',(372.857199044004,-14.5947537647743,3.54896839771591));
#28522=CARTESIAN_POINT('Ctrl Pts',(372.752193548181,-14.600627417467,3.60882061915788));
#28523=CARTESIAN_POINT('Ctrl Pts',(372.644572289829,-14.6065010701597,3.6639842669187));
#28524=CARTESIAN_POINT('Ctrl Pts',(372.534795674837,-14.6123747228524,3.71424288088465));
#28525=CARTESIAN_POINT('Ctrl Pts',(372.425864780562,-14.6182031248351,3.76411430172139));
#28526=CARTESIAN_POINT('Ctrl Pts',(372.314812024559,-14.6240315268178,3.80915590334672));
#28527=CARTESIAN_POINT('Ctrl Pts',(372.20210562926,-14.6298599288005,3.84920532054668));
#28528=CARTESIAN_POINT('Ctrl Pts',(372.088086684375,-14.6357562068482,3.88972114292145));
#28529=CARTESIAN_POINT('Ctrl Pts',(371.972375749005,-14.6416524848959,3.92512764102816));
#28530=CARTESIAN_POINT('Ctrl Pts',(371.855470507816,-14.6475487629436,3.95530937551278));
#28531=CARTESIAN_POINT('Ctrl Pts',(371.738565266627,-14.6534450409913,3.98549110999739));
#28532=CARTESIAN_POINT('Ctrl Pts',(371.620466146087,-14.659341319039,4.01044804739018));
#28533=CARTESIAN_POINT('Ctrl Pts',(371.501677478411,-14.6652375970867,4.03011862488805));
#28534=CARTESIAN_POINT('Ctrl Pts',(371.384044436807,-14.6710765136641,4.04959783874287));
#28535=CARTESIAN_POINT('Ctrl Pts',(371.265380472658,-14.6769154302414,4.06395187513785));
#28536=CARTESIAN_POINT('Ctrl Pts',(371.146168404866,-14.6827543468188,4.07307920785252));
#28537=CARTESIAN_POINT('Ctrl Pts',(371.027100336288,-14.688586210424,4.08219551543557));
#28538=CARTESIAN_POINT('Ctrl Pts',(370.907485882455,-14.6944180740292,4.08609764807583));
#28539=CARTESIAN_POINT('Ctrl Pts',(370.787816779592,-14.7002499376343,4.08473532192122));
#28540=CARTESIAN_POINT('Ctrl Pts',(370.66826155876,-14.7060762513987,4.0833742922121));
#28541=CARTESIAN_POINT('Ctrl Pts',(370.548652195972,-14.7119025651631,4.07675877654074));
#28542=CARTESIAN_POINT('Ctrl Pts',(370.429483691496,-14.7177288789274,4.06489044151223));
#28543=CARTESIAN_POINT('Ctrl Pts',(370.309817118944,-14.7235795439321,4.05297250244768));
#28544=CARTESIAN_POINT('Ctrl Pts',(370.190595510944,-14.7294302089367,4.03575770788277));
#28545=CARTESIAN_POINT('Ctrl Pts',(370.072318666318,-14.7352808739413,4.0133006664283));
#28546=CARTESIAN_POINT('Ctrl Pts',(369.95465539979,-14.7411011877819,3.99096012409794));
#28547=CARTESIAN_POINT('Ctrl Pts',(369.837927518439,-14.7469215016226,3.96343168110069));
#28548=CARTESIAN_POINT('Ctrl Pts',(369.72261958799,-14.7527418154632,3.93082077524223));
#28549=CARTESIAN_POINT('Ctrl Pts',(369.607326034435,-14.7585614036119,3.89821393539673));
#28550=CARTESIAN_POINT('Ctrl Pts',(369.493452469857,-14.7643809917605,3.86052600369593));
#28551=CARTESIAN_POINT('Ctrl Pts',(369.381469834352,-14.7702005799092,3.81791273264077));
#28552=CARTESIAN_POINT('Ctrl Pts',(369.269475170411,-14.7760207931597,3.7752948843487));
#28553=CARTESIAN_POINT('Ctrl Pts',(369.159372218528,-14.7818410064102,3.72775078908034));
#28554=CARTESIAN_POINT('Ctrl Pts',(369.051612848481,-14.7876612196608,3.67548471171662));
#28555=CARTESIAN_POINT('Ctrl Pts',(368.942864392941,-14.7935348546089,3.62273890234619));
#28556=CARTESIAN_POINT('Ctrl Pts',(368.836503142544,-14.7994084895571,3.56518416254497));
#28557=CARTESIAN_POINT('Ctrl Pts',(368.732967999565,-14.8052821245052,3.50307775998863));
#28558=CARTESIAN_POINT('Ctrl Pts',(368.63022988261,-14.8111105435028,3.44144946001386));
#28559=CARTESIAN_POINT('Ctrl Pts',(368.530274821467,-14.8169389625003,3.37533960636082));
#28560=CARTESIAN_POINT('Ctrl Pts',(368.433501534976,-14.8227673814978,3.30504251198595));
#28561=CARTESIAN_POINT('Ctrl Pts',(368.335602120762,-14.8286636244213,3.23392738703963));
#28562=CARTESIAN_POINT('Ctrl Pts',(368.240959337544,-14.8345598673448,3.15852721721278));
#28563=CARTESIAN_POINT('Ctrl Pts',(368.149949857687,-14.8404561102682,3.07918714347423));
#28564=CARTESIAN_POINT('Ctrl Pts',(368.05894037783,-14.8463523531917,2.99984706973568));
#28565=CARTESIAN_POINT('Ctrl Pts',(367.971564470121,-14.8522485961152,2.91656742484888));
#28566=CARTESIAN_POINT('Ctrl Pts',(367.888158136163,-14.8581448390387,2.82972930181761));
#28567=CARTESIAN_POINT('Ctrl Pts',(367.806660262009,-14.863906167237,2.74487816298118));
#28568=CARTESIAN_POINT('Ctrl Pts',(367.728691228059,-14.8696674954354,2.6563575941899));
#28569=CARTESIAN_POINT('Ctrl Pts',(367.654603693653,-14.8754288236337,2.56449661014033));
#28570=CARTESIAN_POINT('Ctrl Pts',(367.580625533572,-14.8811816464689,2.4727712390961));
#28571=CARTESIAN_POINT('Ctrl Pts',(367.510517729518,-14.8869344693041,2.37771558942559));
#28572=CARTESIAN_POINT('Ctrl Pts',(367.44459590751,-14.8926872921393,2.27969518373436));
#28573=CARTESIAN_POINT('Ctrl Pts',(367.37872953369,-14.8984352761579,2.18175722500505));
#28574=CARTESIAN_POINT('Ctrl Pts',(367.317042376498,-14.9041832601765,2.08085981096543));
#28575=CARTESIAN_POINT('Ctrl Pts',(367.259809457048,-14.909931244195,1.9774010027479));
#28576=CARTESIAN_POINT('Ctrl Pts',(367.202610438528,-14.9156758234947,1.87400347656646));
#28577=CARTESIAN_POINT('Ctrl Pts',(367.149860614512,-14.9214204027943,1.76804793698009));
#28578=CARTESIAN_POINT('Ctrl Pts',(367.101790944581,-14.927164982094,1.65996020321443));
#28579=CARTESIAN_POINT('Ctrl Pts',(367.053737790816,-14.9329075876247,1.55190960710544));
#28580=CARTESIAN_POINT('Ctrl Pts',(367.010361762391,-14.9386501931554,1.4417286554423));
#28581=CARTESIAN_POINT('Ctrl Pts',(366.971846879343,-14.944392798686,1.32986577364936));
#28582=CARTESIAN_POINT('Ctrl Pts',(366.933322274463,-14.9501368537509,1.21797465570625));
#28583=CARTESIAN_POINT('Ctrl Pts',(366.899661410976,-14.9558809088158,1.10440115207591));
#28584=CARTESIAN_POINT('Ctrl Pts',(366.870999241777,-14.9616249638807,0.989611329846685));
#28585=CARTESIAN_POINT('Ctrl Pts',(366.842334210192,-14.9673695925835,0.87481004397493));
#28586=CARTESIAN_POINT('Ctrl Pts',(366.818668959252,-14.9731142212863,0.758792605684265));
#28587=CARTESIAN_POINT('Ctrl Pts',(366.800087550079,-14.9788588499891,0.642036495215628));
#28588=CARTESIAN_POINT('Ctrl Pts',(366.781489033254,-14.9846087676939,0.525172888972658));
#28589=CARTESIAN_POINT('Ctrl Pts',(366.767983764793,-14.9903586853988,0.407569666818465));
#28590=CARTESIAN_POINT('Ctrl Pts',(366.759604034958,-14.9961086031037,0.289710716467365));
#28591=CARTESIAN_POINT('Ctrl Pts',(366.752668740967,-15.0008673925278,0.192167420153659));
#28592=CARTESIAN_POINT('Ctrl Pts',(366.749243325144,-15.0056261819518,0.0944491614589898));
#28593=CARTESIAN_POINT('Ctrl Pts',(366.749319083349,-15.0103849713759,-0.00317019281933907));
#28594=CARTESIAN_POINT('Origin',(370.834317853224,-8.23961502859548,0.));
#28595=CARTESIAN_POINT('',(373.320592904309,-12.9531485432512,-3.24124379989409));
#28596=CARTESIAN_POINT('',(373.320592904309,-13.0571931311057,-3.2412437998941));
#28597=CARTESIAN_POINT('',(373.320592904309,-8.23961502859548,-3.24124379989413));
#28598=CARTESIAN_POINT('',(366.749318109676,-13.864615028561,-0.00144748442786206));
#28599=CARTESIAN_POINT('Ctrl Pts',(373.320592904309,-13.0571931311057,-3.2412437998941));
#28600=CARTESIAN_POINT('Ctrl Pts',(373.415634712958,-13.0630222050237,-3.16833966424664));
#28601=CARTESIAN_POINT('Ctrl Pts',(373.507397375535,-13.0688512789417,-3.09130541218824));
#28602=CARTESIAN_POINT('Ctrl Pts',(373.595519638687,-13.0746803528596,-3.01047997833458));
#28603=CARTESIAN_POINT('Ctrl Pts',(373.683775086311,-13.0805182366072,-2.92953238814687));
#28604=CARTESIAN_POINT('Ctrl Pts',(373.76837885436,-13.0863561203548,-2.84478245481835));
#28605=CARTESIAN_POINT('Ctrl Pts',(373.849007325584,-13.0921940041024,-2.75660522839973));
#28606=CARTESIAN_POINT('Ctrl Pts',(373.9143684516,-13.0969264596419,-2.68512473620953));
#28607=CARTESIAN_POINT('Ctrl Pts',(373.977117920218,-13.1016589151815,-2.61139273980695));
#28608=CARTESIAN_POINT('Ctrl Pts',(374.03710392341,-13.106391370721,-2.53562347138149));
#28609=CARTESIAN_POINT('Ctrl Pts',(374.111114034853,-13.1122302255079,-2.44214013023974));
#28610=CARTESIAN_POINT('Ctrl Pts',(374.181139475934,-13.1180690802947,-2.34527280419094));
#28611=CARTESIAN_POINT('Ctrl Pts',(374.246857595481,-13.1239079350815,-2.24539473311907));
#28612=CARTESIAN_POINT('Ctrl Pts',(374.312496322541,-13.1297397360878,-2.14563732235193));
#28613=CARTESIAN_POINT('Ctrl Pts',(374.373837858353,-13.1355715370941,-2.04287673835842));
#28614=CARTESIAN_POINT('Ctrl Pts',(374.43060006475,-13.1414033381003,-1.9375188399243));
#28615=CARTESIAN_POINT('Ctrl Pts',(374.487308246335,-13.1472295885481,-1.83226121843365));
#28616=CARTESIAN_POINT('Ctrl Pts',(374.539445579219,-13.1530558389958,-1.72441155653902));
#28617=CARTESIAN_POINT('Ctrl Pts',(374.586773795764,-13.1588820894436,-1.61440372871605));
#28618=CARTESIAN_POINT('Ctrl Pts',(374.634300528992,-13.1647327779115,-1.50393447659702));
#28619=CARTESIAN_POINT('Ctrl Pts',(374.676977486266,-13.1705834663794,-1.39128926017079));
#28620=CARTESIAN_POINT('Ctrl Pts',(374.714610386602,-13.1764341548473,-1.27693181313962));
#28621=CARTESIAN_POINT('Ctrl Pts',(374.752047494974,-13.1822544040512,-1.16316933139164));
#28622=CARTESIAN_POINT('Ctrl Pts',(374.784492787487,-13.188074653255,-1.04771278505638));
#28623=CARTESIAN_POINT('Ctrl Pts',(374.811803840143,-13.1938949024589,-0.931037176413037));
#28624=CARTESIAN_POINT('Ctrl Pts',(374.839111485795,-13.1997144255973,-0.814376122839463));
#28625=CARTESIAN_POINT('Ctrl Pts',(374.861286073291,-13.2055339487357,-0.696496704403742));
#28626=CARTESIAN_POINT('Ctrl Pts',(374.878235797962,-13.2113534718741,-0.57788636965012));
#28627=CARTESIAN_POINT('Ctrl Pts',(374.895187342422,-13.2171736198197,-0.459263300418008));
#28628=CARTESIAN_POINT('Ctrl Pts',(374.906912851315,-13.2229937677653,-0.33990956043577));
#28629=CARTESIAN_POINT('Ctrl Pts',(374.91337219933,-13.2288139157109,-0.220319407936235));
#28630=CARTESIAN_POINT('Ctrl Pts',(374.91989100824,-13.2346876404578,-0.0996283800139154));
#28631=CARTESIAN_POINT('Ctrl Pts',(374.921046175616,-13.2405613652046,0.0213030153844473));
#28632=CARTESIAN_POINT('Ctrl Pts',(374.916850230376,-13.2464350899514,0.141966156199758));
#28633=CARTESIAN_POINT('Ctrl Pts',(374.912686696418,-13.2522634435269,0.261697243117249));
#28634=CARTESIAN_POINT('Ctrl Pts',(374.903254520544,-13.2580917971023,0.381163802454329));
#28635=CARTESIAN_POINT('Ctrl Pts',(374.888618103044,-13.2639201506777,0.499874468553034));
#28636=CARTESIAN_POINT('Ctrl Pts',(374.873810778426,-13.2698165610103,0.619971300206968));
#28637=CARTESIAN_POINT('Ctrl Pts',(374.853676970586,-13.2757129713428,0.73929405099517));
#28638=CARTESIAN_POINT('Ctrl Pts',(374.828336241694,-13.2816093816754,0.857345970167816));
#28639=CARTESIAN_POINT('Ctrl Pts',(374.802995512802,-13.2875057920079,0.975397889340462));
#28640=CARTESIAN_POINT('Ctrl Pts',(374.772448023863,-13.2934022023404,1.09217858049311));
#28641=CARTESIAN_POINT('Ctrl Pts',(374.73686449609,-13.299298612673,1.20720946825777));
#28642=CARTESIAN_POINT('Ctrl Pts',(374.701628305141,-13.3051374671486,1.3211175201024));
#28643=CARTESIAN_POINT('Ctrl Pts',(374.661347710689,-13.3109763216242,1.4336533651992));
#28644=CARTESIAN_POINT('Ctrl Pts',(374.61614803537,-13.3168151760998,1.54433981798324));
#28645=CARTESIAN_POINT('Ctrl Pts',(374.571002964228,-13.3226469768556,1.6548925542618));
#28646=CARTESIAN_POINT('Ctrl Pts',(374.520950786023,-13.3284787776115,1.7635999700876));
#28647=CARTESIAN_POINT('Ctrl Pts',(374.466166637357,-13.3343105783674,1.86999984203066));
#28648=CARTESIAN_POINT('Ctrl Pts',(374.411434630269,-13.3401368286253,1.97629844640786));
#28649=CARTESIAN_POINT('Ctrl Pts',(374.351979798616,-13.3459630788833,2.08029351793484));
#28650=CARTESIAN_POINT('Ctrl Pts',(374.288025195678,-13.3517893291412,2.1815431677319));
#28651=CARTESIAN_POINT('Ctrl Pts',(374.223802334092,-13.357640017703,2.28321751087358));
#28652=CARTESIAN_POINT('Ctrl Pts',(374.155042026257,-13.3634907062649,2.38212296678474));
#28653=CARTESIAN_POINT('Ctrl Pts',(374.082016828196,-13.3693413948267,2.47783703418227));
#28654=CARTESIAN_POINT('Ctrl Pts',(374.009371558597,-13.3751616439899,2.57305312965482));
#28655=CARTESIAN_POINT('Ctrl Pts',(373.932505926946,-13.3809818931532,2.66511064520723));
#28656=CARTESIAN_POINT('Ctrl Pts',(373.851731111693,-13.3868021423164,2.75362347237566));
#28657=CARTESIAN_POINT('Ctrl Pts',(373.770966372169,-13.3926216654705,2.84212525858524));
#28658=CARTESIAN_POINT('Ctrl Pts',(373.686293692495,-13.3984411886245,2.92708293641963));
#28659=CARTESIAN_POINT('Ctrl Pts',(373.598063144806,-13.4042607117785,3.00814510342507));
#28660=CARTESIAN_POINT('Ctrl Pts',(373.509823123481,-13.4100808597958,3.08921597437034));
#28661=CARTESIAN_POINT('Ctrl Pts',(373.418024773309,-13.4159010078132,3.16639022837159));
#28662=CARTESIAN_POINT('Ctrl Pts',(373.323053011204,-13.4217211558306,3.23935523112764));
#28663=CARTESIAN_POINT('Ctrl Pts',(373.227206994545,-13.4275948807301,3.31299190706824));
#28664=CARTESIAN_POINT('Ctrl Pts',(373.128129170963,-13.4334686056296,3.38234117696181));
#28665=CARTESIAN_POINT('Ctrl Pts',(373.02624608336,-13.4393423305292,3.44712570614027));
#28666=CARTESIAN_POINT('Ctrl Pts',(372.925149983459,-13.4451706843139,3.51140981244237));
#28667=CARTESIAN_POINT('Ctrl Pts',(372.821292189772,-13.4509990380987,3.57119929880891));
#28668=CARTESIAN_POINT('Ctrl Pts',(372.715114351455,-13.4568273918834,3.62626936840638));
#28669=CARTESIAN_POINT('Ctrl Pts',(372.60769669301,-13.4627238023403,3.68198248161638));
#28670=CARTESIAN_POINT('Ctrl Pts',(372.497904851588,-13.4686202127972,3.73286507992408));
#28671=CARTESIAN_POINT('Ctrl Pts',(372.386216115876,-13.4745166232542,3.77873481239129));
#28672=CARTESIAN_POINT('Ctrl Pts',(372.274527380164,-13.4804130337111,3.82460454485849));
#28673=CARTESIAN_POINT('Ctrl Pts',(372.160942168137,-13.486309444168,3.86546132006785));
#28674=CARTESIAN_POINT('Ctrl Pts',(372.045951713958,-13.4922058546249,3.90117525721697));
#28675=CARTESIAN_POINT('Ctrl Pts',(371.932083590863,-13.4980447148722,3.93654061880763));
#28676=CARTESIAN_POINT('Ctrl Pts',(371.816494090411,-13.5038835751196,3.96696979634805));
#28677=CARTESIAN_POINT('Ctrl Pts',(371.699647624774,-13.5097224353669,3.99229625484738));
#28678=CARTESIAN_POINT('Ctrl Pts',(371.582942317908,-13.5155542418593,4.01759211719896));
#28679=CARTESIAN_POINT('Ctrl Pts',(371.46498346001,-13.5213860483518,4.03779743825467));
#28680=CARTESIAN_POINT('Ctrl Pts',(371.346251297956,-13.5272178548442,4.05279522652758));
#28681=CARTESIAN_POINT('Ctrl Pts',(371.227632141643,-13.5330441107966,4.06777874035151));
#28682=CARTESIAN_POINT('Ctrl Pts',(371.108241546071,-13.538870366749,4.07756453259185));
#28683=CARTESIAN_POINT('Ctrl Pts',(370.988570089168,-13.5446966227014,4.08208662912804));
#28684=CARTESIAN_POINT('Ctrl Pts',(370.868396829967,-13.5505473091129,4.08662768756622));
#28685=CARTESIAN_POINT('Ctrl Pts',(370.747940753732,-13.5563979955243,4.08586072260642));
#28686=CARTESIAN_POINT('Ctrl Pts',(370.627704445442,-13.5622486819358,4.07977154994303));
#28687=CARTESIAN_POINT('Ctrl Pts',(370.508093532916,-13.5680689366537,4.07371404943293));
#28688=CARTESIAN_POINT('Ctrl Pts',(370.388700516253,-13.5738891913715,4.06238960520887));
#28689=CARTESIAN_POINT('Ctrl Pts',(370.270019813719,-13.5797094460894,4.04583646760595));
#28690=CARTESIAN_POINT('Ctrl Pts',(370.151353916506,-13.5855289747351,4.02928539499355));
#28691=CARTESIAN_POINT('Ctrl Pts',(370.033400558351,-13.5913485033809,4.00750698262282));
#28692=CARTESIAN_POINT('Ctrl Pts',(369.916647533344,-13.5971680320267,3.98059118524009));
#28693=CARTESIAN_POINT('Ctrl Pts',(369.799881973539,-13.6029881854667,3.95367249813293));
#28694=CARTESIAN_POINT('Ctrl Pts',(369.684317398419,-13.6088083389067,3.92161542049096));
#28695=CARTESIAN_POINT('Ctrl Pts',(369.570429337899,-13.6146284923467,3.88456056984963));
#28696=CARTESIAN_POINT('Ctrl Pts',(369.455493151723,-13.6205022093658,3.84716469891608));
#28697=CARTESIAN_POINT('Ctrl Pts',(369.342264898922,-13.626375926385,3.80467871715061));
#28698=CARTESIAN_POINT('Ctrl Pts',(369.231214537902,-13.6322496434042,3.75729753418646));
#28699=CARTESIAN_POINT('Ctrl Pts',(369.121021730229,-13.6380780023927,3.71028223829959));
#28700=CARTESIAN_POINT('Ctrl Pts',(369.012973638525,-13.6439063613811,3.65844731053448));
#28701=CARTESIAN_POINT('Ctrl Pts',(368.907505440725,-13.6497347203696,3.60202983427953));
#28702=CARTESIAN_POINT('Ctrl Pts',(368.800806065393,-13.6556311164041,3.54495377154423));
#28703=CARTESIAN_POINT('Ctrl Pts',(368.696747568476,-13.6615275124386,3.48318770888157));
#28704=CARTESIAN_POINT('Ctrl Pts',(368.595750276169,-13.6674239084732,3.4170221250319));
#28705=CARTESIAN_POINT('Ctrl Pts',(368.494752983861,-13.6733203045077,3.35085654118224));
#28706=CARTESIAN_POINT('Ctrl Pts',(368.396817207948,-13.6792167005423,3.28029172913517));
#28707=CARTESIAN_POINT('Ctrl Pts',(368.302327890809,-13.6851130965768,3.20565934407081));
#28708=CARTESIAN_POINT('Ctrl Pts',(368.209633776792,-13.6908974669465,3.13244490015359));
#28709=CARTESIAN_POINT('Ctrl Pts',(368.119964495517,-13.6966818373162,3.05508541895734));
#28710=CARTESIAN_POINT('Ctrl Pts',(368.03371601442,-13.7024662076859,2.97386185632225));
#28711=CARTESIAN_POINT('Ctrl Pts',(367.947572413299,-13.7082435441389,2.89273706325591));
#28712=CARTESIAN_POINT('Ctrl Pts',(367.864841639667,-13.714020880592,2.80775781424708));
#28713=CARTESIAN_POINT('Ctrl Pts',(367.785888110422,-13.719798217045,2.71924642193395));
#28714=CARTESIAN_POINT('Ctrl Pts',(367.703426535092,-13.7258322508582,2.62680231063686));
#28715=CARTESIAN_POINT('Ctrl Pts',(367.625085979366,-13.7318662846714,2.53050519941724));
#28716=CARTESIAN_POINT('Ctrl Pts',(367.551240700248,-13.7379003184845,2.43076724669488));
#28717=CARTESIAN_POINT('Ctrl Pts',(367.480651420613,-13.7436682985808,2.33542695793263));
#28718=CARTESIAN_POINT('Ctrl Pts',(367.414169730435,-13.7494362786771,2.2369431626848));
#28719=CARTESIAN_POINT('Ctrl Pts',(367.352082186995,-13.7552042587734,2.13571059950636));
#28720=CARTESIAN_POINT('Ctrl Pts',(367.290014383364,-13.7609704050264,2.03451022171223));
#28721=CARTESIAN_POINT('Ctrl Pts',(367.232338165302,-13.7667365512794,1.9305631664438));
#28722=CARTESIAN_POINT('Ctrl Pts',(367.179296528996,-13.7725026975325,1.82429277240197));
#28723=CARTESIAN_POINT('Ctrl Pts',(367.126258799186,-13.7782684191111,1.71803020513293));
#28724=CARTESIAN_POINT('Ctrl Pts',(367.077855156735,-13.7840341406897,1.60944501046251));
#28725=CARTESIAN_POINT('Ctrl Pts',(367.034282094525,-13.7897998622683,1.49898406682881));
#28726=CARTESIAN_POINT('Ctrl Pts',(366.990701597061,-13.7955665677025,1.38850427427539));
#28727=CARTESIAN_POINT('Ctrl Pts',(366.951953469599,-13.8013332731368,1.27614848225212));
#28728=CARTESIAN_POINT('Ctrl Pts',(366.918185362683,-13.8070999785711,1.1623817430307));
#28729=CARTESIAN_POINT('Ctrl Pts',(366.884386361119,-13.8128719599997,1.04851091791767));
#28730=CARTESIAN_POINT('Ctrl Pts',(366.855576592803,-13.8186439414283,0.933226966533934));
#28731=CARTESIAN_POINT('Ctrl Pts',(366.831853294486,-13.824415922857,0.817008234991934));
#28732=CARTESIAN_POINT('Ctrl Pts',(366.808117223194,-13.8301910120057,0.700726929567399));
#28733=CARTESIAN_POINT('Ctrl Pts',(366.789473140479,-13.8359661011544,0.583510250425359));
#28734=CARTESIAN_POINT('Ctrl Pts',(366.775966572866,-13.8417411903032,0.465843198103686));
#28735=CARTESIAN_POINT('Ctrl Pts',(366.762442319589,-13.8475238414239,0.348022071111352));
#28736=CARTESIAN_POINT('Ctrl Pts',(366.7540690373,-13.8533064925447,0.229749806177949));
#28737=CARTESIAN_POINT('Ctrl Pts',(366.750840186333,-13.8590891436655,0.11151297683367));
#28738=CARTESIAN_POINT('Ctrl Pts',(366.749811692746,-13.8609311052973,0.0738507180229249));
#28739=CARTESIAN_POINT('Ctrl Pts',(366.74930477244,-13.8627730669292,0.0361920264922796));
#28740=CARTESIAN_POINT('Ctrl Pts',(366.749318109676,-13.864615028561,-0.00144748442786197));
#28741=CARTESIAN_POINT('Ctrl Pts',(366.749318109676,-13.8646150285955,-0.00144748513296822));
#28742=CARTESIAN_POINT('Ctrl Pts',(366.749350464652,-13.8690834652399,-0.0927576226328301));
#28743=CARTESIAN_POINT('Ctrl Pts',(366.752444184748,-13.8735519018843,-0.184007250062436));
#28744=CARTESIAN_POINT('Ctrl Pts',(366.75858808408,-13.8780203385288,-0.275048811866955));
#28745=CARTESIAN_POINT('Ctrl Pts',(366.766616196763,-13.8838591569996,-0.394011034000072));
#28746=CARTESIAN_POINT('Ctrl Pts',(366.779869115059,-13.8896979754705,-0.51280090005843));
#28747=CARTESIAN_POINT('Ctrl Pts',(366.798334899559,-13.8955367939414,-0.630925191859141));
#28748=CARTESIAN_POINT('Ctrl Pts',(366.816778375896,-13.9013685586469,-0.748906779952974));
#28749=CARTESIAN_POINT('Ctrl Pts',(366.840422128447,-13.9072003233524,-0.866223995644971));
#28750=CARTESIAN_POINT('Ctrl Pts',(366.869202296336,-13.9130320880579,-0.982386696024231));
#28751=CARTESIAN_POINT('Ctrl Pts',(366.897955072137,-13.9188583022672,-1.09843883627878));
#28752=CARTESIAN_POINT('Ctrl Pts',(366.931834439113,-13.9246845164764,-1.21333825579321));
#28753=CARTESIAN_POINT('Ctrl Pts',(366.97072522258,-13.9305107306857,-1.32660355209665));
#28754=CARTESIAN_POINT('Ctrl Pts',(367.009779465928,-13.9363614327605,-1.44034490802412));
#28755=CARTESIAN_POINT('Ctrl Pts',(367.053887280941,-13.9422121348353,-1.55243796460567));
#28756=CARTESIAN_POINT('Ctrl Pts',(367.102880849631,-13.9480628369101,-1.66240876087073));
#28757=CARTESIAN_POINT('Ctrl Pts',(367.151619106916,-13.9538830502694,-1.77180648602832));
#28758=CARTESIAN_POINT('Ctrl Pts',(367.205192143526,-13.9597032636287,-1.879103646418));
#28759=CARTESIAN_POINT('Ctrl Pts',(367.263386173736,-13.965523476988,-1.9838528021074));
#28760=CARTESIAN_POINT('Ctrl Pts',(367.321572946456,-13.9713429644973,-2.0885888943268));
#28761=CARTESIAN_POINT('Ctrl Pts',(367.38437936936,-13.9771624520065,-2.19077725943343));
#28762=CARTESIAN_POINT('Ctrl Pts',(367.451545809899,-13.9829819395158,-2.28999526263686));
#28763=CARTESIAN_POINT('Ctrl Pts',(367.518719464713,-13.9888020520899,-2.38922392273988));
#28764=CARTESIAN_POINT('Ctrl Pts',(367.590253840866,-13.9946221646641,-2.4854812506462));
#28765=CARTESIAN_POINT('Ctrl Pts',(367.665846462443,-14.0004422772383,-2.57837430288916));
#28766=CARTESIAN_POINT('Ctrl Pts',(367.742136064331,-14.0063160525085,-2.67212384915385));
#28767=CARTESIAN_POINT('Ctrl Pts',(367.822558871191,-14.0121898277787,-2.76244643184495));
#28768=CARTESIAN_POINT('Ctrl Pts',(367.906763749228,-14.0180636030489,-2.84897384476831));
#28769=CARTESIAN_POINT('Ctrl Pts',(367.990316980597,-14.0238919222105,-2.93483163733683));
#28770=CARTESIAN_POINT('Ctrl Pts',(368.077593612437,-14.029720241372,-3.01695255774001));
#28771=CARTESIAN_POINT('Ctrl Pts',(368.168215715381,-14.0355485605336,-3.09501605659609));
#28772=CARTESIAN_POINT('Ctrl Pts',(368.259897985426,-14.0414450638581,-3.1739928023382));
#28773=CARTESIAN_POINT('Ctrl Pts',(368.355004165594,-14.0473415671826,-3.24881632189692));
#28774=CARTESIAN_POINT('Ctrl Pts',(368.453111834642,-14.0532380705072,-3.31919913489236));
#28775=CARTESIAN_POINT('Ctrl Pts',(368.55121950369,-14.0591345738317,-3.3895819478878));
#28776=CARTESIAN_POINT('Ctrl Pts',(368.652328275925,-14.0650310771562,-3.45552386899358));
#28777=CARTESIAN_POINT('Ctrl Pts',(368.755990062825,-14.0709275804807,-3.51678526436531));
#28778=CARTESIAN_POINT('Ctrl Pts',(368.858639294538,-14.0767664875085,-3.57744826619613));
#28779=CARTESIAN_POINT('Ctrl Pts',(368.964101496172,-14.0826053945363,-3.63370479082797));
#28780=CARTESIAN_POINT('Ctrl Pts',(369.071963148423,-14.0884443015642,-3.68528572765585));
#28781=CARTESIAN_POINT('Ctrl Pts',(369.179694493783,-14.0942761546502,-3.73680434992329));
#28782=CARTESIAN_POINT('Ctrl Pts',(369.2898191601,-14.1001080077363,-3.78365844746453));
#28783=CARTESIAN_POINT('Ctrl Pts',(369.401896798964,-14.1059398608223,-3.82562346857523));
#28784=CARTESIAN_POINT('Ctrl Pts',(369.513867761825,-14.1117661631242,-3.86754854718911));
#28785=CARTESIAN_POINT('Ctrl Pts',(369.627787620653,-14.1175924654262,-3.90459366688072));
#28786=CARTESIAN_POINT('Ctrl Pts',(369.743194213509,-14.1234187677281,-3.93658153768663));
#28787=CARTESIAN_POINT('Ctrl Pts',(369.859083457493,-14.1292694366741,-3.96870318752134));
#28788=CARTESIAN_POINT('Ctrl Pts',(369.976471524561,-14.1351201056201,-3.99572501662337));
#28789=CARTESIAN_POINT('Ctrl Pts',(370.094872646103,-14.1409707745661,-4.01751736594451));
#28790=CARTESIAN_POINT('Ctrl Pts',(370.212659188833,-14.1467910747359,-4.03919659880189));
#28791=CARTESIAN_POINT('Ctrl Pts',(370.331447889633,-14.1526113749056,-4.05570044669782));
#28792=CARTESIAN_POINT('Ctrl Pts',(370.450748823307,-14.1584316750753,-4.06695215109405));
#28793=CARTESIAN_POINT('Ctrl Pts',(370.570034865771,-14.1642512487518,-4.07820245104606));
#28794=CARTESIAN_POINT('Ctrl Pts',(370.689832610125,-14.1700708224283,-4.08420187357412));
#28795=CARTESIAN_POINT('Ctrl Pts',(370.809646657491,-14.1758903961048,-4.08492549896578));
#28796=CARTESIAN_POINT('Ctrl Pts',(370.929473558449,-14.1817105941023,-4.08564920198762));
#28797=CARTESIAN_POINT('Ctrl Pts',(371.049316360235,-14.1875307920998,-4.08109598008354));
#28798=CARTESIAN_POINT('Ctrl Pts',(371.168679918398,-14.1933509900972,-4.0712930389954));
#28799=CARTESIAN_POINT('Ctrl Pts',(371.28913975247,-14.1992246427919,-4.06140006432988));
#28800=CARTESIAN_POINT('Ctrl Pts',(371.409111074852,-14.2050982954865,-4.0461604745554));
#28801=CARTESIAN_POINT('Ctrl Pts',(371.528091673987,-14.2109719481811,-4.02565558457548));
#28802=CARTESIAN_POINT('Ctrl Pts',(371.646155644711,-14.2168003501627,-4.00530866459122));
#28803=CARTESIAN_POINT('Ctrl Pts',(371.763243717384,-14.2226287521444,-3.97977743425995));
#28804=CARTESIAN_POINT('Ctrl Pts',(371.878877773692,-14.228457154126,-3.94919226836981));
#28805=CARTESIAN_POINT('Ctrl Pts',(371.995858474459,-14.2343534321771,-3.91825091550933));
#28806=CARTESIAN_POINT('Ctrl Pts',(372.111350668757,-14.2402497102282,-3.88213729285527));
#28807=CARTESIAN_POINT('Ctrl Pts',(372.224878418643,-14.2461459882793,-3.84103714039612));
#28808=CARTESIAN_POINT('Ctrl Pts',(372.338406168528,-14.2520422663304,-3.79993698793697));
#28809=CARTESIAN_POINT('Ctrl Pts',(372.449969103123,-14.2579385443815,-3.75385051885361));
#28810=CARTESIAN_POINT('Ctrl Pts',(372.559116219245,-14.2638348224326,-3.70301169274025));
#28811=CARTESIAN_POINT('Ctrl Pts',(372.667208109033,-14.2696740956988,-3.65266437267868));
#28812=CARTESIAN_POINT('Ctrl Pts',(372.773256689999,-14.2755133689651,-3.59750437989767));
#28813=CARTESIAN_POINT('Ctrl Pts',(372.876806066402,-14.2813526422313,-3.53772057955799));
#28814=CARTESIAN_POINT('Ctrl Pts',(372.980216768418,-14.2871840954829,-3.47801684229699));
#28815=CARTESIAN_POINT('Ctrl Pts',(373.081134578619,-14.2930155487344,-3.41370182303264));
#28816=CARTESIAN_POINT('Ctrl Pts',(373.179125350556,-14.298847001986,-3.34501162934537));
#28817=CARTESIAN_POINT('Ctrl Pts',(373.226995558795,-14.3016957690278,-3.31145526673294));
#28818=CARTESIAN_POINT('Ctrl Pts',(373.274167568559,-14.3045445360695,-3.27685548514191));
#28819=CARTESIAN_POINT('Ctrl Pts',(373.320592904309,-14.3073933031112,-3.2412437998941));
#28820=CARTESIAN_POINT('',(366.749318910897,-13.7603849713562,0.00293958966507201));
#28821=CARTESIAN_POINT('Ctrl Pts',(366.749318910896,-13.7603849714045,0.00293958867138478));
#28822=CARTESIAN_POINT('Ctrl Pts',(366.749233092332,-13.7661811969052,-0.116318166152711));
#28823=CARTESIAN_POINT('Ctrl Pts',(366.754373994896,-13.7719774224059,-0.235652147899815));
#28824=CARTESIAN_POINT('Ctrl Pts',(366.764734942895,-13.7777736479066,-0.354570072003375));
#28825=CARTESIAN_POINT('Ctrl Pts',(366.775093077567,-13.7835682995473,-0.47345570609983));
#28826=CARTESIAN_POINT('Ctrl Pts',(366.790668403739,-13.789362951188,-0.591925099556149));
#28827=CARTESIAN_POINT('Ctrl Pts',(366.811402223152,-13.7951576028288,-0.709489135451252));
#28828=CARTESIAN_POINT('Ctrl Pts',(366.832135340407,-13.8009520582315,-0.827049189997007));
#28829=CARTESIAN_POINT('Ctrl Pts',(366.858026532062,-13.8067465136342,-0.943703544737596));
#28830=CARTESIAN_POINT('Ctrl Pts',(366.888965739009,-13.8125409690369,-1.05897199909083));
#28831=CARTESIAN_POINT('Ctrl Pts',(366.919911251373,-13.818336605351,-1.17426394518391));
#28832=CARTESIAN_POINT('Ctrl Pts',(366.955906718432,-13.8241322416652,-1.28816903385626));
#28833=CARTESIAN_POINT('Ctrl Pts',(366.996792032616,-13.8299278779794,-1.40022161680409));
#28834=CARTESIAN_POINT('Ctrl Pts',(367.037719238015,-13.8357294525199,-1.51238900916566));
#28835=CARTESIAN_POINT('Ctrl Pts',(367.08354615477,-13.8415310270605,-1.62269972028456));
#28836=CARTESIAN_POINT('Ctrl Pts',(367.134064194678,-13.8473326016011,-1.73070733008778));
#28837=CARTESIAN_POINT('Ctrl Pts',(367.184610154335,-13.8531373824913,-1.8387746323355));
#28838=CARTESIAN_POINT('Ctrl Pts',(367.239852212216,-13.8589421633816,-1.94453593504841));
#28839=CARTESIAN_POINT('Ctrl Pts',(367.299536225143,-13.8647469442719,-2.04757022877807));
#28840=CARTESIAN_POINT('Ctrl Pts',(367.359310356431,-13.8705604899438,-2.15076009652668));
#28841=CARTESIAN_POINT('Ctrl Pts',(367.423539618352,-13.8763740356158,-2.25121438642522));
#28842=CARTESIAN_POINT('Ctrl Pts',(367.491926831069,-13.8821875812877,-2.3485415165621));
#28843=CARTESIAN_POINT('Ctrl Pts',(367.536710380988,-13.8859945972848,-2.41227644912965));
#28844=CARTESIAN_POINT('Ctrl Pts',(367.583276142426,-13.8898016132819,-2.47467100927438));
#28845=CARTESIAN_POINT('Ctrl Pts',(367.631531783043,-13.893608629279,-2.53562347138825));
#28846=CARTESIAN_POINT('Ctrl Pts',(367.7055419637,-13.8994474895263,-2.62910689995473));
#28847=CARTESIAN_POINT('Ctrl Pts',(367.78376005255,-13.9052863497737,-2.7194883031148));
#28848=CARTESIAN_POINT('Ctrl Pts',(367.865896788345,-13.911125210021,-2.80636800537333));
#28849=CARTESIAN_POINT('Ctrl Pts',(367.947934297171,-13.9169570165134,-2.89314275082489));
#28850=CARTESIAN_POINT('Ctrl Pts',(368.03388075901,-13.9227888230059,-2.97642391827985));
#28851=CARTESIAN_POINT('Ctrl Pts',(368.12340586915,-13.9286206294983,-3.05584378111874));
#28852=CARTESIAN_POINT('Ctrl Pts',(368.212845771952,-13.9344468854507,-3.13518805449391));
#28853=CARTESIAN_POINT('Ctrl Pts',(368.305857244036,-13.9402731414031,-3.21067806775095));
#28854=CARTESIAN_POINT('Ctrl Pts',(368.402072647356,-13.9460993973555,-3.28198236718782));
#28855=CARTESIAN_POINT('Ctrl Pts',(368.498691497845,-13.951950083767,-3.35358565739715));
#28856=CARTESIAN_POINT('Ctrl Pts',(368.598540923152,-13.9578007701785,-3.42096775296308));
#28857=CARTESIAN_POINT('Ctrl Pts',(368.701214132483,-13.96365145659,-3.4838331642831));
#28858=CARTESIAN_POINT('Ctrl Pts',(368.803353298552,-13.9694717113078,-3.54637158816914));
#28859=CARTESIAN_POINT('Ctrl Pts',(368.908286589121,-13.9752919660257,-3.60443999606237));
#28860=CARTESIAN_POINT('Ctrl Pts',(369.015584346616,-13.9811122207435,-3.65779078569854));
#28861=CARTESIAN_POINT('Ctrl Pts',(369.122868718803,-13.9869317493893,-3.71113491986678));
#28862=CARTESIAN_POINT('Ctrl Pts',(369.232516607959,-13.9927512780351,-3.75976242596029));
#28863=CARTESIAN_POINT('Ctrl Pts',(369.344074628949,-13.9985708066808,-3.80347211538398));
#28864=CARTESIAN_POINT('Ctrl Pts',(369.455644626994,-14.0043909601208,-3.8471864975522));
#28865=CARTESIAN_POINT('Ctrl Pts',(369.569124786904,-14.0102111135608,-3.88598186527154));
#28866=CARTESIAN_POINT('Ctrl Pts',(369.684043239005,-14.0160312670008,-3.91970576853471));
#28867=CARTESIAN_POINT('Ctrl Pts',(369.800019299583,-14.02190498402,-3.95374003697664));
#28868=CARTESIAN_POINT('Ctrl Pts',(369.917459859636,-14.0277787010391,-3.98260889101293));
#28869=CARTESIAN_POINT('Ctrl Pts',(370.035866992001,-14.0336524180583,-4.00620783562352));
#28870=CARTESIAN_POINT('Ctrl Pts',(370.153359760542,-14.0394807770468,-4.02962454441117));
#28871=CARTESIAN_POINT('Ctrl Pts',(370.271803812536,-14.0453091360352,-4.04785244622414));
#28872=CARTESIAN_POINT('Ctrl Pts',(370.390706113024,-14.0511374950237,-4.06084149209945));
#28873=CARTESIAN_POINT('Ctrl Pts',(370.510996413344,-14.0570338910582,-4.07398216492748));
#28874=CARTESIAN_POINT('Ctrl Pts',(370.631755301709,-14.0629302870927,-4.08176086392417));
#28875=CARTESIAN_POINT('Ctrl Pts',(370.752471851296,-14.0688266831273,-4.08417999505018));
#28876=CARTESIAN_POINT('Ctrl Pts',(370.873188400882,-14.0747230791618,-4.08659912617619));
#28877=CARTESIAN_POINT('Ctrl Pts',(370.993862188928,-14.0806194751964,-4.08365875519713));
#28878=CARTESIAN_POINT('Ctrl Pts',(371.113988241904,-14.0865158712309,-4.07541525168848));
#28879=CARTESIAN_POINT('Ctrl Pts',(371.232928481495,-14.0923540615293,-4.06725312317356));
#28880=CARTESIAN_POINT('Ctrl Pts',(371.351690459257,-14.0981922518276,-4.05386751480068));
#28881=CARTESIAN_POINT('Ctrl Pts',(371.46978113535,-14.104030442126,-4.03527092238788));
#28882=CARTESIAN_POINT('Ctrl Pts',(371.587736952339,-14.1098619652332,-4.01669556721319));
#28883=CARTESIAN_POINT('Ctrl Pts',(371.70502259486,-14.1156934883403,-3.99292112540638));
#28884=CARTESIAN_POINT('Ctrl Pts',(371.821148058735,-14.1215250114475,-3.96401200117885));
#28885=CARTESIAN_POINT('Ctrl Pts',(371.937167875275,-14.1273512292163,-3.93512917757356));
#28886=CARTESIAN_POINT('Ctrl Pts',(372.052029221206,-14.1331774469851,-3.90112106157912));
#28887=CARTESIAN_POINT('Ctrl Pts',(372.165250828261,-14.1390036647538,-3.86210336681422));
#28888=CARTESIAN_POINT('Ctrl Pts',(372.278394693045,-14.1448258820194,-3.82311246308595));
#28889=CARTESIAN_POINT('Ctrl Pts',(372.389900677209,-14.150648099285,-3.77911895777986));
#28890=CARTESIAN_POINT('Ctrl Pts',(372.49930185826,-14.1564703165505,-3.73028862998216));
#28891=CARTESIAN_POINT('Ctrl Pts',(372.608658062249,-14.1622901401835,-3.68147837733061));
#28892=CARTESIAN_POINT('Ctrl Pts',(372.715910815491,-14.1681099638165,-3.62783542500394));
#28893=CARTESIAN_POINT('Ctrl Pts',(372.820612903843,-14.1739297874495,-3.5695737801434));
#28894=CARTESIAN_POINT('Ctrl Pts',(372.925315203698,-14.1797496228389,-3.51131201759125));
#28895=CARTESIAN_POINT('Ctrl Pts',(373.027466470007,-14.1855694582282,-3.44843173395799));
#28896=CARTESIAN_POINT('Ctrl Pts',(373.126644151864,-14.1913892936176,-3.38119285764115));
#28897=CARTESIAN_POINT('Ctrl Pts',(373.192649407338,-14.1952625412525,-3.33644368498476));
#28898=CARTESIAN_POINT('Ctrl Pts',(373.257338109058,-14.1991357888874,-3.28976493221356));
#28899=CARTESIAN_POINT('Ctrl Pts',(373.320592904309,-14.2030090365224,-3.2412437998941));
#28900=CARTESIAN_POINT('Ctrl Pts',(373.320592904309,-12.9531485432512,-3.2412437998941));
#28901=CARTESIAN_POINT('Ctrl Pts',(373.415389105552,-12.9589780536625,-3.16852806339356));
#28902=CARTESIAN_POINT('Ctrl Pts',(373.507099306673,-12.9648075640739,-3.09156831113415));
#28903=CARTESIAN_POINT('Ctrl Pts',(373.595325455516,-12.9706370744852,-3.01065807093533));
#28904=CARTESIAN_POINT('Ctrl Pts',(373.683476099339,-12.9764615959301,-2.92981707471166));
#28905=CARTESIAN_POINT('Ctrl Pts',(373.768148326379,-12.982286117375,-2.84503259115645));
#28906=CARTESIAN_POINT('Ctrl Pts',(373.848976665281,-12.9881106388198,-2.75663875886719));
#28907=CARTESIAN_POINT('Ctrl Pts',(373.929761206976,-12.993932004221,-2.66829282318176));
#28908=CARTESIAN_POINT('Ctrl Pts',(374.006705730902,-12.9997533696222,-2.57634172817591));
#28909=CARTESIAN_POINT('Ctrl Pts',(374.079481548501,-13.0055747350234,-2.48115650269327));
#28910=CARTESIAN_POINT('Ctrl Pts',(374.152237640405,-13.0113945225588,-2.3859970769167));
#28911=CARTESIAN_POINT('Ctrl Pts',(374.220827027024,-13.0172143100941,-2.28760558614071));
#28912=CARTESIAN_POINT('Ctrl Pts',(374.284961616153,-13.0230340976295,-2.18638574395216));
#28913=CARTESIAN_POINT('Ctrl Pts',(374.34909370896,-13.0288536586401,-2.08516984156239));
#28914=CARTESIAN_POINT('Ctrl Pts',(374.408771132333,-13.0346732196508,-1.98112614958709));
#28915=CARTESIAN_POINT('Ctrl Pts',(374.46374974405,-13.0404927806615,-1.87468641373873));
#28916=CARTESIAN_POINT('Ctrl Pts',(374.518738977417,-13.0463134659884,-1.76822611415268));
#28917=CARTESIAN_POINT('Ctrl Pts',(374.569027407677,-13.0521341513154,-1.65936921051655));
#28918=CARTESIAN_POINT('Ctrl Pts',(374.614417649656,-13.0579548366423,-1.54857047918815));
#28919=CARTESIAN_POINT('Ctrl Pts',(374.659853002979,-13.0637813068896,-1.43766162992624));
#28920=CARTESIAN_POINT('Ctrl Pts',(374.700380292053,-13.069607777137,-1.32480747475849));
#28921=CARTESIAN_POINT('Ctrl Pts',(374.735850874107,-13.0754342473843,-1.2104813451526));
#28922=CARTESIAN_POINT('Ctrl Pts',(374.771340403745,-13.0812638300007,-1.09609414510564));
#28923=CARTESIAN_POINT('Ctrl Pts',(374.801767741011,-13.087093412617,-0.980233796070421));
#28924=CARTESIAN_POINT('Ctrl Pts',(374.827034985985,-13.0929229952334,-0.863385717831531));
#28925=CARTESIAN_POINT('Ctrl Pts',(374.852339369046,-13.0987611462372,-0.746365894946289));
#28926=CARTESIAN_POINT('Ctrl Pts',(374.87246844124,-13.104599297241,-0.628355842638248));
#28927=CARTESIAN_POINT('Ctrl Pts',(374.887375904404,-13.1104374482449,-0.509848441956565));
#28928=CARTESIAN_POINT('Ctrl Pts',(374.897200083234,-13.1142848526537,-0.431750788168268));
#28929=CARTESIAN_POINT('Ctrl Pts',(374.904757614425,-13.1181322570625,-0.353437235778988));
#28930=CARTESIAN_POINT('Ctrl Pts',(374.910047622374,-13.1219796614713,-0.275048811783993));
#28931=CARTESIAN_POINT('Ctrl Pts',(374.918075800169,-13.127818527299,-0.156085624782912));
#28932=CARTESIAN_POINT('Ctrl Pts',(374.920903302936,-13.1336573931267,-0.0365912520044337));
#28933=CARTESIAN_POINT('Ctrl Pts',(374.918475698036,-13.1394962589545,0.082943948910298));
#28934=CARTESIAN_POINT('Ctrl Pts',(374.916051025807,-13.1453280711314,0.202334745143395));
#28935=CARTESIAN_POINT('Ctrl Pts',(374.90838388312,-13.1511598833084,0.32176586896938));
#28936=CARTESIAN_POINT('Ctrl Pts',(374.89547170126,-13.1569916954854,0.440743034634737));
#28937=CARTESIAN_POINT('Ctrl Pts',(374.882571808608,-13.1628179572177,0.559606963427308));
#28938=CARTESIAN_POINT('Ctrl Pts',(374.864436852962,-13.16864421895,0.678017392453952));
#28939=CARTESIAN_POINT('Ctrl Pts',(374.841116288482,-13.1744704806823,0.795481803196109));
#28940=CARTESIAN_POINT('Ctrl Pts',(374.817697968761,-13.1803211649632,0.913438601751774));
#28941=CARTESIAN_POINT('Ctrl Pts',(374.789050479173,-13.1861718492441,1.03044101940979));
#28942=CARTESIAN_POINT('Ctrl Pts',(374.755276435948,-13.1920225335249,1.14599685538825));
#28943=CARTESIAN_POINT('Ctrl Pts',(374.721678017938,-13.1978427942147,1.26095180037127));
#28944=CARTESIAN_POINT('Ctrl Pts',(374.683006359508,-13.2036630549045,1.37447478173989));
#28945=CARTESIAN_POINT('Ctrl Pts',(374.639413194194,-13.2094833155943,1.48609368686157));
#28946=CARTESIAN_POINT('Ctrl Pts',(374.595825466632,-13.2153028502725,1.59769866879066));
#28947=CARTESIAN_POINT('Ctrl Pts',(374.547317600993,-13.2211223849508,1.70739966916459));
#28948=CARTESIAN_POINT('Ctrl Pts',(374.494090094668,-13.2269419196291,1.81474299578722));
#28949=CARTESIAN_POINT('Ctrl Pts',(374.44085687327,-13.2327620791546,1.92209784793244));
#28950=CARTESIAN_POINT('Ctrl Pts',(374.382903183838,-13.23858223868,2.02709415955572));
#28951=CARTESIAN_POINT('Ctrl Pts',(374.320475967924,-13.2444023982055,2.12930190421862));
#28952=CARTESIAN_POINT('Ctrl Pts',(374.257474381133,-13.2502761069737,2.2324500264256));
#28953=CARTESIAN_POINT('Ctrl Pts',(374.189916741048,-13.2561498157418,2.33275764285162));
#28954=CARTESIAN_POINT('Ctrl Pts',(374.118101511986,-13.2620235245099,2.42981272579799));
#28955=CARTESIAN_POINT('Ctrl Pts',(374.046840679252,-13.2678518896564,2.52611856680229));
#28956=CARTESIAN_POINT('Ctrl Pts',(373.971388066244,-13.2736802548028,2.61922163617767));
#28957=CARTESIAN_POINT('Ctrl Pts',(373.892075109945,-13.2795086199493,2.7087535064988));
#28958=CARTESIAN_POINT('Ctrl Pts',(373.811836593065,-13.2854050005283,2.79933018934163));
#28959=CARTESIAN_POINT('Ctrl Pts',(373.727647358567,-13.2913013811073,2.88625148480409));
#28960=CARTESIAN_POINT('Ctrl Pts',(373.639887342266,-13.2971977616862,2.96917578498761));
#28961=CARTESIAN_POINT('Ctrl Pts',(373.552127325965,-13.3030941422652,3.05210008517112));
#28962=CARTESIAN_POINT('Ctrl Pts',(373.460796885094,-13.3089905228442,3.13102715464025));
#28963=CARTESIAN_POINT('Ctrl Pts',(373.366307815629,-13.3148869034232,3.20565934407867));
#28964=CARTESIAN_POINT('Ctrl Pts',(373.272740512783,-13.320725763203,3.27956347617355));
#28965=CARTESIAN_POINT('Ctrl Pts',(373.175793742295,-13.3265646229828,3.34947909213848));
#28966=CARTESIAN_POINT('Ctrl Pts',(373.075841111034,-13.3324034827626,3.41508396451658));
#28967=CARTESIAN_POINT('Ctrl Pts',(372.976009228044,-13.3382352888789,3.48060958260274));
#28968=CARTESIAN_POINT('Ctrl Pts',(372.873179044464,-13.3440670949951,3.54183459581339));
#28969=CARTESIAN_POINT('Ctrl Pts',(372.767756739998,-13.3498989011114,3.59847732674655));
#28970=CARTESIAN_POINT('Ctrl Pts',(372.662434771708,-13.3557251567786,3.65506614769307));
#28971=CARTESIAN_POINT('Ctrl Pts',(372.554525946849,-13.3615514124459,3.70708117289297));
#28972=CARTESIAN_POINT('Ctrl Pts',(372.444464410948,-13.3673776681131,3.75428462728229));
#28973=CARTESIAN_POINT('Ctrl Pts',(372.333941360669,-13.3732283546657,3.80168601706065));
#28974=CARTESIAN_POINT('Ctrl Pts',(372.221247852402,-13.3790790412183,3.84423516805264));
#28975=CARTESIAN_POINT('Ctrl Pts',(372.106847839179,-13.3849297277708,3.88173832642591));
#28976=CARTESIAN_POINT('Ctrl Pts',(371.99304286882,-13.3907499824277,3.91904641500757));
#28977=CARTESIAN_POINT('Ctrl Pts',(371.877549495946,-13.3965702370845,3.95136075995291));
#28978=CARTESIAN_POINT('Ctrl Pts',(371.760842884978,-13.4023904917413,3.97853947643273));
#28979=CARTESIAN_POINT('Ctrl Pts',(371.644150831371,-13.4082100204105,4.00571480278401));
#28980=CARTESIAN_POINT('Ctrl Pts',(371.526246235741,-13.4140295490797,4.02775568302582));
#28981=CARTESIAN_POINT('Ctrl Pts',(371.407616651283,-13.4198490777489,4.04457086575872));
#28982=CARTESIAN_POINT('Ctrl Pts',(371.288974328835,-13.4256692312968,4.06138785404145));
#28983=CARTESIAN_POINT('Ctrl Pts',(371.169607264439,-13.4314893848447,4.07297797222377));
#28984=CARTESIAN_POINT('Ctrl Pts',(371.050009762303,-13.4373095383925,4.07930165596487));
#28985=CARTESIAN_POINT('Ctrl Pts',(370.929311587348,-13.4431832556411,4.08568353746661));
#28986=CARTESIAN_POINT('Ctrl Pts',(370.808379131339,-13.4490569728896,4.08670152332728));
#28987=CARTESIAN_POINT('Ctrl Pts',(370.687720999121,-13.4549306901382,4.08236871955081));
#28988=CARTESIAN_POINT('Ctrl Pts',(370.567994611619,-13.4607590494411,4.07806937449732));
#28989=CARTESIAN_POINT('Ctrl Pts',(370.448538728588,-13.4665874087439,4.06850168216696));
#28990=CARTESIAN_POINT('Ctrl Pts',(370.329844643048,-13.4724157680468,4.05373060035005));
#28991=CARTESIAN_POINT('Ctrl Pts',(370.209764990935,-13.4783121642682,4.03878708940899));
#28992=CARTESIAN_POINT('Ctrl Pts',(370.090465457346,-13.4842085604896,4.01851800387922));
#28993=CARTESIAN_POINT('Ctrl Pts',(369.972442652823,-13.490104956711,3.99304346819986));
#28994=CARTESIAN_POINT('Ctrl Pts',(369.8544198483,-13.4960013529323,3.96756893252049));
#28995=CARTESIAN_POINT('Ctrl Pts',(369.737674169058,-13.5018977491537,3.93688910814501));
#28996=CARTESIAN_POINT('Ctrl Pts',(369.622683992498,-13.5077941453751,3.90117525721957));
#28997=CARTESIAN_POINT('Ctrl Pts',(369.508815975897,-13.5136330001618,3.86580992870413));
#28998=CARTESIAN_POINT('Ctrl Pts',(369.396325883695,-13.5194718549485,3.8254017561411));
#28999=CARTESIAN_POINT('Ctrl Pts',(369.285690759097,-13.5253107097351,3.78007660283948));
#29000=CARTESIAN_POINT('Ctrl Pts',(369.175189290142,-13.5311425107412,3.73480620576969));
#29001=CARTESIAN_POINT('Ctrl Pts',(369.06653870332,-13.5369743117473,3.68463079724408));
#29002=CARTESIAN_POINT('Ctrl Pts',(368.960201023265,-13.5428061127534,3.62972603754946));
#29003=CARTESIAN_POINT('Ctrl Pts',(368.853964552685,-13.548632363201,3.57487353479583));
#29004=CARTESIAN_POINT('Ctrl Pts',(368.750036967426,-13.5544586136486,3.51530082231403));
#29005=CARTESIAN_POINT('Ctrl Pts',(368.648859903293,-13.5602848640961,3.45123145400047));
#29006=CARTESIAN_POINT('Ctrl Pts',(368.547258455213,-13.5661355525641,3.38689334877934));
#29007=CARTESIAN_POINT('Ctrl Pts',(368.448431036185,-13.5719862410321,3.31802093983099));
#29008=CARTESIAN_POINT('Ctrl Pts',(368.352799838286,-13.5778369295,3.24488726176098));
#29009=CARTESIAN_POINT('Ctrl Pts',(368.25766617898,-13.5836571787037,3.17213407486989));
#29010=CARTESIAN_POINT('Ctrl Pts',(368.1656958819,-13.5894774279074,3.0951641096098));
#29011=CARTESIAN_POINT('Ctrl Pts',(368.077274702612,-13.5952976771111,3.01428898177723));
#29012=CARTESIAN_POINT('Ctrl Pts',(367.988864553705,-13.6011172002493,2.93342394296956));
#29013=CARTESIAN_POINT('Ctrl Pts',(367.904002941103,-13.6069367233875,2.84865498445783));
#29014=CARTESIAN_POINT('Ctrl Pts',(367.823040870314,-13.6127562465257,2.76033257637481));
#29015=CARTESIAN_POINT('Ctrl Pts',(367.742070107115,-13.6185763944711,2.6720006856465));
#29016=CARTESIAN_POINT('Ctrl Pts',(367.664999992291,-13.6243965424165,2.58011488583731));
#29017=CARTESIAN_POINT('Ctrl Pts',(367.59214272374,-13.6302166903619,2.48506044790789));
#29018=CARTESIAN_POINT('Ctrl Pts',(367.518614774742,-13.636090415109,2.38913099566252));
#29019=CARTESIAN_POINT('Ctrl Pts',(367.449377892856,-13.6419641398561,2.28997459903167));
#29020=CARTESIAN_POINT('Ctrl Pts',(367.3847089292,-13.6478378646032,2.18801811493667));
#29021=CARTESIAN_POINT('Ctrl Pts',(367.320539496385,-13.6536662181784,2.08684918650043));
#29022=CARTESIAN_POINT('Ctrl Pts',(367.260867811579,-13.6594945717536,1.98292366137199));
#29023=CARTESIAN_POINT('Ctrl Pts',(367.205918170984,-13.6653229253289,1.87668344318415));
#29024=CARTESIAN_POINT('Ctrl Pts',(367.150326892175,-13.6712193356619,1.76920267486424));
#29025=CARTESIAN_POINT('Ctrl Pts',(367.099568817166,-13.6771157459949,1.65935320104759));
#29026=CARTESIAN_POINT('Ctrl Pts',(367.05382575592,-13.683012156328,1.54761251682033));
#29027=CARTESIAN_POINT('Ctrl Pts',(367.008082694673,-13.688908566661,1.43587183259306));
#29028=CARTESIAN_POINT('Ctrl Pts',(366.967354738134,-13.694804976994,1.32224035603285));
#29029=CARTESIAN_POINT('Ctrl Pts',(366.931771210358,-13.7007013873271,1.20720946825787));
#29030=CARTESIAN_POINT('Ctrl Pts',(366.889874249855,-13.7076439724576,1.07176914339708));
#29031=CARTESIAN_POINT('Ctrl Pts',(366.855006217274,-13.7145865575881,0.934062471553731));
#29032=CARTESIAN_POINT('Ctrl Pts',(366.827376047162,-13.7215291427186,0.794759311258914));
#29033=CARTESIAN_POINT('Ctrl Pts',(366.800005672858,-13.728406449405,0.65676596472998));
#29034=CARTESIAN_POINT('Ctrl Pts',(366.779737729344,-13.7352837560913,0.517206071648502));
#29035=CARTESIAN_POINT('Ctrl Pts',(366.766728357886,-13.7421610627776,0.376750179056597));
#29036=CARTESIAN_POINT('Ctrl Pts',(366.755237348061,-13.7482356989705,0.252687302766028));
#29037=CARTESIAN_POINT('Ctrl Pts',(366.749408851624,-13.7543103351634,0.127925664420039));
#29038=CARTESIAN_POINT('Ctrl Pts',(366.749318910897,-13.7603849713562,0.00293958966506929));
#29039=CARTESIAN_POINT('Origin',(370.834317853224,-8.23961502859548,0.));
#29040=CARTESIAN_POINT('',(373.320592904309,-11.7029891890582,-3.24124379989411));
#29041=CARTESIAN_POINT('',(373.320592904309,-11.8073874696441,-3.24124379989412));
#29042=CARTESIAN_POINT('',(373.320592904309,-8.23961502859548,-3.24124379989413));
#29043=CARTESIAN_POINT('',(366.749318160251,-11.2603849713631,0.00158379706420307));
#29044=CARTESIAN_POINT('Ctrl Pts',(366.749318160251,-11.2603849714045,0.00158379621223467));
#29045=CARTESIAN_POINT('Ctrl Pts',(366.749271660382,-11.2662079034056,-0.118350794889082));
#29046=CARTESIAN_POINT('Ctrl Pts',(366.754511367077,-11.2720308354067,-0.23832601982146));
#29047=CARTESIAN_POINT('Ctrl Pts',(366.765021606588,-11.2778537674077,-0.357845018286969));
#29048=CARTESIAN_POINT('Ctrl Pts',(366.775531340107,-11.283676419077,-0.477358262781803));
#29049=CARTESIAN_POINT('Ctrl Pts',(366.791311066522,-11.2894990707462,-0.59641492158895));
#29050=CARTESIAN_POINT('Ctrl Pts',(366.812293155352,-11.2953217224155,-0.714522448705577));
#29051=CARTESIAN_POINT('Ctrl Pts',(366.833279063491,-11.3011454339655,-0.832651474600536));
#29052=CARTESIAN_POINT('Ctrl Pts',(366.859469147176,-11.3069691455155,-0.949830626889041));
#29053=CARTESIAN_POINT('Ctrl Pts',(366.890744608621,-11.3127928570656,-1.06557733855915));
#29054=CARTESIAN_POINT('Ctrl Pts',(366.923424012687,-11.3188779926354,-1.18651987258203));
#29055=CARTESIAN_POINT('Ctrl Pts',(366.961655862029,-11.3249631282053,-1.3058978956442));
#29056=CARTESIAN_POINT('Ctrl Pts',(367.005246895972,-11.3310482637751,-1.4231797512366));
#29057=CARTESIAN_POINT('Ctrl Pts',(367.047033600812,-11.3368815221535,-1.53560705197797));
#29058=CARTESIAN_POINT('Ctrl Pts',(367.093744473723,-11.3427147805319,-1.64610789774426));
#29059=CARTESIAN_POINT('Ctrl Pts',(367.145160824468,-11.3485480389102,-1.75423641997932));
#29060=CARTESIAN_POINT('Ctrl Pts',(367.19661482878,-11.3543855691395,-1.86244412761821));
#29061=CARTESIAN_POINT('Ctrl Pts',(367.252780985196,-11.3602230993687,-1.96827569535019));
#29062=CARTESIAN_POINT('Ctrl Pts',(367.313395671236,-11.3660606295979,-2.07131165892109));
#29063=CARTESIAN_POINT('Ctrl Pts',(367.374098204497,-11.3719066200014,-2.1744969497207));
#29064=CARTESIAN_POINT('Ctrl Pts',(367.439261914381,-11.377752610405,-2.2748782131449));
#29065=CARTESIAN_POINT('Ctrl Pts',(367.508581043213,-11.3835986008085,-2.37206654007454));
#29066=CARTESIAN_POINT('Ctrl Pts',(367.517339358752,-11.384337228507,-2.38434606591743));
#29067=CARTESIAN_POINT('Ctrl Pts',(367.526163959873,-11.3850758562054,-2.39657466641323));
#29068=CARTESIAN_POINT('Ctrl Pts',(367.535054186773,-11.3858144839039,-2.40875159766206));
#29069=CARTESIAN_POINT('Ctrl Pts',(367.605317058358,-11.3916521417843,-2.50499055378519));
#29070=CARTESIAN_POINT('Ctrl Pts',(367.679902869804,-11.3974897996647,-2.59830131414769));
#29071=CARTESIAN_POINT('Ctrl Pts',(367.758539379142,-11.403327457545,-2.68827301038714));
#29072=CARTESIAN_POINT('Ctrl Pts',(367.837078657014,-11.4091578973528,-2.77813345957347));
#29073=CARTESIAN_POINT('Ctrl Pts',(367.919658404463,-11.4149883371606,-2.86466275422529));
#29074=CARTESIAN_POINT('Ctrl Pts',(368.005964041971,-11.4208187769684,-2.94748023205755));
#29075=CARTESIAN_POINT('Ctrl Pts',(368.092185149825,-11.4266435063142,-3.03021659661654));
#29076=CARTESIAN_POINT('Ctrl Pts',(368.182124595608,-11.43246823566,-3.10924809789295));
#29077=CARTESIAN_POINT('Ctrl Pts',(368.275428991747,-11.4382929650058,-3.18422875977987));
#29078=CARTESIAN_POINT('Ctrl Pts',(368.369157386334,-11.4441441633745,-3.25955015249597));
#29079=CARTESIAN_POINT('Ctrl Pts',(368.46628111593,-11.4499953617433,-3.33078348678459));
#29080=CARTESIAN_POINT('Ctrl Pts',(368.566405734061,-11.4558465601121,-3.39761675586779));
#29081=CARTESIAN_POINT('Ctrl Pts',(368.665968312269,-11.461664913341,-3.46407486281691));
#29082=CARTESIAN_POINT('Ctrl Pts',(368.76849782855,-11.4674832665699,-3.52618195619947));
#29083=CARTESIAN_POINT('Ctrl Pts',(368.873575460687,-11.4733016197989,-3.58367329288085));
#29084=CARTESIAN_POINT('Ctrl Pts',(368.978637520203,-11.4791191107415,-3.64115610928314));
#29085=CARTESIAN_POINT('Ctrl Pts',(369.086246588171,-11.4849366016841,-3.69402433492965));
#29086=CARTESIAN_POINT('Ctrl Pts',(369.195958220374,-11.4907540926267,-3.74205861972375));
#29087=CARTESIAN_POINT('Ctrl Pts',(369.30567913085,-11.4965720755524,-3.79009696675955));
#29088=CARTESIAN_POINT('Ctrl Pts',(369.417502586998,-11.5023900584781,-3.83330039746001));
#29089=CARTESIAN_POINT('Ctrl Pts',(369.530963669884,-11.5082080414038,-3.87149749745121));
#29090=CARTESIAN_POINT('Ctrl Pts',(369.645558927073,-11.5140841817748,-3.91007642148396));
#29091=CARTESIAN_POINT('Ctrl Pts',(369.761824334618,-11.5199603221458,-3.94354822893277));
#29092=CARTESIAN_POINT('Ctrl Pts',(369.879265776766,-11.5258364625168,-3.9717880773341));
#29093=CARTESIAN_POINT('Ctrl Pts',(369.99570284113,-11.5316623492061,-3.99978641408623));
#29094=CARTESIAN_POINT('Ctrl Pts',(370.113295489678,-11.5374882358954,-4.02264191374151));
#29095=CARTESIAN_POINT('Ctrl Pts',(370.231553464511,-11.5433141225848,-4.04028465478602));
#29096=CARTESIAN_POINT('Ctrl Pts',(370.351341566586,-11.5492153897966,-4.05815567336308));
#29097=CARTESIAN_POINT('Ctrl Pts',(370.471811904407,-11.5551166570084,-4.07067804364192));
#29098=CARTESIAN_POINT('Ctrl Pts',(370.592452268245,-11.5610179242203,-4.0778334981706));
#29099=CARTESIAN_POINT('Ctrl Pts',(370.713092632082,-11.5669191914321,-4.08498895269929));
#29100=CARTESIAN_POINT('Ctrl Pts',(370.833902593644,-11.572820458644,-4.08677753983674));
#29101=CARTESIAN_POINT('Ctrl Pts',(370.954373694032,-11.5787217258558,-4.08323543223847));
#29102=CARTESIAN_POINT('Ctrl Pts',(371.073698652196,-11.5845668493826,-4.07972702366896));
#29103=CARTESIAN_POINT('Ctrl Pts',(371.193044864443,-11.5904119729093,-4.07097858147516));
#29104=CARTESIAN_POINT('Ctrl Pts',(371.311918092408,-11.5962570964361,-4.05698447267567));
#29105=CARTESIAN_POINT('Ctrl Pts',(371.430658839178,-11.6020957057211,-4.04300595995514));
#29106=CARTESIAN_POINT('Ctrl Pts',(371.548927251579,-11.6079343150061,-4.02379345434519));
#29107=CARTESIAN_POINT('Ctrl Pts',(371.666230227338,-11.613772924291,-3.99939330421453));
#29108=CARTESIAN_POINT('Ctrl Pts',(371.783429498612,-11.6196063718147,-3.97501472561675));
#29109=CARTESIAN_POINT('Ctrl Pts',(371.899664637159,-11.6254398193383,-3.94545770783133));
#29110=CARTESIAN_POINT('Ctrl Pts',(372.014449378726,-11.6312732668619,-3.91082019306902));
#29111=CARTESIAN_POINT('Ctrl Pts',(372.132045556661,-11.6372495937116,-3.87533429752578));
#29112=CARTESIAN_POINT('Ctrl Pts',(372.248118935508,-11.6432259205613,-3.83451584958903));
#29113=CARTESIAN_POINT('Ctrl Pts',(372.362159242034,-11.649202247411,-3.78852552989119));
#29114=CARTESIAN_POINT('Ctrl Pts',(372.473359808257,-11.6550297565598,-3.74368042427057));
#29115=CARTESIAN_POINT('Ctrl Pts',(372.582626971052,-11.6608572657087,-3.69391815786364));
#29116=CARTESIAN_POINT('Ctrl Pts',(372.689505290836,-11.6666847748575,-3.63943739763784));
#29117=CARTESIAN_POINT('Ctrl Pts',(372.800477654598,-11.6727355105577,-3.58286971624134));
#29118=CARTESIAN_POINT('Ctrl Pts',(372.908874080937,-11.6787862462578,-3.52121500301371));
#29119=CARTESIAN_POINT('Ctrl Pts',(373.014211161153,-11.6848369819579,-3.45474892952387));
#29120=CARTESIAN_POINT('Ctrl Pts',(373.119548241369,-11.690887717658,-3.38828285603403));
#29121=CARTESIAN_POINT('Ctrl Pts',(373.221825568593,-11.6969384533581,-3.3170056918752));
#29122=CARTESIAN_POINT('Ctrl Pts',(373.320592904309,-11.7029891890582,-3.2412437998941));
#29123=CARTESIAN_POINT('',(369.776413430251,-11.,3.94563850749837));
#29124=CARTESIAN_POINT('Ctrl Pts',(369.776413430251,-11.,3.94563850749839));
#29125=CARTESIAN_POINT('Ctrl Pts',(369.658555082909,-11.0059425548389,3.91403833259629));
#29126=CARTESIAN_POINT('Ctrl Pts',(369.54203182805,-11.0118851096777,3.87713126827553));
#29127=CARTESIAN_POINT('Ctrl Pts',(369.427338766957,-11.0178276645166,3.83505343519563));
#29128=CARTESIAN_POINT('Ctrl Pts',(369.312716174018,-11.0237665682116,3.79300145500712));
#29129=CARTESIAN_POINT('Ctrl Pts',(369.199921894619,-11.0297054719065,3.74578516541319));
#29130=CARTESIAN_POINT('Ctrl Pts',(369.089435035688,-11.0356443756014,3.69359025245994));
#29131=CARTESIAN_POINT('Ctrl Pts',(368.978992730761,-11.0415808844239,3.64141638718932));
#29132=CARTESIAN_POINT('Ctrl Pts',(368.870856339153,-11.0475173932464,3.58426806167526));
#29133=CARTESIAN_POINT('Ctrl Pts',(368.765483899815,-11.0534539020689,3.5223786101474));
#29134=CARTESIAN_POINT('Ctrl Pts',(368.660107526221,-11.0593906325409,3.46048684787291));
#29135=CARTESIAN_POINT('Ctrl Pts',(368.557495646737,-11.0653273630128,3.39385379192271));
#29136=CARTESIAN_POINT('Ctrl Pts',(368.458080684342,-11.0712640934848,3.32275817916765));
#29137=CARTESIAN_POINT('Ctrl Pts',(368.358660266531,-11.0772011497362,3.2516586650261));
#29138=CARTESIAN_POINT('Ctrl Pts',(368.262437427882,-11.0831382059875,3.17609632917323));
#29139=CARTESIAN_POINT('Ctrl Pts',(368.169814137957,-11.0890752622388,3.09639224765349));
#29140=CARTESIAN_POINT('Ctrl Pts',(368.077167996229,-11.0950137832669,3.01666850172726));
#29141=CARTESIAN_POINT('Ctrl Pts',(367.988123463082,-11.100952304295,2.9328012252537));
#29142=CARTESIAN_POINT('Ctrl Pts',(367.90304779981,-11.1068908253231,2.84515041324005));
#29143=CARTESIAN_POINT('Ctrl Pts',(367.817934820676,-11.1128319511035,2.75746115585251));
#29144=CARTESIAN_POINT('Ctrl Pts',(367.736794445859,-11.118773076884,2.6659853329638));
#29145=CARTESIAN_POINT('Ctrl Pts',(367.659955363951,-11.1247142026645,2.57111800326221));
#29146=CARTESIAN_POINT('Ctrl Pts',(367.583016261277,-11.1306630619568,2.47612718558003));
#29147=CARTESIAN_POINT('Ctrl Pts',(367.510389879206,-11.1366119212492,2.37773634013093));
#29148=CARTESIAN_POINT('Ctrl Pts',(367.442363466651,-11.1425607805416,2.27637221020805));
#29149=CARTESIAN_POINT('Ctrl Pts',(367.374291336794,-11.1485136377782,2.17493995829567));
#29150=CARTESIAN_POINT('Ctrl Pts',(367.310825540233,-11.1544664950147,2.07053076535526));
#29151=CARTESIAN_POINT('Ctrl Pts',(367.252208140915,-11.1604193522512,1.96359746612641));
#29152=CARTESIAN_POINT('Ctrl Pts',(367.193491815945,-11.166382255827,1.85648370092013));
#29153=CARTESIAN_POINT('Ctrl Pts',(367.139640412308,-11.1723451594028,1.74683766006762));
#29154=CARTESIAN_POINT('Ctrl Pts',(367.090848866821,-11.1783080629785,1.63513453508797));
#29155=CARTESIAN_POINT('Ctrl Pts',(367.051029535186,-11.1831744559697,1.54397235250682));
#29156=CARTESIAN_POINT('Ctrl Pts',(367.014579378245,-11.1880408489608,1.45144053637299));
#29157=CARTESIAN_POINT('Ctrl Pts',(366.981579687489,-11.1929072419519,1.35780470844867));
#29158=CARTESIAN_POINT('Ctrl Pts',(366.93694994957,-11.1994886928329,1.23116890174215));
#29159=CARTESIAN_POINT('Ctrl Pts',(366.898524370235,-11.2060701437139,1.10220791307046));
#29160=CARTESIAN_POINT('Ctrl Pts',(366.86652191129,-11.2126515945948,0.971504175580758));
#29161=CARTESIAN_POINT('Ctrl Pts',(366.834629314539,-11.2192104518171,0.84124913484363));
#29162=CARTESIAN_POINT('Ctrl Pts',(366.809115930347,-11.2257693090393,0.709263473234092));
#29163=CARTESIAN_POINT('Ctrl Pts',(366.79015143706,-11.2323281662616,0.576144945624114));
#29164=CARTESIAN_POINT('Ctrl Pts',(366.771298075538,-11.2388485886377,0.44380649142543));
#29165=CARTESIAN_POINT('Ctrl Pts',(366.758917173706,-11.2453690110138,0.310348606542818));
#29166=CARTESIAN_POINT('Ctrl Pts',(366.753127314955,-11.2518894333899,0.176376841858498));
#29167=CARTESIAN_POINT('Ctrl Pts',(366.750612755721,-11.254721279381,0.118192358882813));
#29168=CARTESIAN_POINT('Ctrl Pts',(366.749340774381,-11.2575531253721,0.0599111639190462));
#29169=CARTESIAN_POINT('Ctrl Pts',(366.749318160251,-11.2603849713631,0.00158379706420297));
#29170=CARTESIAN_POINT('',(371.893335409592,-11.,3.94533988590394));
#29171=CARTESIAN_POINT('Origin',(370.834317853224,-11.,0.));
#29172=CARTESIAN_POINT('',(366.749317884331,-11.3646150285611,-0.000504124207611034));
#29173=CARTESIAN_POINT('Ctrl Pts',(371.893335409592,-11.,3.94533988590394));
#29174=CARTESIAN_POINT('Ctrl Pts',(371.779439084971,-11.0057722725029,3.9759122094216));
#29175=CARTESIAN_POINT('Ctrl Pts',(371.664032071455,-11.0115445450058,4.00159818186356));
#29176=CARTESIAN_POINT('Ctrl Pts',(371.547575100626,-11.0173168175087,4.02224925868946));
#29177=CARTESIAN_POINT('Ctrl Pts',(371.431254230685,-11.0230823440745,4.04287620102291));
#29178=CARTESIAN_POINT('Ctrl Pts',(371.313886249872,-11.0288478706402,4.05847987589247));
#29179=CARTESIAN_POINT('Ctrl Pts',(371.195946097017,-11.0346133972059,4.06896178567588));
#29180=CARTESIAN_POINT('Ctrl Pts',(371.074312838115,-11.0405594619557,4.07977191959225));
#29181=CARTESIAN_POINT('Ctrl Pts',(370.952071411611,-11.0465055267056,4.08513411645457));
#29182=CARTESIAN_POINT('Ctrl Pts',(370.829753664507,-11.0524515914554,4.08499745020497));
#29183=CARTESIAN_POINT('Ctrl Pts',(370.711326098722,-11.0582085481604,4.08486513047502));
#29184=CARTESIAN_POINT('Ctrl Pts',(370.592827443816,-11.0639655048653,4.07957840674844));
#29185=CARTESIAN_POINT('Ctrl Pts',(370.474743937419,-11.0697224615703,4.06914384103981));
#29186=CARTESIAN_POINT('Ctrl Pts',(370.356692365384,-11.0754778613708,4.05871209724262));
#29187=CARTESIAN_POINT('Ctrl Pts',(370.239056132905,-11.0812332611713,4.04313531578104));
#29188=CARTESIAN_POINT('Ctrl Pts',(370.122318273177,-11.0869886609718,4.02247207547947));
#29189=CARTESIAN_POINT('Ctrl Pts',(370.005583211736,-11.0927439228114,4.00180933049004));
#29190=CARTESIAN_POINT('Ctrl Pts',(369.889746889886,-11.098499184651,3.97606044244825));
#29191=CARTESIAN_POINT('Ctrl Pts',(369.775283298204,-11.1042544464906,3.94533532304586));
#29192=CARTESIAN_POINT('Ctrl Pts',(369.660794237774,-11.1100109889061,3.91460336714373));
#29193=CARTESIAN_POINT('Ctrl Pts',(369.547678916266,-11.1157675313215,3.87889308758316));
#29194=CARTESIAN_POINT('Ctrl Pts',(369.436396562165,-11.121524073737,3.83836437353257));
#29195=CARTESIAN_POINT('Ctrl Pts',(369.32500564356,-11.1272862321027,3.79779612060125));
#29196=CARTESIAN_POINT('Ctrl Pts',(369.215451652393,-11.1330483904685,3.75240019435146));
#29197=CARTESIAN_POINT('Ctrl Pts',(369.108174193521,-11.1388105488342,3.70238478093063));
#29198=CARTESIAN_POINT('Ctrl Pts',(369.000833722416,-11.1445760917551,3.65233998964304));
#29199=CARTESIAN_POINT('Ctrl Pts',(368.895772814035,-11.1503416346759,3.59767050111718));
#29200=CARTESIAN_POINT('Ctrl Pts',(368.793405326633,-11.1561071775967,3.53862982788566));
#29201=CARTESIAN_POINT('Ctrl Pts',(368.690901453063,-11.1618804020609,3.4795104936326));
#29202=CARTESIAN_POINT('Ctrl Pts',(368.591098510422,-11.1676536265252,3.41600857687091));
#29203=CARTESIAN_POINT('Ctrl Pts',(368.494380284798,-11.1734268509894,3.34842010146105));
#29204=CARTESIAN_POINT('Ctrl Pts',(368.472645635539,-11.1747242177269,3.33323152870201));
#29205=CARTESIAN_POINT('Ctrl Pts',(368.451066625825,-11.1760215844643,3.31783674250088));
#29206=CARTESIAN_POINT('Ctrl Pts',(368.429647365639,-11.1773189512017,3.30223936838908));
#29207=CARTESIAN_POINT('Ctrl Pts',(368.33357121294,-11.1831382934053,3.23227730229304));
#29208=CARTESIAN_POINT('Ctrl Pts',(368.240402810823,-11.1889576356089,3.15801106487821));
#29209=CARTESIAN_POINT('Ctrl Pts',(368.150551312676,-11.1947769778125,3.07971137541123));
#29210=CARTESIAN_POINT('Ctrl Pts',(368.060807061285,-11.2005893740488,3.00150514445892));
#29211=CARTESIAN_POINT('Ctrl Pts',(367.974372144894,-11.2064017702852,2.91927530397612));
#29212=CARTESIAN_POINT('Ctrl Pts',(367.891625510157,-11.2122141665215,2.83333492091153));
#29213=CARTESIAN_POINT('Ctrl Pts',(367.808956003466,-11.2180211450299,2.74747464278148));
#29214=CARTESIAN_POINT('Ctrl Pts',(367.729968221061,-11.2238281235382,2.65791099598431));
#29215=CARTESIAN_POINT('Ctrl Pts',(367.655006396492,-11.2296351020466,2.56499584036495));
#29216=CARTESIAN_POINT('Ctrl Pts',(367.580092479708,-11.2354383693394,2.47214006642955));
#29217=CARTESIAN_POINT('Ctrl Pts',(367.509199657806,-11.2412416366323,2.37593736242979));
#29218=CARTESIAN_POINT('Ctrl Pts',(367.442633400948,-11.2470449039252,2.27677437972832));
#29219=CARTESIAN_POINT('Ctrl Pts',(367.376089151854,-11.2528462525742,2.17764418173846));
#29220=CARTESIAN_POINT('Ctrl Pts',(367.313868851014,-11.2586476012233,2.07555599032896));
#29221=CARTESIAN_POINT('Ctrl Pts',(367.256235632751,-11.2644489498723,1.97092684378053));
#29222=CARTESIAN_POINT('Ctrl Pts',(367.198607821631,-11.2702497542395,1.86630751352781));
#29223=CARTESIAN_POINT('Ctrl Pts',(367.145566434097,-11.2760505586066,1.75914806051596));
#29224=CARTESIAN_POINT('Ctrl Pts',(367.097329153327,-11.2818513629737,1.64989104393092));
#29225=CARTESIAN_POINT('Ctrl Pts',(367.049084975963,-11.2876529966951,1.54061840662022));
#29226=CARTESIAN_POINT('Ctrl Pts',(367.005646435884,-11.2934546304165,1.42924798358644));
#29227=CARTESIAN_POINT('Ctrl Pts',(366.967183223484,-11.2992562641379,1.31624266587345));
#29228=CARTESIAN_POINT('Ctrl Pts',(366.928683436374,-11.305063414639,1.2031298912836));
#29229=CARTESIAN_POINT('Ctrl Pts',(366.895168557871,-11.31087056514,1.08837950474184));
#29230=CARTESIAN_POINT('Ctrl Pts',(366.866758541716,-11.3166777156411,0.972470107339642));
#29231=CARTESIAN_POINT('Ctrl Pts',(366.838334371929,-11.322487759216,0.856502964844621));
#29232=CARTESIAN_POINT('Ctrl Pts',(366.815020211601,-11.3282978027909,0.739376061951449));
#29233=CARTESIAN_POINT('Ctrl Pts',(366.796884646067,-11.3341078463658,0.621577105232758));
#29234=CARTESIAN_POINT('Ctrl Pts',(366.778722266324,-11.3399264803387,0.50360397771694));
#29235=CARTESIAN_POINT('Ctrl Pts',(366.765753822078,-11.3457451143116,0.384957217836436));
#29236=CARTESIAN_POINT('Ctrl Pts',(366.757995936781,-11.3515637482845,0.266128979116804));
#29237=CARTESIAN_POINT('Ctrl Pts',(366.752195587086,-11.3559141750434,0.177284492275928));
#29238=CARTESIAN_POINT('Ctrl Pts',(366.749306920368,-11.3602646018023,0.0883386385946549));
#29239=CARTESIAN_POINT('Ctrl Pts',(366.749317884331,-11.3646150285611,-0.000504124207612033));
#29240=CARTESIAN_POINT('Ctrl Pts',(366.749317884331,-11.3646150285955,-0.000504124909455006));
#29241=CARTESIAN_POINT('Ctrl Pts',(366.749322598097,-11.3664854167815,-0.0387004819959074));
#29242=CARTESIAN_POINT('Ctrl Pts',(366.749863028343,-11.3683558049676,-0.0768922472437367));
#29243=CARTESIAN_POINT('Ctrl Pts',(366.750938849501,-11.3702261931536,-0.115069161598965));
#29244=CARTESIAN_POINT('Ctrl Pts',(366.75429518582,-11.3760614119119,-0.234173125385912));
#29245=CARTESIAN_POINT('Ctrl Pts',(366.762871991954,-11.3818966306702,-0.353312031471976));
#29246=CARTESIAN_POINT('Ctrl Pts',(366.776677225411,-11.3877318494285,-0.471993151986081));
#29247=CARTESIAN_POINT('Ctrl Pts',(366.790465659685,-11.3935599674804,-0.590529852928814));
#29248=CARTESIAN_POINT('Ctrl Pts',(366.809469818492,-11.3993880855323,-0.708609476083606));
#29249=CARTESIAN_POINT('Ctrl Pts',(366.833645657319,-11.4052162035842,-0.825740262378583));
#29250=CARTESIAN_POINT('Ctrl Pts',(366.857798298364,-11.4110387293002,-0.942758656527254));
#29251=CARTESIAN_POINT('Ctrl Pts',(366.88711266417,-11.4168612550162,-1.05882962943746));
#29252=CARTESIAN_POINT('Ctrl Pts',(366.921493086368,-11.4226837807323,-1.17346808387846));
#29253=CARTESIAN_POINT('Ctrl Pts',(366.95604795318,-11.4285358496645,-1.28868820833842));
#29254=CARTESIAN_POINT('Ctrl Pts',(366.995720380752,-11.4343879185967,-1.40246082410072));
#29255=CARTESIAN_POINT('Ctrl Pts',(367.040361389904,-11.440239987529,-1.51430490801364));
#29256=CARTESIAN_POINT('Ctrl Pts',(367.08473066592,-11.4460564344832,-1.62546818868625));
#29257=CARTESIAN_POINT('Ctrl Pts',(367.13400804007,-11.4518728814375,-1.73472597299548));
#29258=CARTESIAN_POINT('Ctrl Pts',(367.187997909219,-11.4576893283918,-1.84162316067947));
#29259=CARTESIAN_POINT('Ctrl Pts',(367.241980833302,-11.4635050271389,-1.94850659748858));
#29260=CARTESIAN_POINT('Ctrl Pts',(367.300674863371,-11.4693207258861,-2.05302967914904));
#29261=CARTESIAN_POINT('Ctrl Pts',(367.363837598286,-11.4751364246333,-2.15476026510718));
#29262=CARTESIAN_POINT('Ctrl Pts',(367.427006927125,-11.480952730515,-2.25650147131213));
#29263=CARTESIAN_POINT('Ctrl Pts',(367.494645674013,-11.4867690363968,-2.35544925703979));
#29264=CARTESIAN_POINT('Ctrl Pts',(367.566467450474,-11.4925853422785,-2.45119945032005));
#29265=CARTESIAN_POINT('Ctrl Pts',(367.639063491327,-11.4984643500141,-2.54798186486703));
#29266=CARTESIAN_POINT('Ctrl Pts',(367.715933039427,-11.5043433577497,-2.64149699004699));
#29267=CARTESIAN_POINT('Ctrl Pts',(367.796738524552,-11.5102223654853,-2.73136171570656));
#29268=CARTESIAN_POINT('Ctrl Pts',(367.87679485592,-11.516046868496,-2.82039329870493));
#29269=CARTESIAN_POINT('Ctrl Pts',(367.960714120322,-11.5218713715067,-2.90584163408582));
#29270=CARTESIAN_POINT('Ctrl Pts',(368.048131624811,-11.5276958745174,-2.98737197225236));
#29271=CARTESIAN_POINT('Ctrl Pts',(368.136776186875,-11.5336021346154,-3.07004673131913));
#29272=CARTESIAN_POINT('Ctrl Pts',(368.229017613753,-11.5395083947134,-3.14869238285008));
#29273=CARTESIAN_POINT('Ctrl Pts',(368.324442591822,-11.5454146548115,-3.22300343968169));
#29274=CARTESIAN_POINT('Ctrl Pts',(368.41986756989,-11.5513209149095,-3.2973144965133));
#29275=CARTESIAN_POINT('Ctrl Pts',(368.518475715946,-11.5572271750076,-3.36729075595378));
#29276=CARTESIAN_POINT('Ctrl Pts',(368.619825966729,-11.5631334351056,-3.43267398461454));
#29277=CARTESIAN_POINT('Ctrl Pts',(368.720023213455,-11.5689725030476,-3.4973133855354));
#29278=CARTESIAN_POINT('Ctrl Pts',(368.823204048632,-11.5748115709897,-3.55765960597024));
#29279=CARTESIAN_POINT('Ctrl Pts',(368.928965788806,-11.5806506389317,-3.61342752945438));
#29280=CARTESIAN_POINT('Ctrl Pts',(369.03459971804,-11.5864826504773,-3.66912805852182));
#29281=CARTESIAN_POINT('Ctrl Pts',(369.14280799164,-11.5923146620229,-3.7202611093649));
#29282=CARTESIAN_POINT('Ctrl Pts',(369.253159372267,-11.5981466735684,-3.76658503927602));
#29283=CARTESIAN_POINT('Ctrl Pts',(369.363405671341,-11.60397313161,-3.81286485745531));
#29284=CARTESIAN_POINT('Ctrl Pts',(369.475790644761,-11.6097995896516,-3.85434451033228));
#29285=CARTESIAN_POINT('Ctrl Pts',(369.589859406784,-11.6156260476932,-3.89082872600213));
#29286=CARTESIAN_POINT('Ctrl Pts',(369.704401000401,-11.6214766572501,-3.92746417404763));
#29287=CARTESIAN_POINT('Ctrl Pts',(369.82064000553,-11.6273272668069,-3.95906248855058));
#29288=CARTESIAN_POINT('Ctrl Pts',(369.938096133759,-11.6331778763638,-3.98547508203966));
#29289=CARTESIAN_POINT('Ctrl Pts',(370.054946738593,-11.6389983241827,-4.01175151027708));
#29290=CARTESIAN_POINT('Ctrl Pts',(370.173001545222,-11.6448187720016,-4.03289547844079));
#29291=CARTESIAN_POINT('Ctrl Pts',(370.291773986964,-11.6506392198205,-4.04881107896914));
#29292=CARTESIAN_POINT('Ctrl Pts',(370.410531534084,-11.656458937728,-4.06472468360656));
#29293=CARTESIAN_POINT('Ctrl Pts',(370.53000613533,-11.6622786556355,-4.07541117107995));
#29294=CARTESIAN_POINT('Ctrl Pts',(370.649703722092,-11.668098373543,-4.08082621813109));
#29295=CARTESIAN_POINT('Ctrl Pts',(370.769414074254,-11.6739187121065,-4.08624184268128));
#29296=CARTESIAN_POINT('Ctrl Pts',(370.889347053994,-11.67973905067,-4.08638489069963));
#29297=CARTESIAN_POINT('Ctrl Pts',(371.00900680281,-11.6855593892335,-4.08126313423826));
#29298=CARTESIAN_POINT('Ctrl Pts',(371.129758272065,-11.6914328298855,-4.07609464922975));
#29299=CARTESIAN_POINT('Ctrl Pts',(371.250231078803,-11.6973062705375,-4.06556481543231));
#29300=CARTESIAN_POINT('Ctrl Pts',(371.369920269737,-11.7031797111895,-4.04973518287613));
#29301=CARTESIAN_POINT('Ctrl Pts',(371.488694308412,-11.709008243087,-4.03402658484183));
#29302=CARTESIAN_POINT('Ctrl Pts',(371.606696280947,-11.7148367749846,-4.01309908232749));
#29303=CARTESIAN_POINT('Ctrl Pts',(371.723443294561,-11.7206653068822,-3.98706420183666));
#29304=CARTESIAN_POINT('Ctrl Pts',(371.841539609265,-11.7265612019114,-3.96072842377636));
#29305=CARTESIAN_POINT('Ctrl Pts',(371.958351360577,-11.7324570969406,-3.92916657745507));
#29306=CARTESIAN_POINT('Ctrl Pts',(372.073395784961,-11.7383529919699,-3.89254555260209));
#29307=CARTESIAN_POINT('Ctrl Pts',(372.188440209345,-11.7442488869991,-3.85592452774911));
#29308=CARTESIAN_POINT('Ctrl Pts',(372.30171692802,-11.7501447820283,-3.81424452269664));
#29309=CARTESIAN_POINT('Ctrl Pts',(372.4127661906,-11.7560406770575,-3.76772157228141));
#29310=CARTESIAN_POINT('Ctrl Pts',(372.522748452178,-11.7618799222202,-3.72164563100016));
#29311=CARTESIAN_POINT('Ctrl Pts',(372.630876980634,-11.7677191673829,-3.67068073444835));
#29312=CARTESIAN_POINT('Ctrl Pts',(372.736688921398,-11.7735584125456,-3.61499783111619));
#29313=CARTESIAN_POINT('Ctrl Pts',(372.842360004958,-11.7793898844859,-3.55938905304787));
#29314=CARTESIAN_POINT('Ctrl Pts',(372.945720282467,-11.7852213564263,-3.49907495555428));
#29315=CARTESIAN_POINT('Ctrl Pts',(373.046326778446,-11.7910528283666,-3.43427452524351));
#29316=CARTESIAN_POINT('Ctrl Pts',(373.140263668869,-11.7964977087924,-3.37376997370112));
#29317=CARTESIAN_POINT('Ctrl Pts',(373.231799722461,-11.8019425892183,-3.30935477406498));
#29318=CARTESIAN_POINT('Ctrl Pts',(373.320592904309,-11.8073874696441,-3.2412437998941));
#29319=CARTESIAN_POINT('Origin',(370.834317853224,-11.,0.));
#29320=CARTESIAN_POINT('',(372.012622422822,-15.1306250182556,3.17836489468462));
#29321=CARTESIAN_POINT('',(372.012622422842,-15.4759533536068,3.17836489467751));
#29322=CARTESIAN_POINT('',(372.012622422842,-11.,3.17836489467752));
#29323=CARTESIAN_POINT('',(367.444571657931,-15.8589799862073,0.00507877902897487));
#29324=CARTESIAN_POINT('Ctrl Pts',(372.012622422842,-15.4759533536068,3.17836489467751));
#29325=CARTESIAN_POINT('Ctrl Pts',(371.915085677486,-15.4820510309549,3.21452436552715));
#29326=CARTESIAN_POINT('Ctrl Pts',(371.815818975043,-15.4881487083029,3.24621370971365));
#29327=CARTESIAN_POINT('Ctrl Pts',(371.715267978533,-15.494246385651,3.27327541450729));
#29328=CARTESIAN_POINT('Ctrl Pts',(371.614748749664,-15.5003421365256,3.30032856954439));
#29329=CARTESIAN_POINT('Ctrl Pts',(371.512946443811,-15.5064378874003,3.32275688102416));
#29330=CARTESIAN_POINT('Ctrl Pts',(371.410321653924,-15.5125336382749,3.34045276632958));
#29331=CARTESIAN_POINT('Ctrl Pts',(371.307703062513,-15.5186290209697,3.358147582814));
#29332=CARTESIAN_POINT('Ctrl Pts',(371.204262505207,-15.5247244036646,3.37111046963088));
#29333=CARTESIAN_POINT('Ctrl Pts',(371.100469655214,-15.5308197863594,3.37928517305025));
#29334=CARTESIAN_POINT('Ctrl Pts',(370.996656552083,-15.5369163584487,3.38746147160269));
#29335=CARTESIAN_POINT('Ctrl Pts',(370.892491443781,-15.543012930538,3.39084769666992));
#29336=CARTESIAN_POINT('Ctrl Pts',(370.788447109625,-15.5491095026272,3.389439619964));
#29337=CARTESIAN_POINT('Ctrl Pts',(370.684294576641,-15.5552124147249,3.38803007895681));
#29338=CARTESIAN_POINT('Ctrl Pts',(370.580263494632,-15.5613153268226,3.38181628746154));
#29339=CARTESIAN_POINT('Ctrl Pts',(370.476824564169,-15.5674182389203,3.3708461268323));
#29340=CARTESIAN_POINT('Ctrl Pts',(370.373326239876,-15.5735246552626,3.35986966722219));
#29341=CARTESIAN_POINT('Ctrl Pts',(370.270421164752,-15.5796310716049,3.34413146283107));
#29342=CARTESIAN_POINT('Ctrl Pts',(370.168570958071,-15.5857374879472,3.32373075535515));
#29343=CARTESIAN_POINT('Ctrl Pts',(370.066565210115,-15.5918532297472,3.30329889279225));
#29344=CARTESIAN_POINT('Ctrl Pts',(369.965617960256,-15.5979689715471,3.2781904104684));
#29345=CARTESIAN_POINT('Ctrl Pts',(369.866176836464,-15.604084713347,3.24855476083871));
#29346=CARTESIAN_POINT('Ctrl Pts',(369.811430946844,-15.6074516475967,3.23223927744915));
#29347=CARTESIAN_POINT('Ctrl Pts',(369.757141228761,-15.6108185818464,3.21455252186698));
#29348=CARTESIAN_POINT('Ctrl Pts',(369.703379629996,-15.6141855160962,3.19552559021866));
#29349=CARTESIAN_POINT('Ctrl Pts',(369.606165004131,-15.6202737884117,3.16112006501042));
#29350=CARTESIAN_POINT('Ctrl Pts',(369.51035770414,-15.6263620607272,3.12221617440523));
#29351=CARTESIAN_POINT('Ctrl Pts',(369.416404507066,-15.6324503330427,3.07894897737639));
#29352=CARTESIAN_POINT('Ctrl Pts',(369.322571621384,-15.6385308090454,3.03573718598441));
#29353=CARTESIAN_POINT('Ctrl Pts',(369.2305885063,-15.644611285048,2.98817337365492));
#29354=CARTESIAN_POINT('Ctrl Pts',(369.140885049192,-15.6506917610507,2.93644179249781));
#29355=CARTESIAN_POINT('Ctrl Pts',(369.051270458902,-15.6567662132882,2.88476146043614));
#29356=CARTESIAN_POINT('Ctrl Pts',(368.963931406737,-15.6628406655257,2.82892178304921));
#29357=CARTESIAN_POINT('Ctrl Pts',(368.879275289204,-15.6689151177632,2.76915395660295));
#29358=CARTESIAN_POINT('Ctrl Pts',(368.794674436653,-15.674985604493,2.70942514763024));
#29359=CARTESIAN_POINT('Ctrl Pts',(368.712753386944,-15.6810560912227,2.64577353530503));
#29360=CARTESIAN_POINT('Ctrl Pts',(368.633891803325,-15.6871265779525,2.57847440581156));
#29361=CARTESIAN_POINT('Ctrl Pts',(368.555056086467,-15.6931950735501,2.51119735057105));
#29362=CARTESIAN_POINT('Ctrl Pts',(368.479278168274,-15.6992635691477,2.4402754346612));
#29363=CARTESIAN_POINT('Ctrl Pts',(368.40690508613,-15.7053320647453,2.36602458158218));
#29364=CARTESIAN_POINT('Ctrl Pts',(368.334536748511,-15.7114001625138,2.29177859612659));
#29365=CARTESIAN_POINT('Ctrl Pts',(368.265573103118,-15.7174682602823,2.21420441559934));
#29366=CARTESIAN_POINT('Ctrl Pts',(368.200324044597,-15.7235363580508,2.13365453591159));
#29367=CARTESIAN_POINT('Ctrl Pts',(368.135062139283,-15.7296056505583,2.05308879687357));
#29368=CARTESIAN_POINT('Ctrl Pts',(368.073516544506,-15.7356749430659,1.96954652887919));
#29369=CARTESIAN_POINT('Ctrl Pts',(368.015956014002,-15.7417442355735,1.883412224055));
#29370=CARTESIAN_POINT('Ctrl Pts',(367.958333931101,-15.7478200182837,1.79718581144496));
#29371=CARTESIAN_POINT('Ctrl Pts',(367.904705659556,-15.7538958009939,1.70836218635213));
#29372=CARTESIAN_POINT('Ctrl Pts',(367.855295787055,-15.7599715837041,1.61735357661238));
#29373=CARTESIAN_POINT('Ctrl Pts',(367.805856909444,-15.7660509330852,1.52629154202677));
#29374=CARTESIAN_POINT('Ctrl Pts',(367.760641549194,-15.7721302824663,1.43304235549025));
#29375=CARTESIAN_POINT('Ctrl Pts',(367.719826751698,-15.7782096318473,1.33803970083583));
#29376=CARTESIAN_POINT('Ctrl Pts',(367.678947355797,-15.7842986031374,1.24288668356181));
#29377=CARTESIAN_POINT('Ctrl Pts',(367.642482581195,-15.7903875744275,1.14597505873585));
#29378=CARTESIAN_POINT('Ctrl Pts',(367.610560106106,-15.7964765457175,1.04775524355367));
#29379=CARTESIAN_POINT('Ctrl Pts',(367.592007668837,-15.800015283161,0.990672672274866));
#29380=CARTESIAN_POINT('Ctrl Pts',(367.574988493561,-15.8035540206046,0.933148487401219));
#29381=CARTESIAN_POINT('Ctrl Pts',(367.559519679585,-15.8070927580481,0.875272520092086));
#29382=CARTESIAN_POINT('Ctrl Pts',(367.524528649451,-15.8150975132095,0.744354938486314));
#29383=CARTESIAN_POINT('Ctrl Pts',(367.497384183701,-15.823102268371,0.611307366002712));
#29384=CARTESIAN_POINT('Ctrl Pts',(367.478289125932,-15.8311070235325,0.476944697096577));
#29385=CARTESIAN_POINT('Ctrl Pts',(367.45956976824,-15.8389542831173,0.345225647588131));
#29386=CARTESIAN_POINT('Ctrl Pts',(367.44858613634,-15.8468015427021,0.212242435105983));
#29387=CARTESIAN_POINT('Ctrl Pts',(367.445483495871,-15.8546488022869,0.0787829989611029));
#29388=CARTESIAN_POINT('Ctrl Pts',(367.444912676366,-15.8560925302603,0.0542293163407381));
#29389=CARTESIAN_POINT('Ctrl Pts',(367.444608486778,-15.8575362582338,0.0296595777462121));
#29390=CARTESIAN_POINT('Ctrl Pts',(367.444571657931,-15.8589799862073,0.00507877902897487));
#29391=CARTESIAN_POINT('',(368.26108342621,-16.,-2.20655152809223));
#29392=CARTESIAN_POINT('Ctrl Pts',(367.444571791084,-15.8604132225308,0.00516688582735295));
#29393=CARTESIAN_POINT('Ctrl Pts',(367.444368925066,-15.8689596753995,-0.127923782203768));
#29394=CARTESIAN_POINT('Ctrl Pts',(367.452004419869,-15.8774239806517,-0.260919577064219));
#29395=CARTESIAN_POINT('Ctrl Pts',(367.479606817387,-15.8922327881285,-0.497313792977768));
#29396=CARTESIAN_POINT('Ctrl Pts',(367.496601528192,-15.8986398126175,-0.60088279544555));
#29397=CARTESIAN_POINT('Ctrl Pts',(367.533806436283,-15.9093613893647,-0.776246727587198));
#29398=CARTESIAN_POINT('Ctrl Pts',(367.551629335393,-15.9137397185277,-0.848464409357345));
#29399=CARTESIAN_POINT('Ctrl Pts',(367.595944192492,-15.9232110648643,-1.00560666487732));
#29400=CARTESIAN_POINT('Ctrl Pts',(367.623431929418,-15.9282724154365,-1.09019356338717));
#29401=CARTESIAN_POINT('Ctrl Pts',(367.690219426018,-15.9390944475785,-1.27116653976022));
#29402=CARTESIAN_POINT('Ctrl Pts',(367.730695232446,-15.9448218038598,-1.36702142877395));
#29403=CARTESIAN_POINT('Ctrl Pts',(367.877191286025,-15.9633925603866,-1.6737587249561));
#29404=CARTESIAN_POINT('Ctrl Pts',(368.000806589721,-15.9759676173899,-1.87543678879479));
#29405=CARTESIAN_POINT('Ctrl Pts',(368.165052549216,-15.9912516825638,-2.08963778707627));
#29406=CARTESIAN_POINT('Ctrl Pts',(368.186166578252,-15.993194783547,-2.11633126665893));
#29407=CARTESIAN_POINT('Ctrl Pts',(368.225218517582,-15.9967580887144,-2.16420324926291));
#29408=CARTESIAN_POINT('Ctrl Pts',(368.243021585248,-15.9983715362902,-2.18548818541282));
#29409=CARTESIAN_POINT('Ctrl Pts',(368.261083426209,-16.0000000000003,-2.2065515280925));
#29410=CARTESIAN_POINT('',(373.376670596656,-16.,-2.24206324408181));
#29411=CARTESIAN_POINT('Origin',(370.834317853224,-16.,0.));
#29412=CARTESIAN_POINT('Ctrl Pts',(373.376670596656,-16.,-2.24206324408178));
#29413=CARTESIAN_POINT('Ctrl Pts',(373.181129850895,-15.9815073064942,-2.46379363137158));
#29414=CARTESIAN_POINT('Ctrl Pts',(372.957360744741,-15.9621520677859,-2.65906379107586));
#29415=CARTESIAN_POINT('Ctrl Pts',(372.624823145168,-15.9373252245759,-2.88013923328604));
#29416=CARTESIAN_POINT('Ctrl Pts',(372.536073584592,-15.9310067923377,-2.93345220247366));
#29417=CARTESIAN_POINT('Ctrl Pts',(372.382793677882,-15.9205976093272,-3.01622752956713));
#29418=CARTESIAN_POINT('Ctrl Pts',(372.319531307382,-15.9164369440155,-3.04787597287237));
#29419=CARTESIAN_POINT('Ctrl Pts',(372.181961182041,-15.9076570415518,-3.11139705929018));
#29420=CARTESIAN_POINT('Ctrl Pts',(372.107409577823,-15.903060053103,-3.14263791780728));
#29421=CARTESIAN_POINT('Ctrl Pts',(371.829792649048,-15.8864392827796,-3.24747049345628));
#29422=CARTESIAN_POINT('Ctrl Pts',(371.620948274416,-15.8749254565236,-3.3042783361045));
#29423=CARTESIAN_POINT('Ctrl Pts',(371.294039411643,-15.8571425492,-3.36042503244688));
#29424=CARTESIAN_POINT('Ctrl Pts',(371.1790482447,-15.8509221310753,-3.3741604633309));
#29425=CARTESIAN_POINT('Ctrl Pts',(370.987595630786,-15.8403343195617,-3.38713921303782));
#29426=CARTESIAN_POINT('Ctrl Pts',(370.911458383628,-15.836062878099,-3.38972769808728));
#29427=CARTESIAN_POINT('Ctrl Pts',(370.793483966147,-15.8292657561943,-3.38976202483508));
#29428=CARTESIAN_POINT('Ctrl Pts',(370.751668630722,-15.8268212488625,-3.38900029485282));
#29429=CARTESIAN_POINT('Ctrl Pts',(370.659661419984,-15.8213480916324,-3.38562036872409));
#29430=CARTESIAN_POINT('Ctrl Pts',(370.60949513568,-15.8183049363756,-3.38265935375856));
#29431=CARTESIAN_POINT('Ctrl Pts',(370.308538621423,-15.7997639362016,-3.35817175643423));
#29432=CARTESIAN_POINT('Ctrl Pts',(370.060724557639,-15.7833721310607,-3.30988069002626));
#29433=CARTESIAN_POINT('Ctrl Pts',(369.671815573573,-15.7574845746523,-3.18799112169855));
#29434=CARTESIAN_POINT('Ctrl Pts',(369.526463382616,-15.7477541465874,-3.13116995294513));
#29435=CARTESIAN_POINT('Ctrl Pts',(369.317224026491,-15.7337521781211,-3.03224980723153));
#29436=CARTESIAN_POINT('Ctrl Pts',(369.250019055329,-15.7292534396165,-2.99768430518787));
#29437=CARTESIAN_POINT('Ctrl Pts',(369.120795446843,-15.7205873274601,-2.92565981991112));
#29438=CARTESIAN_POINT('Ctrl Pts',(369.058711579588,-15.7164161902242,-2.88840230383671));
#29439=CARTESIAN_POINT('Ctrl Pts',(368.895611415357,-15.7054018723884,-2.78327541581863));
#29440=CARTESIAN_POINT('Ctrl Pts',(368.796974851988,-15.6986831471059,-2.71190744469673));
#29441=CARTESIAN_POINT('Ctrl Pts',(368.512214597918,-15.6787819523762,-2.48154622506456));
#29442=CARTESIAN_POINT('Ctrl Pts',(368.339269910257,-15.6660283890105,-2.30758724485276));
#29443=CARTESIAN_POINT('Ctrl Pts',(368.136792464523,-15.6481987742494,-2.05429158960542));
#29444=CARTESIAN_POINT('Ctrl Pts',(368.089242598258,-15.6437435333288,-1.99030580620531));
#29445=CARTESIAN_POINT('Ctrl Pts',(368.020127289003,-15.6367444247644,-1.89010674556755));
#29446=CARTESIAN_POINT('Ctrl Pts',(367.996905841995,-15.6342923527546,-1.85506468777503));
#29447=CARTESIAN_POINT('Ctrl Pts',(367.948509069746,-15.6289422105522,-1.77899655050264));
#29448=CARTESIAN_POINT('Ctrl Pts',(367.923544980871,-15.626034023493,-1.73784976699607));
#29449=CARTESIAN_POINT('Ctrl Pts',(367.788875678473,-15.6095448407672,-1.50483647351955));
#29450=CARTESIAN_POINT('Ctrl Pts',(367.697269890652,-15.5952341464205,-1.30313907047644));
#29451=CARTESIAN_POINT('Ctrl Pts',(367.585313285836,-15.5730710283633,-0.974796926929378));
#29452=CARTESIAN_POINT('Ctrl Pts',(367.551346176506,-15.5650970921987,-0.853440525345097));
#29453=CARTESIAN_POINT('Ctrl Pts',(367.502936543691,-15.5511694015422,-0.634072694639167));
#29454=CARTESIAN_POINT('Ctrl Pts',(367.485883754585,-15.5451568403413,-0.536788145642456));
#29455=CARTESIAN_POINT('Ctrl Pts',(367.464094627573,-15.5351197794893,-0.36991737839074));
#29456=CARTESIAN_POINT('Ctrl Pts',(367.457213189075,-15.5310346384404,-0.300680169648971));
#29457=CARTESIAN_POINT('Ctrl Pts',(367.44694727203,-15.5223316747026,-0.150566255261707));
#29458=CARTESIAN_POINT('Ctrl Pts',(367.444318485203,-15.5177385953621,-0.0696805304459789));
#29459=CARTESIAN_POINT('Ctrl Pts',(367.445415315348,-15.4992324152054,0.261494802441862));
#29460=CARTESIAN_POINT('Ctrl Pts',(367.473956208093,-15.4860609706456,0.510897509708436));
#29461=CARTESIAN_POINT('Ctrl Pts',(367.561438832565,-15.4650019222951,0.893860808524713));
#29462=CARTESIAN_POINT('Ctrl Pts',(367.601914910565,-15.4572839725652,1.03067359573983));
#29463=CARTESIAN_POINT('Ctrl Pts',(367.667227884636,-15.4464920090718,1.20921946241856));
#29464=CARTESIAN_POINT('Ctrl Pts',(367.684518334353,-15.4437495089187,1.25356813036079));
#29465=CARTESIAN_POINT('Ctrl Pts',(367.718818462732,-15.4384872562773,1.33635096595479));
#29466=CARTESIAN_POINT('Ctrl Pts',(367.735619858271,-15.4359779786288,1.37486015810798));
#29467=CARTESIAN_POINT('Ctrl Pts',(367.785713281397,-15.4287013156099,1.48409043161024));
#29468=CARTESIAN_POINT('Ctrl Pts',(367.82074077183,-15.4238521825269,1.55398381326585));
#29469=CARTESIAN_POINT('Ctrl Pts',(367.955245838918,-15.4061800543025,1.80069278290662));
#29470=CARTESIAN_POINT('Ctrl Pts',(368.068130614859,-15.3930403856624,1.96971054294453));
#29471=CARTESIAN_POINT('Ctrl Pts',(368.290250308091,-15.3705880698647,2.245203272554));
#29472=CARTESIAN_POINT('Ctrl Pts',(368.3928117271,-15.3611728460088,2.35632640979305));
#29473=CARTESIAN_POINT('Ctrl Pts',(368.556872201341,-15.347506755999,2.51182560962108));
#29474=CARTESIAN_POINT('Ctrl Pts',(368.612988702248,-15.3430449324642,2.56158635832513));
#29475=CARTESIAN_POINT('Ctrl Pts',(368.726365910705,-15.3344226245516,2.65559225676189));
#29476=CARTESIAN_POINT('Ctrl Pts',(368.783483518159,-15.3302592822766,2.69994652608585));
#29477=CARTESIAN_POINT('Ctrl Pts',(368.941226536833,-15.319199642174,2.81454419418131));
#29478=CARTESIAN_POINT('Ctrl Pts',(369.044319700471,-15.3124315283819,2.88120881749646));
#29479=CARTESIAN_POINT('Ctrl Pts',(369.361922022979,-15.2925699548962,3.06294263369627));
#29480=CARTESIAN_POINT('Ctrl Pts',(369.585409599288,-15.2798939253938,3.16066181787488));
#29481=CARTESIAN_POINT('Ctrl Pts',(369.893163928145,-15.2621618525088,3.25744373128031));
#29482=CARTESIAN_POINT('Ctrl Pts',(369.969720993533,-15.2577242499199,3.27859434104151));
#29483=CARTESIAN_POINT('Ctrl Pts',(370.087724318164,-15.2507499141775,3.30677501825687));
#29484=CARTESIAN_POINT('Ctrl Pts',(370.128680391649,-15.2483045801731,3.31575611149422));
#29485=CARTESIAN_POINT('Ctrl Pts',(370.217159029718,-15.2429513328119,3.33344466156055));
#29486=CARTESIAN_POINT('Ctrl Pts',(370.264719933196,-15.2400329123458,3.34190005784656));
#29487=CARTESIAN_POINT('Ctrl Pts',(370.440641079645,-15.2291267817304,3.36931114247035));
#29488=CARTESIAN_POINT('Ctrl Pts',(370.569871638207,-15.2209017652042,3.38190805200113));
#29489=CARTESIAN_POINT('Ctrl Pts',(370.878679489492,-15.201155567086,3.39420021505435));
#29490=CARTESIAN_POINT('Ctrl Pts',(371.058159037159,-15.1896181542278,3.38710274522967));
#29491=CARTESIAN_POINT('Ctrl Pts',(371.354384885678,-15.1709103792875,3.35172981177866));
#29492=CARTESIAN_POINT('Ctrl Pts',(371.471714152433,-15.1635847541056,3.33141007565144));
#29493=CARTESIAN_POINT('Ctrl Pts',(371.657823241952,-15.1521187011189,3.28898321264146));
#29494=CARTESIAN_POINT('Ctrl Pts',(371.727382122338,-15.147867585696,3.27078110476225));
#29495=CARTESIAN_POINT('Ctrl Pts',(371.868732958214,-15.1392852872532,3.2289463313005));
#29496=CARTESIAN_POINT('Ctrl Pts',(371.940419163311,-15.1349634594056,3.20509752148028));
#29497=CARTESIAN_POINT('Ctrl Pts',(372.011709388664,-15.1306798775974,3.17870326891439));
#29498=CARTESIAN_POINT('Ctrl Pts',(372.012165924805,-15.1306524464985,3.17853413066531));
#29499=CARTESIAN_POINT('Ctrl Pts',(372.012622422822,-15.1306250182556,3.1783648946846));
#29500=CARTESIAN_POINT('Origin',(370.834317853224,-11.,0.));
#29501=CARTESIAN_POINT('',(372.012622418493,-13.8856567889318,3.1783648962896));
#29502=CARTESIAN_POINT('',(372.012622422842,-14.2257519494217,3.17836489467751));
#29503=CARTESIAN_POINT('',(372.012622422842,-11.,3.17836489467752));
#29504=CARTESIAN_POINT('',(367.444568873987,-14.6089821967165,-0.00263063910416286));
#29505=CARTESIAN_POINT('Ctrl Pts',(372.012622422842,-14.2257519494217,3.17836489467751));
#29506=CARTESIAN_POINT('Ctrl Pts',(371.91124658596,-14.2320990949235,3.21594761906723));
#29507=CARTESIAN_POINT('Ctrl Pts',(371.808171373033,-14.2384462404253,3.24863824573331));
#29508=CARTESIAN_POINT('Ctrl Pts',(371.703910693242,-14.2447933859271,3.27631093687543));
#29509=CARTESIAN_POINT('Ctrl Pts',(371.599650013451,-14.2511405314289,3.30398362801756));
#29510=CARTESIAN_POINT('Ctrl Pts',(371.494204378047,-14.2574876769308,3.32663833846832));
#29511=CARTESIAN_POINT('Ctrl Pts',(371.388095647466,-14.2638348224326,3.34420920653966));
#29512=CARTESIAN_POINT('Ctrl Pts',(371.285822638614,-14.2699525251375,3.3611449057602));
#29513=CARTESIAN_POINT('Ctrl Pts',(371.182610429071,-14.2760702278424,3.3734115222908));
#29514=CARTESIAN_POINT('Ctrl Pts',(371.078920131339,-14.2821879305474,3.38091330679169));
#29515=CARTESIAN_POINT('Ctrl Pts',(370.975360398977,-14.2882979299267,3.38840564515063));
#29516=CARTESIAN_POINT('Ctrl Pts',(370.871324196144,-14.2944079293061,3.39114505110587));
#29517=CARTESIAN_POINT('Ctrl Pts',(370.767281275843,-14.3005179286855,3.38908706878312));
#29518=CARTESIAN_POINT('Ctrl Pts',(370.663340093026,-14.3066219534539,3.3870310988409));
#29519=CARTESIAN_POINT('Ctrl Pts',(370.559392628715,-14.3127259782223,3.38018707898977));
#29520=CARTESIAN_POINT('Ctrl Pts',(370.45591134727,-14.3188300029908,3.36856253894029));
#29521=CARTESIAN_POINT('Ctrl Pts',(370.352498257132,-14.3249300053755,3.35694565914164));
#29522=CARTESIAN_POINT('Ctrl Pts',(370.249551160134,-14.3310300077602,3.34055457182891));
#29523=CARTESIAN_POINT('Ctrl Pts',(370.147539315721,-14.3371300101448,3.31944879504494));
#29524=CARTESIAN_POINT('Ctrl Pts',(370.04556157806,-14.343227973048,3.29835007478964));
#29525=CARTESIAN_POINT('Ctrl Pts',(369.944518887154,-14.3493259359512,3.27253988471554));
#29526=CARTESIAN_POINT('Ctrl Pts',(369.844871427421,-14.3554238988543,3.24212905865364));
#29527=CARTESIAN_POINT('Ctrl Pts',(369.745231894195,-14.361521376692,3.21172065163599));
#29528=CARTESIAN_POINT('Ctrl Pts',(369.64698777777,-14.3676188545297,3.17671246085942));
#29529=CARTESIAN_POINT('Ctrl Pts',(369.550584338613,-14.3737163323674,3.13726526228891));
#29530=CARTESIAN_POINT('Ctrl Pts',(369.454164005467,-14.3798148787429,3.09781115088893));
#29531=CARTESIAN_POINT('Ctrl Pts',(369.359585383833,-14.3859134251184,3.05391664693505));
#29532=CARTESIAN_POINT('Ctrl Pts',(369.267273164675,-14.392011971494,3.00579041295133));
#29533=CARTESIAN_POINT('Ctrl Pts',(369.174868353328,-14.3981166349119,2.95761590677372));
#29534=CARTESIAN_POINT('Ctrl Pts',(369.084734860711,-14.4042212983298,2.90520139258086));
#29535=CARTESIAN_POINT('Ctrl Pts',(368.997272123444,-14.4103259617477,2.84880115999623));
#29536=CARTESIAN_POINT('Ctrl Pts',(368.909760749328,-14.4164340198866,2.79236956400288));
#29537=CARTESIAN_POINT('Ctrl Pts',(368.824923435153,-14.4225420780255,2.73194808084853));
#29538=CARTESIAN_POINT('Ctrl Pts',(368.743128469909,-14.4286501361644,2.66783283314581));
#29539=CARTESIAN_POINT('Ctrl Pts',(368.661211980528,-14.4347672691466,2.60362232835576));
#29540=CARTESIAN_POINT('Ctrl Pts',(368.582347188466,-14.4408844021289,2.53570737689277));
#29541=CARTESIAN_POINT('Ctrl Pts',(368.506867344009,-14.4470015351111,2.46442268891778));
#29542=CARTESIAN_POINT('Ctrl Pts',(368.466804260173,-14.4502483782022,2.42658630423728));
#29543=CARTESIAN_POINT('Ctrl Pts',(368.427694157088,-14.4534952212934,2.38780117871283));
#29544=CARTESIAN_POINT('Ctrl Pts',(368.389582259366,-14.4567420643846,2.34812115075559));
#29545=CARTESIAN_POINT('Ctrl Pts',(368.315123261944,-14.4630854032317,2.27059850622654));
#29546=CARTESIAN_POINT('Ctrl Pts',(368.244214620814,-14.4694287420789,2.1893839797476));
#29547=CARTESIAN_POINT('Ctrl Pts',(368.177245026862,-14.4757720809261,2.10484418851099));
#29548=CARTESIAN_POINT('Ctrl Pts',(368.113616044009,-14.481798998142,2.02452145382602));
#29549=CARTESIAN_POINT('Ctrl Pts',(368.053542963847,-14.487825915358,1.94119757354517));
#29550=CARTESIAN_POINT('Ctrl Pts',(367.997322392813,-14.493852832574,1.85522554426817));
#29551=CARTESIAN_POINT('Ctrl Pts',(367.941149535837,-14.4998746347817,1.76932647893339));
#29552=CARTESIAN_POINT('Ctrl Pts',(367.888822931825,-14.5058964369894,1.68078409341299));
#29553=CARTESIAN_POINT('Ctrl Pts',(367.840598028115,-14.5119182391971,1.5899832298651));
#29554=CARTESIAN_POINT('Ctrl Pts',(367.792400881935,-14.517936575346,1.49923462992842));
#29555=CARTESIAN_POINT('Ctrl Pts',(367.748300949639,-14.523954911495,1.40623052089193));
#29556=CARTESIAN_POINT('Ctrl Pts',(367.708509001295,-14.5299732476439,1.31138250853956));
#29557=CARTESIAN_POINT('Ctrl Pts',(367.668729090899,-14.5359897631126,1.2165631898157));
#29558=CARTESIAN_POINT('Ctrl Pts',(367.633254741903,-14.5420062785813,1.11990148061017));
#29559=CARTESIAN_POINT('Ctrl Pts',(367.602249173642,-14.54802279405,1.02183027600718));
#29560=CARTESIAN_POINT('Ctrl Pts',(367.571234157724,-14.5540411428015,0.923729188283593));
#29561=CARTESIAN_POINT('Ctrl Pts',(367.544690779183,-14.5600594915531,0.824218163703193));
#29562=CARTESIAN_POINT('Ctrl Pts',(367.522732626955,-14.5660778403046,0.723746054672887));
#29563=CARTESIAN_POINT('Ctrl Pts',(367.500770556816,-14.5720972628875,0.623256018781771));
#29564=CARTESIAN_POINT('Ctrl Pts',(367.483395422998,-14.5781166854704,0.521804987559546));
#29565=CARTESIAN_POINT('Ctrl Pts',(367.470669535808,-14.5841361080533,0.419851234659084));
#29566=CARTESIAN_POINT('Ctrl Pts',(367.457932447937,-14.5901608286269,0.317807747233233));
#29567=CARTESIAN_POINT('Ctrl Pts',(367.449852814453,-14.5961855492004,0.215261091024579));
#29568=CARTESIAN_POINT('Ctrl Pts',(367.446440971499,-14.6022102697739,0.112673407565595));
#29569=CARTESIAN_POINT('Ctrl Pts',(367.445162641052,-14.6044675787548,0.0742364217549553));
#29570=CARTESIAN_POINT('Ctrl Pts',(367.444539054526,-14.6067248877357,0.0357936694278519));
#29571=CARTESIAN_POINT('Ctrl Pts',(367.444568873987,-14.6089821967165,-0.00263063910417031));
#29572=CARTESIAN_POINT('Ctrl Pts',(367.444568873987,-14.6089821967504,-0.00263063968060246));
#29573=CARTESIAN_POINT('Ctrl Pts',(367.444678491567,-14.6172801566126,-0.143879964709788));
#29574=CARTESIAN_POINT('Ctrl Pts',(367.453620519671,-14.6255781164748,-0.284780872301649));
#29575=CARTESIAN_POINT('Ctrl Pts',(367.471242920486,-14.633876076337,-0.424419673543423));
#29576=CARTESIAN_POINT('Ctrl Pts',(367.482408804865,-14.6391338196701,-0.512897442594087));
#29577=CARTESIAN_POINT('Ctrl Pts',(367.497058665012,-14.6443915630033,-0.600869113347477));
#29578=CARTESIAN_POINT('Ctrl Pts',(367.515144168952,-14.6496493063364,-0.688106907490654));
#29579=CARTESIAN_POINT('Ctrl Pts',(367.536190000969,-14.6557676640746,-0.789624231375929));
#29580=CARTESIAN_POINT('Ctrl Pts',(367.56193066331,-14.6618860218127,-0.890335427005092));
#29581=CARTESIAN_POINT('Ctrl Pts',(367.592289324518,-14.6680043795509,-0.989775773373781));
#29582=CARTESIAN_POINT('Ctrl Pts',(367.622609746661,-14.6741150307476,-1.08909086698887));
#29583=CARTESIAN_POINT('Ctrl Pts',(367.657536478472,-14.6802256819443,-1.18713789094678));
#29584=CARTESIAN_POINT('Ctrl Pts',(367.69694172691,-14.686336333141,-1.28346254504481));
#29585=CARTESIAN_POINT('Ctrl Pts',(367.736308420847,-14.6924410056138,-1.37969295411159));
#29586=CARTESIAN_POINT('Ctrl Pts',(367.780144756326,-14.6985456780865,-1.47420395355472));
#29587=CARTESIAN_POINT('Ctrl Pts',(367.828273468945,-14.7046503505593,-1.56655744300817));
#29588=CARTESIAN_POINT('Ctrl Pts',(367.876370399687,-14.7107509918013,-1.65884994667818));
#29589=CARTESIAN_POINT('Ctrl Pts',(367.928753874277,-14.7168516330433,-1.7489873981159));
#29590=CARTESIAN_POINT('Ctrl Pts',(367.98519928576,-14.7229522742852,-1.83655341633011));
#29591=CARTESIAN_POINT('Ctrl Pts',(368.041625773511,-14.729050870243,-1.92409007740244));
#29592=CARTESIAN_POINT('Ctrl Pts',(368.102111260977,-14.7351494662008,-2.00905666226684));
#29593=CARTESIAN_POINT('Ctrl Pts',(368.166386539706,-14.7412480621586,-2.09106374098151));
#29594=CARTESIAN_POINT('Ctrl Pts',(368.230656636426,-14.7473461664348,-2.17306420811305));
#29595=CARTESIAN_POINT('Ctrl Pts',(368.298715654354,-14.753444270711,-2.25210530946646));
#29596=CARTESIAN_POINT('Ctrl Pts',(368.370253171042,-14.7595423749871,-2.32782952651722));
#29597=CARTESIAN_POINT('Ctrl Pts',(368.441803135644,-14.7656415403663,-2.40356691998958));
#29598=CARTESIAN_POINT('Ctrl Pts',(368.516832509931,-14.7717407057454,-2.47598597351562));
#29599=CARTESIAN_POINT('Ctrl Pts',(368.594993607598,-14.7778398711246,-2.54476560520858));
#29600=CARTESIAN_POINT('Ctrl Pts',(368.673232903487,-14.783945138566,-2.61361404920098));
#29601=CARTESIAN_POINT('Ctrl Pts',(368.75460985913,-14.7900504060074,-2.6788155202828));
#29602=CARTESIAN_POINT('Ctrl Pts',(368.838743319677,-14.7961556734488,-2.74008892986352));
#29603=CARTESIAN_POINT('Ctrl Pts',(368.922923454412,-14.8022643278708,-2.80139633170603));
#29604=CARTESIAN_POINT('Ctrl Pts',(369.009862785874,-14.8083729822929,-2.85877109705749));
#29605=CARTESIAN_POINT('Ctrl Pts',(369.099152350093,-14.8144816367149,-2.91197626007593));
#29606=CARTESIAN_POINT('Ctrl Pts',(369.188574303088,-14.8205993483798,-2.96526030987622));
#29607=CARTESIAN_POINT('Ctrl Pts',(369.280353073307,-14.8267170600448,-3.01436221111961));
#29608=CARTESIAN_POINT('Ctrl Pts',(369.374056317144,-14.8328347717098,-3.05909158227477));
#29609=CARTESIAN_POINT('Ctrl Pts',(369.423691543035,-14.8360753639027,-3.08278502500238));
#29610=CARTESIAN_POINT('Ctrl Pts',(369.473866428129,-14.8393159560956,-3.10525240129708));
#29611=CARTESIAN_POINT('Ctrl Pts',(369.524514850808,-14.8425565482884,-3.12647103894502));
#29612=CARTESIAN_POINT('Ctrl Pts',(369.620132428815,-14.8486743612509,-3.16652904338437));
#29613=CARTESIAN_POINT('Ctrl Pts',(369.71774026339,-14.8547921742134,-3.20225986171064));
#29614=CARTESIAN_POINT('Ctrl Pts',(369.816911691517,-14.8609099871759,-3.23346405030593));
#29615=CARTESIAN_POINT('Ctrl Pts',(369.915958346431,-14.86702010297,-3.26462897913713));
#29616=CARTESIAN_POINT('Ctrl Pts',(370.016564280881,-14.8731302187641,-3.29127847606453));
#29617=CARTESIAN_POINT('Ctrl Pts',(370.118282604491,-14.8792403345582,-3.31326101976171));
#29618=CARTESIAN_POINT('Ctrl Pts',(370.219901562857,-14.8853444815835,-3.33522208944361));
#29619=CARTESIAN_POINT('Ctrl Pts',(370.322630335728,-14.8914486286089,-3.35252518385291));
#29620=CARTESIAN_POINT('Ctrl Pts',(370.426007415101,-14.8975527756342,-3.36506874352068));
#29621=CARTESIAN_POINT('Ctrl Pts',(370.52931650728,-14.9036529081931,-3.37760405376389));
#29622=CARTESIAN_POINT('Ctrl Pts',(370.633272637189,-14.9097530407519,-3.38538600365403));
#29623=CARTESIAN_POINT('Ctrl Pts',(370.737405434675,-14.9158531733107,-3.38836436140374));
#29624=CARTESIAN_POINT('Ctrl Pts',(370.841503498906,-14.9219512711843,-3.39134172572908));
#29625=CARTESIAN_POINT('Ctrl Pts',(370.945777689179,-14.928049369058,-3.38951867092157));
#29626=CARTESIAN_POINT('Ctrl Pts',(371.049754640543,-14.9341474669317,-3.38289699121475));
#29627=CARTESIAN_POINT('Ctrl Pts',(371.153723398455,-14.9402450842712,-3.3762758333006));
#29628=CARTESIAN_POINT('Ctrl Pts',(371.257394539983,-14.9463427016108,-3.36485682990787));
#29629=CARTESIAN_POINT('Ctrl Pts',(371.360297713031,-14.9524403189504,-3.3486938124554));
#29630=CARTESIAN_POINT('Ctrl Pts',(371.463218990748,-14.9585390090979,-3.33252795129991));
#29631=CARTESIAN_POINT('Ctrl Pts',(371.565371611726,-14.9646376992453,-3.31161648354425));
#29632=CARTESIAN_POINT('Ctrl Pts',(371.666294203627,-14.9707363893928,-3.2860645786214));
#29633=CARTESIAN_POINT('Ctrl Pts',(371.767318111185,-14.9768412019831,-3.26048702227629));
#29634=CARTESIAN_POINT('Ctrl Pts',(371.867109111646,-14.9829460145734,-3.23025983199035));
#29635=CARTESIAN_POINT('Ctrl Pts',(371.965219891154,-14.9890508271636,-3.19553839643754));
#29636=CARTESIAN_POINT('Ctrl Pts',(372.063385279427,-14.9951590377116,-3.16079763482564));
#29637=CARTESIAN_POINT('Ctrl Pts',(372.159868190242,-15.0012672482596,-3.12155780481548));
#29638=CARTESIAN_POINT('Ctrl Pts',(372.254241977364,-15.0073754588075,-3.07802218058713));
#29639=CARTESIAN_POINT('Ctrl Pts',(372.348756026856,-15.01349274764,-3.03442185184674));
#29640=CARTESIAN_POINT('Ctrl Pts',(372.441154315709,-15.0196100364725,-2.98651317438402));
#29641=CARTESIAN_POINT('Ctrl Pts',(372.531035399137,-15.0257273253049,-2.93454504683261));
#29642=CARTESIAN_POINT('Ctrl Pts',(372.578721230837,-15.0289728136167,-2.9069736904403));
#29643=CARTESIAN_POINT('Ctrl Pts',(372.625699018816,-15.0322183019285,-2.87826042788618));
#29644=CARTESIAN_POINT('Ctrl Pts',(372.671912418313,-15.0354637902403,-2.84844716939898));
#29645=CARTESIAN_POINT('Ctrl Pts',(372.758966103217,-15.0415774222159,-2.7922869639474));
#29646=CARTESIAN_POINT('Ctrl Pts',(372.843581656635,-15.0476910541914,-2.73204285312905));
#29647=CARTESIAN_POINT('Ctrl Pts',(372.925353574086,-15.0538046861669,-2.66795327481173));
#29648=CARTESIAN_POINT('Ctrl Pts',(373.007022294952,-15.0599106027072,-2.60394457787502));
#29649=CARTESIAN_POINT('Ctrl Pts',(373.085854182912,-15.0660165192474,-2.5361003234214));
#29650=CARTESIAN_POINT('Ctrl Pts',(373.161471772641,-15.0721224357876,-2.46470276054571));
#29651=CARTESIAN_POINT('Ctrl Pts',(373.23701529353,-15.0782223714686,-2.39337513291565));
#29652=CARTESIAN_POINT('Ctrl Pts',(373.309350469883,-15.0843223071496,-2.31850140982599));
#29653=CARTESIAN_POINT('Ctrl Pts',(373.378132740677,-15.0904222428306,-2.24040417801623));
#29654=CARTESIAN_POINT('Ctrl Pts',(373.446869744383,-15.0965181640131,-2.16235834366976));
#29655=CARTESIAN_POINT('Ctrl Pts',(373.512058212156,-15.1026140851956,-2.0810935382982));
#29656=CARTESIAN_POINT('Ctrl Pts',(373.573390877461,-15.1087100063781,-1.9969687104201));
#29657=CARTESIAN_POINT('Ctrl Pts',(373.634703092097,-15.114803894946,-1.91287193299475));
#29658=CARTESIAN_POINT('Ctrl Pts',(373.692161809484,-15.120897783514,-1.82591737239204));
#29659=CARTESIAN_POINT('Ctrl Pts',(373.745500961033,-15.1269916720819,-1.73649588980455));
#29660=CARTESIAN_POINT('Ctrl Pts',(373.798835972629,-15.1330850876688,-1.64708134772249));
#29661=CARTESIAN_POINT('Ctrl Pts',(373.848051836545,-15.1391785032557,-1.55520063016936));
#29662=CARTESIAN_POINT('Ctrl Pts',(373.892927096109,-15.1452719188426,-1.4612715565008));
#29663=CARTESIAN_POINT('Ctrl Pts',(373.937810352466,-15.1513664202791,-1.36732574462576));
#29664=CARTESIAN_POINT('Ctrl Pts',(373.978351284079,-15.1574609217156,-1.27133123539307));
#29665=CARTESIAN_POINT('Ctrl Pts',(374.014375849501,-15.1635554231521,-1.17372748234632));
#29666=CARTESIAN_POINT('Ctrl Pts',(374.050436870469,-15.1696560920019,-1.07602495786037));
#29667=CARTESIAN_POINT('Ctrl Pts',(374.081972252425,-15.1757567608516,-0.976710338023476));
#29668=CARTESIAN_POINT('Ctrl Pts',(374.108857320693,-15.1818574297013,-0.87623988638124));
#29669=CARTESIAN_POINT('Ctrl Pts',(374.135757452608,-15.1879615167426,-0.775713141362782));
#29670=CARTESIAN_POINT('Ctrl Pts',(374.158001989767,-15.1940656037839,-0.674029690166241));
#29671=CARTESIAN_POINT('Ctrl Pts',(374.175517441013,-15.2001696908251,-0.571655820453991));
#29672=CARTESIAN_POINT('Ctrl Pts',(374.193059143276,-15.2062829262743,-0.469128519457345));
#29673=CARTESIAN_POINT('Ctrl Pts',(374.205857553494,-15.2123961617234,-0.365909155705961));
#29674=CARTESIAN_POINT('Ctrl Pts',(374.213891062114,-15.2185093971726,-0.262469023419861));
#29675=CARTESIAN_POINT('Ctrl Pts',(374.218210843927,-15.2217966088458,-0.206847149673646));
#29676=CARTESIAN_POINT('Ctrl Pts',(374.221153783389,-15.225083820519,-0.151161453373989));
#29677=CARTESIAN_POINT('Ctrl Pts',(374.222722742927,-15.2283710321923,-0.0954848989914071));
#29678=CARTESIAN_POINT('Ctrl Pts',(374.225646482962,-15.2344967174866,0.00826779001192193));
#29679=CARTESIAN_POINT('Ctrl Pts',(374.22380511661,-15.240622402781,0.112316487565813));
#29680=CARTESIAN_POINT('Ctrl Pts',(374.217166772466,-15.2467480880754,0.216190314493111));
#29681=CARTESIAN_POINT('Ctrl Pts',(374.210536771381,-15.2528660746201,0.319933592993223));
#29682=CARTESIAN_POINT('Ctrl Pts',(374.199121807844,-15.2589840611649,0.423502018137774));
#29683=CARTESIAN_POINT('Ctrl Pts',(374.182942004536,-15.2651020477097,0.526423171743573));
#29684=CARTESIAN_POINT('Ctrl Pts',(374.166778019509,-15.2712140529687,0.629243703872613));
#29685=CARTESIAN_POINT('Ctrl Pts',(374.14585852571,-15.2773260582276,0.731417806450445));
#29686=CARTESIAN_POINT('Ctrl Pts',(374.120255515033,-15.2834380634865,0.83247747429178));
#29687=CARTESIAN_POINT('Ctrl Pts',(374.094669534451,-15.289546003285,0.933469921300837));
#29688=CARTESIAN_POINT('Ctrl Pts',(374.064406337256,-15.2956539430835,1.03334899828593));
#29689=CARTESIAN_POINT('Ctrl Pts',(374.029588980748,-15.301761882882,1.13165696397399));
#29690=CARTESIAN_POINT('Ctrl Pts',(373.994783425207,-15.3078677524603,1.22993160923945));
#29691=CARTESIAN_POINT('Ctrl Pts',(373.95542692049,-15.3139736220386,1.32663580284301));
#29692=CARTESIAN_POINT('Ctrl Pts',(373.911692128891,-15.3200794916169,1.42132777006712));
#29693=CARTESIAN_POINT('Ctrl Pts',(373.867961104058,-15.3261848353123,1.51601158171345));
#29694=CARTESIAN_POINT('Ctrl Pts',(373.819852720375,-15.3322901790076,1.60868312717393));
#29695=CARTESIAN_POINT('Ctrl Pts',(373.767587096109,-15.3383955227029,1.69892219105149));
#29696=CARTESIAN_POINT('Ctrl Pts',(373.71531276046,-15.3445018840075,1.78917629554126));
#29697=CARTESIAN_POINT('Ctrl Pts',(373.658880019764,-15.3506082453121,1.87699674618686));
#29698=CARTESIAN_POINT('Ctrl Pts',(373.598553654873,-15.3567146066167,1.96199018738174));
#29699=CARTESIAN_POINT('Ctrl Pts',(373.53816807586,-15.3628269616989,2.04706705498447));
#29700=CARTESIAN_POINT('Ctrl Pts',(373.473881487395,-15.3689393167812,2.12931102659843));
#29701=CARTESIAN_POINT('Ctrl Pts',(373.406000461701,-15.3750516718634,2.20835993980987));
#29702=CARTESIAN_POINT('Ctrl Pts',(373.338082407272,-15.3811673612026,2.28745197377941));
#29703=CARTESIAN_POINT('Ctrl Pts',(373.266566299743,-15.3872830505417,2.3633451686863));
#29704=CARTESIAN_POINT('Ctrl Pts',(373.19179596917,-15.3933987398809,2.43571385744193));
#29705=CARTESIAN_POINT('Ctrl Pts',(373.116916696127,-15.399523339951,2.50818798940859));
#29706=CARTESIAN_POINT('Ctrl Pts',(373.038774048626,-15.4056479400212,2.57712707956269));
#29707=CARTESIAN_POINT('Ctrl Pts',(372.957745372005,-15.4117725400914,2.64224537751176));
#29708=CARTESIAN_POINT('Ctrl Pts',(372.915824972209,-15.414941118109,2.67593450089272));
#29709=CARTESIAN_POINT('Ctrl Pts',(372.873132607385,-15.4181096961266,2.70860167443043));
#29710=CARTESIAN_POINT('Ctrl Pts',(372.829723411387,-15.4212782741442,2.7402119846744));
#29711=CARTESIAN_POINT('Ctrl Pts',(372.745956983784,-15.4273926573989,2.8012101834123));
#29712=CARTESIAN_POINT('Ctrl Pts',(372.659259889217,-15.4335070406537,2.8584593510474));
#29713=CARTESIAN_POINT('Ctrl Pts',(372.570001202592,-15.4396214239084,2.91166762753366));
#29714=CARTESIAN_POINT('Ctrl Pts',(372.480861478248,-15.4457276580293,2.96480498903985));
#29715=CARTESIAN_POINT('Ctrl Pts',(372.389167315509,-15.4518338921502,3.01391195612958));
#29716=CARTESIAN_POINT('Ctrl Pts',(372.295318353059,-15.4579401262711,3.05873872731598));
#29717=CARTESIAN_POINT('Ctrl Pts',(372.203034376697,-15.463944535383,3.10281798599457));
#29718=CARTESIAN_POINT('Ctrl Pts',(372.108667275517,-15.4699489444949,3.1427585082035));
#29719=CARTESIAN_POINT('Ctrl Pts',(372.012622422842,-15.4759533536068,3.17836489467751));
#29720=CARTESIAN_POINT('',(367.444568011016,-14.2687123280742,-0.00103428840593673));
#29721=CARTESIAN_POINT('Ctrl Pts',(372.012622422822,-15.1306250182556,3.1783648946846));
#29722=CARTESIAN_POINT('Ctrl Pts',(372.161032596329,-15.1217079361894,3.12334528824775));
#29723=CARTESIAN_POINT('Ctrl Pts',(372.305414148786,-15.1131054391572,3.05799614709269));
#29724=CARTESIAN_POINT('Ctrl Pts',(372.626234746501,-15.0935376841111,2.8847866973167));
#29725=CARTESIAN_POINT('Ctrl Pts',(372.798420158046,-15.0826949788232,2.77042447763917));
#29726=CARTESIAN_POINT('Ctrl Pts',(373.014175051594,-15.0673780481445,2.59684781429391));
#29727=CARTESIAN_POINT('Ctrl Pts',(373.067817887976,-15.0634051567002,2.55085715505148));
#29728=CARTESIAN_POINT('Ctrl Pts',(373.149864917275,-15.056994278482,2.47594112509051));
#29729=CARTESIAN_POINT('Ctrl Pts',(373.1792540704,-15.0546253927127,2.44812513828116));
#29730=CARTESIAN_POINT('Ctrl Pts',(373.244456133965,-15.0491902514634,2.38416159347616));
#29731=CARTESIAN_POINT('Ctrl Pts',(373.279962741684,-15.0461059021237,2.34772517642751));
#29732=CARTESIAN_POINT('Ctrl Pts',(373.356662537957,-15.0391883457301,2.26538834555573));
#29733=CARTESIAN_POINT('Ctrl Pts',(373.39745034035,-15.0353364008036,2.21913455438393));
#29734=CARTESIAN_POINT('Ctrl Pts',(373.527516817818,-15.0225304767566,2.06326570295236));
#29735=CARTESIAN_POINT('Ctrl Pts',(373.611202371626,-15.0134356867424,1.94917852805273));
#29736=CARTESIAN_POINT('Ctrl Pts',(373.791970452569,-14.9920290988576,1.66736945561437));
#29737=CARTESIAN_POINT('Ctrl Pts',(373.882301309212,-14.9798215417997,1.49587559400311));
#29738=CARTESIAN_POINT('Ctrl Pts',(373.987577673462,-14.9633829645738,1.24633047091956));
#29739=CARTESIAN_POINT('Ctrl Pts',(374.01519497254,-14.9587633231341,1.17405676600786));
#29740=CARTESIAN_POINT('Ctrl Pts',(374.063345615591,-14.9500560196876,1.03383390403054));
#29741=CARTESIAN_POINT('Ctrl Pts',(374.084265342552,-14.9459581893863,0.966061689284126));
#29742=CARTESIAN_POINT('Ctrl Pts',(374.132246648781,-14.9356436411694,0.791346983459715));
#29743=CARTESIAN_POINT('Ctrl Pts',(374.15624401516,-14.9295212654196,0.683647579028431));
#29744=CARTESIAN_POINT('Ctrl Pts',(374.208333809067,-14.9127540858364,0.380996778704372));
#29745=CARTESIAN_POINT('Ctrl Pts',(374.224760961267,-14.9023802783531,0.184495066474512));
#29746=CARTESIAN_POINT('Ctrl Pts',(374.223581654608,-14.8849369854442,-0.139902469650937));
#29747=CARTESIAN_POINT('Ctrl Pts',(374.215915642548,-14.8779955794848,-0.267343846137505));
#29748=CARTESIAN_POINT('Ctrl Pts',(374.195477810469,-14.8680221677311,-0.441970342865693));
#29749=CARTESIAN_POINT('Ctrl Pts',(374.188845276725,-14.8652433628548,-0.489774723662178));
#29750=CARTESIAN_POINT('Ctrl Pts',(374.174560167472,-14.859954783472,-0.578737997443816));
#29751=CARTESIAN_POINT('Ctrl Pts',(374.16716147609,-14.8574570100149,-0.619926708056189));
#29752=CARTESIAN_POINT('Ctrl Pts',(374.143590976873,-14.8501412982478,-0.738487490188065));
#29753=CARTESIAN_POINT('Ctrl Pts',(374.125473354803,-14.8452384031095,-0.815442244455483));
#29754=CARTESIAN_POINT('Ctrl Pts',(374.041334333776,-14.8251222660819,-1.1240317721796));
#29755=CARTESIAN_POINT('Ctrl Pts',(373.953404546068,-14.8094634602587,-1.34896624894075));
#29756=CARTESIAN_POINT('Ctrl Pts',(373.784823303504,-14.7864706281466,-1.67347145753088));
#29757=CARTESIAN_POINT('Ctrl Pts',(373.721193318367,-14.7787644272893,-1.78099537334861));
#29758=CARTESIAN_POINT('Ctrl Pts',(373.61146277217,-14.7668915466797,-1.94502602878411));
#29759=CARTESIAN_POINT('Ctrl Pts',(373.569231248015,-14.7625977571072,-2.00397356073716));
#29760=CARTESIAN_POINT('Ctrl Pts',(373.479789195423,-14.7540237279204,-2.12071850201278));
#29761=CARTESIAN_POINT('Ctrl Pts',(373.432496037024,-14.7497497992707,-2.17840236998975));
#29762=CARTESIAN_POINT('Ctrl Pts',(373.286745472786,-14.7372699636077,-2.34466942369706));
#29763=CARTESIAN_POINT('Ctrl Pts',(373.183107685914,-14.7292694251476,-2.44848278155932));
#29764=CARTESIAN_POINT('Ctrl Pts',(372.87269969643,-14.7070186511462,-2.7215091649089));
#29765=CARTESIAN_POINT('Ctrl Pts',(372.652247452356,-14.6931519156511,-2.87344939549034));
#29766=CARTESIAN_POINT('Ctrl Pts',(372.37326153728,-14.6752685385109,-3.02066635570474));
#29767=CARTESIAN_POINT('Ctrl Pts',(372.329743820011,-14.6724681911783,-3.04244532166582));
#29768=CARTESIAN_POINT('Ctrl Pts',(372.248094252012,-14.6671673678145,-3.08113290220045));
#29769=CARTESIAN_POINT('Ctrl Pts',(372.210091483007,-14.6646799540019,-3.09828822672553));
#29770=CARTESIAN_POINT('Ctrl Pts',(372.100327774014,-14.6574539130264,-3.14542072861473));
#29771=CARTESIAN_POINT('Ctrl Pts',(372.027840722395,-14.6526335624937,-3.17363421292851));
#29772=CARTESIAN_POINT('Ctrl Pts',(371.734843158155,-14.6331231069796,-3.27621729852323));
#29773=CARTESIAN_POINT('Ctrl Pts',(371.507899067952,-14.618003500171,-3.33029138693313));
#29774=CARTESIAN_POINT('Ctrl Pts',(371.146969311252,-14.5950526482753,-3.37785555533012));
#29775=CARTESIAN_POINT('Ctrl Pts',(371.015843132775,-14.5869221363978,-3.38743469113806));
#29776=CARTESIAN_POINT('Ctrl Pts',(370.811330121631,-14.5745985275255,-3.39046142114457));
#29777=CARTESIAN_POINT('Ctrl Pts',(370.738161100129,-14.5702590859374,-3.38917573328246));
#29778=CARTESIAN_POINT('Ctrl Pts',(370.591430165902,-14.5616829878185,-3.38184113696394));
#29779=CARTESIAN_POINT('Ctrl Pts',(370.517909962575,-14.5574497732543,-3.37575637345786));
#29780=CARTESIAN_POINT('Ctrl Pts',(370.308142373715,-14.5455123115099,-3.35148120805942));
#29781=CARTESIAN_POINT('Ctrl Pts',(370.172722164459,-14.5379821371407,-3.32739884052919));
#29782=CARTESIAN_POINT('Ctrl Pts',(369.789857121636,-14.5167266111077,-3.23500559382736));
#29783=CARTESIAN_POINT('Ctrl Pts',(369.548242929142,-14.503394167927,-3.14676775322605));
#29784=CARTESIAN_POINT('Ctrl Pts',(369.266007709468,-14.4857513237065,-3.00571221788428));
#29785=CARTESIAN_POINT('Ctrl Pts',(369.213810524538,-14.4823912328421,-2.97789485603867));
#29786=CARTESIAN_POINT('Ctrl Pts',(369.127493438093,-14.4766262060756,-2.92895254361624));
#29787=CARTESIAN_POINT('Ctrl Pts',(369.092974450863,-14.4742609709537,-2.90856242904843));
#29788=CARTESIAN_POINT('Ctrl Pts',(369.008848629546,-14.468345250781,-2.85683547956148));
#29789=CARTESIAN_POINT('Ctrl Pts',(368.959682521089,-14.4647587832951,-2.82481651540905));
#29790=CARTESIAN_POINT('Ctrl Pts',(368.848659544897,-14.4564006769465,-2.74833872802926));
#29791=CARTESIAN_POINT('Ctrl Pts',(368.787420481439,-14.4515970621464,-2.70303805115297));
#29792=CARTESIAN_POINT('Ctrl Pts',(368.539424136349,-14.4314684463365,-2.5063234486351));
#29793=CARTESIAN_POINT('Ctrl Pts',(368.367490766731,-14.4159124005769,-2.33730139558551));
#29794=CARTESIAN_POINT('Ctrl Pts',(368.150095720162,-14.3946354824101,-2.07262546481399));
#29795=CARTESIAN_POINT('Ctrl Pts',(368.088898351667,-14.3884066571874,-1.990853991196));
#29796=CARTESIAN_POINT('Ctrl Pts',(367.992051158518,-14.3781229175823,-1.84846967827475));
#29797=CARTESIAN_POINT('Ctrl Pts',(367.954427826168,-14.3740002065088,-1.78928884980916));
#29798=CARTESIAN_POINT('Ctrl Pts',(367.877817820027,-14.3653019544361,-1.66009814992997));
#29799=CARTESIAN_POINT('Ctrl Pts',(367.83942255738,-14.3607483735162,-1.58978674066155));
#29800=CARTESIAN_POINT('Ctrl Pts',(367.763733007414,-14.3512895044746,-1.43868624120367));
#29801=CARTESIAN_POINT('Ctrl Pts',(367.72705547785,-14.346404665627,-1.35765656355363));
#29802=CARTESIAN_POINT('Ctrl Pts',(367.620696948552,-14.3310559962644,-1.09571952955257));
#29803=CARTESIAN_POINT('Ctrl Pts',(367.563322772153,-14.3208555793827,-0.910247476761653));
#29804=CARTESIAN_POINT('Ctrl Pts',(367.49749774033,-14.3041469388678,-0.607807753268595));
#29805=CARTESIAN_POINT('Ctrl Pts',(367.478694830229,-14.2978115900004,-0.493546797610184));
#29806=CARTESIAN_POINT('Ctrl Pts',(367.460581448105,-14.2885826425382,-0.33236769722821));
#29807=CARTESIAN_POINT('Ctrl Pts',(367.456341406009,-14.2858984701718,-0.28607736374207));
#29808=CARTESIAN_POINT('Ctrl Pts',(367.450383115971,-14.2809414647877,-0.20203436540787));
#29809=CARTESIAN_POINT('Ctrl Pts',(367.448341906129,-14.2786851309063,-0.164312631483862));
#29810=CARTESIAN_POINT('Ctrl Pts',(367.445368697389,-14.273869259302,-0.0847391577010026));
#29811=CARTESIAN_POINT('Ctrl Pts',(367.444580781391,-14.2713038080906,-0.0428875832871091));
#29812=CARTESIAN_POINT('Ctrl Pts',(367.444568011016,-14.2687123280742,-0.00103428840593673));
#29813=CARTESIAN_POINT('Ctrl Pts',(367.444568012178,-14.2687125633712,-0.00103808853340888));
#29814=CARTESIAN_POINT('Ctrl Pts',(367.444486813014,-14.2522952246477,0.264107747439789));
#29815=CARTESIAN_POINT('Ctrl Pts',(367.475513863648,-14.2349794374035,0.528358047726244));
#29816=CARTESIAN_POINT('Ctrl Pts',(367.568093262579,-14.2097942005167,0.91657956703046));
#29817=CARTESIAN_POINT('Ctrl Pts',(367.606854946636,-14.2014961560422,1.0449070873222));
#29818=CARTESIAN_POINT('Ctrl Pts',(367.678465512956,-14.188995533336,1.23951219689682));
#29819=CARTESIAN_POINT('Ctrl Pts',(367.706050543616,-14.1846387315909,1.30757000582848));
#29820=CARTESIAN_POINT('Ctrl Pts',(367.765625363201,-14.1760594106411,1.44184984123346));
#29821=CARTESIAN_POINT('Ctrl Pts',(367.797602562222,-14.1718393270823,1.50803379809492));
#29822=CARTESIAN_POINT('Ctrl Pts',(367.894187449857,-14.1600677601578,1.69238399549318));
#29823=CARTESIAN_POINT('Ctrl Pts',(367.96371929658,-14.1526812706842,1.80781610496656));
#29824=CARTESIAN_POINT('Ctrl Pts',(368.169445352685,-14.133049353021,2.10741596188419));
#29825=CARTESIAN_POINT('Ctrl Pts',(368.317703830206,-14.1210938331566,2.28240879893269));
#29826=CARTESIAN_POINT('Ctrl Pts',(368.537995053468,-14.1042569511467,2.49464561649203));
#29827=CARTESIAN_POINT('Ctrl Pts',(368.595351931787,-14.0999399590955,2.54624921906079));
#29828=CARTESIAN_POINT('Ctrl Pts',(368.686282515476,-14.0931084691456,2.62260957937955));
#29829=CARTESIAN_POINT('Ctrl Pts',(368.718639533968,-14.0906793160424,2.64878122313738));
#29830=CARTESIAN_POINT('Ctrl Pts',(368.789998573449,-14.085309354222,2.70435733068372));
#29831=CARTESIAN_POINT('Ctrl Pts',(368.82916857659,-14.0823564727328,2.73352624191801));
#29832=CARTESIAN_POINT('Ctrl Pts',(368.981141080323,-14.0709214243864,2.84167218438247));
#29833=CARTESIAN_POINT('Ctrl Pts',(369.098081785622,-14.062171411656,2.91459149570974));
#29834=CARTESIAN_POINT('Ctrl Pts',(369.371443525127,-14.0422852034675,3.0627472839411));
#29835=CARTESIAN_POINT('Ctrl Pts',(369.529879891887,-14.031153572064,3.13350769072499));
#29836=CARTESIAN_POINT('Ctrl Pts',(369.803261458631,-14.0129635656175,3.23125833311319));
#29837=CARTESIAN_POINT('Ctrl Pts',(369.915460915887,-14.0057628586697,3.2649370769629));
#29838=CARTESIAN_POINT('Ctrl Pts',(370.098790879406,-13.9944321512412,3.30976424414081));
#29839=CARTESIAN_POINT('Ctrl Pts',(370.168919351113,-13.9901965865602,3.32457293945563));
#29840=CARTESIAN_POINT('Ctrl Pts',(370.314135748325,-13.981612900004,3.35045787475958));
#29841=CARTESIAN_POINT('Ctrl Pts',(370.389232094695,-13.9772751940927,3.36125828875296));
#29842=CARTESIAN_POINT('Ctrl Pts',(370.746876534411,-13.9570133482044,3.40049703164021));
#29843=CARTESIAN_POINT('Ctrl Pts',(371.031882947741,-13.9421457106271,3.39587986295225));
#29844=CARTESIAN_POINT('Ctrl Pts',(371.44037943264,-13.9199453550903,3.3376119574648));
#29845=CARTESIAN_POINT('Ctrl Pts',(371.566623695341,-13.9129357714702,3.31220268270208));
#29846=CARTESIAN_POINT('Ctrl Pts',(371.736506950071,-13.9029526715152,3.26782218205719));
#29847=CARTESIAN_POINT('Ctrl Pts',(371.781654178895,-13.9002449115212,3.25502079464464));
#29848=CARTESIAN_POINT('Ctrl Pts',(371.867213124908,-13.8949837534719,3.22883007406804));
#29849=CARTESIAN_POINT('Ctrl Pts',(371.907665689606,-13.8924385122789,3.21560881994681));
#29850=CARTESIAN_POINT('Ctrl Pts',(371.969524478982,-13.8884673720548,3.19409413283978));
#29851=CARTESIAN_POINT('Ctrl Pts',(371.991114593161,-13.8870663757487,3.18633842028861));
#29852=CARTESIAN_POINT('Ctrl Pts',(372.012622418493,-13.8856567889318,3.1783648962896));
#29853=CARTESIAN_POINT('Origin',(370.834317853224,-11.,0.));
#29854=CARTESIAN_POINT('',(372.012622420937,-12.6303878084336,3.17836489538372));
#29855=CARTESIAN_POINT('',(372.012622422842,-12.9759351715034,3.17836489467752));
#29856=CARTESIAN_POINT('',(372.012622422842,-11.,3.17836489467752));
#29857=CARTESIAN_POINT('',(367.444568730885,-13.3589821967097,0.0024392836071674));
#29858=CARTESIAN_POINT('Ctrl Pts',(372.012622422842,-12.9759351715034,3.17836489467751));
#29859=CARTESIAN_POINT('Ctrl Pts',(371.915017028612,-12.9820340934391,3.21454981549423));
#29860=CARTESIAN_POINT('Ctrl Pts',(371.815689609152,-12.9881330153748,3.24625447667781));
#29861=CARTESIAN_POINT('Ctrl Pts',(371.715087288233,-12.9942319373105,3.27332403908544));
#29862=CARTESIAN_POINT('Ctrl Pts',(371.614508166246,-13.0003294528326,3.30038735924209));
#29863=CARTESIAN_POINT('Ctrl Pts',(371.51265513755,-13.0064269683546,3.32281759542008));
#29864=CARTESIAN_POINT('Ctrl Pts',(371.409989849561,-13.0125244838767,3.34050996333387));
#29865=CARTESIAN_POINT('Ctrl Pts',(371.307322076232,-13.0186221470086,3.35820275954781));
#29866=CARTESIAN_POINT('Ctrl Pts',(371.203842423507,-13.0247198101405,3.37115738811166));
#29867=CARTESIAN_POINT('Ctrl Pts',(371.100021206151,-13.0308174732724,3.37932046286574));
#29868=CARTESIAN_POINT('Ctrl Pts',(370.992791957507,-13.0371152980597,3.38775149839783));
#29869=CARTESIAN_POINT('Ctrl Pts',(370.885198813993,-13.0434131228471,3.39107091894942));
#29870=CARTESIAN_POINT('Ctrl Pts',(370.777762446394,-13.0497109476345,3.38927817513675));
#29871=CARTESIAN_POINT('Ctrl Pts',(370.673599818145,-13.0558168687185,3.38754005878492));
#29872=CARTESIAN_POINT('Ctrl Pts',(370.569584979175,-13.0619227898025,3.38099690442181));
#29873=CARTESIAN_POINT('Ctrl Pts',(370.466188147125,-13.0680287108865,3.36970111166964));
#29874=CARTESIAN_POINT('Ctrl Pts',(370.357916808497,-13.0744224875256,3.35787279374259));
#29875=CARTESIAN_POINT('Ctrl Pts',(370.250323700135,-13.0808162641646,3.34083282992388));
#29876=CARTESIAN_POINT('Ctrl Pts',(370.143936197829,-13.0872100408037,3.31870128700884));
#29877=CARTESIAN_POINT('Ctrl Pts',(370.037548695523,-13.0936038174428,3.29656974409381));
#29878=CARTESIAN_POINT('Ctrl Pts',(369.932367294469,-13.0999975940819,3.2693468176568));
#29879=CARTESIAN_POINT('Ctrl Pts',(369.828899033299,-13.106391370721,3.23721146344205));
#29880=CARTESIAN_POINT('Ctrl Pts',(369.729899428162,-13.112509008685,3.2064639922639));
#29881=CARTESIAN_POINT('Ctrl Pts',(369.63215510576,-13.1186266466489,3.17112243544486));
#29882=CARTESIAN_POINT('Ctrl Pts',(369.536121118617,-13.1247442846129,3.13130808141832));
#29883=CARTESIAN_POINT('Ctrl Pts',(369.4402080713,-13.1308542183662,3.09154386735977));
#29884=CARTESIAN_POINT('Ctrl Pts',(369.346001466061,-13.1369641521195,3.04731821790663));
#29885=CARTESIAN_POINT('Ctrl Pts',(369.253941066524,-13.1430740858728,2.99880213994855));
#29886=CARTESIAN_POINT('Ctrl Pts',(369.161970700197,-13.1491780442344,2.95033350973387));
#29887=CARTESIAN_POINT('Ctrl Pts',(369.072142739242,-13.155282002596,2.89758299346691));
#29888=CARTESIAN_POINT('Ctrl Pts',(368.984876048735,-13.1613859609576,2.84076927509254));
#29889=CARTESIAN_POINT('Ctrl Pts',(368.89766687766,-13.1674858960634,2.78399300391314));
#29890=CARTESIAN_POINT('Ctrl Pts',(368.813015974723,-13.1735858311693,2.723159088368));
#29891=CARTESIAN_POINT('Ctrl Pts',(368.731316017541,-13.1796857662751,2.65853123765991));
#29892=CARTESIAN_POINT('Ctrl Pts',(368.64964338308,-13.1857836613942,2.59392500028979));
#29893=CARTESIAN_POINT('Ctrl Pts',(368.570920065526,-13.1918815565134,2.52552761347874));
#29894=CARTESIAN_POINT('Ctrl Pts',(368.495507610443,-13.1979794516325,2.45364457710624));
#29895=CARTESIAN_POINT('Ctrl Pts',(368.420101159271,-13.2040768612718,2.38176726365232));
#29896=CARTESIAN_POINT('Ctrl Pts',(368.348005353698,-13.2101742709112,2.3064051460402));
#29897=CARTESIAN_POINT('Ctrl Pts',(368.279545996073,-13.2162716805506,2.22790166309281));
#29898=CARTESIAN_POINT('Ctrl Pts',(368.211074644952,-13.2223701584042,2.14938442700327));
#29899=CARTESIAN_POINT('Ctrl Pts',(368.146241286959,-13.2284686362579,2.06772505234103));
#29900=CARTESIAN_POINT('Ctrl Pts',(368.085331857782,-13.2345671141116,1.98330054690727));
#29901=CARTESIAN_POINT('Ctrl Pts',(368.024361334513,-13.2406717089322,1.89879136101349));
#29902=CARTESIAN_POINT('Ctrl Pts',(367.967322847398,-13.2467763037528,1.81151185189101));
#29903=CARTESIAN_POINT('Ctrl Pts',(367.914459292129,-13.2528808985734,1.72186847514613));
#29904=CARTESIAN_POINT('Ctrl Pts',(367.861566340936,-13.2589888879861,1.63217525026109));
#29905=CARTESIAN_POINT('Ctrl Pts',(367.81285314498,-13.2650968773988,1.54011591473524));
#29906=CARTESIAN_POINT('Ctrl Pts',(367.7685159951,-13.2712048668115,1.4461203370483));
#29907=CARTESIAN_POINT('Ctrl Pts',(367.724112968819,-13.2773219315112,1.35198510017342));
#29908=CARTESIAN_POINT('Ctrl Pts',(367.684099136276,-13.2834389962109,1.25590826811917));
#29909=CARTESIAN_POINT('Ctrl Pts',(367.648622161941,-13.2895560609105,1.15833847602657));
#29910=CARTESIAN_POINT('Ctrl Pts',(367.629787624147,-13.2928035781647,1.1065391901173));
#29911=CARTESIAN_POINT('Ctrl Pts',(367.612230948321,-13.2960510954188,1.05431936189359));
#29912=CARTESIAN_POINT('Ctrl Pts',(367.595968408265,-13.299298612673,1.00174744064329));
#29913=CARTESIAN_POINT('Ctrl Pts',(367.559542178408,-13.3065726799196,0.883992349435457));
#29914=CARTESIAN_POINT('Ctrl Pts',(367.529519206534,-13.3138467471663,0.764172611276169));
#29915=CARTESIAN_POINT('Ctrl Pts',(367.506097814895,-13.3211208144129,0.642928020050624));
#29916=CARTESIAN_POINT('Ctrl Pts',(367.482901522175,-13.3283249718652,0.52284868949087));
#29917=CARTESIAN_POINT('Ctrl Pts',(367.466180569951,-13.3355291293175,0.401371825250862));
#29918=CARTESIAN_POINT('Ctrl Pts',(367.456080611714,-13.3427332867697,0.279138321575045));
#29919=CARTESIAN_POINT('Ctrl Pts',(367.448487157846,-13.3481495900831,0.187239479087665));
#29920=CARTESIAN_POINT('Ctrl Pts',(367.444635275771,-13.3535658933964,0.0949133469536027));
#29921=CARTESIAN_POINT('Ctrl Pts',(367.444568730885,-13.3589821967097,0.00243928360717191));
#29922=CARTESIAN_POINT('Ctrl Pts',(367.444568730885,-13.3589821967504,0.00243928291276102));
#29923=CARTESIAN_POINT('Ctrl Pts',(367.444494118151,-13.3650551700416,-0.101246290872523));
#29924=CARTESIAN_POINT('Ctrl Pts',(367.449181100272,-13.3711281433329,-0.205001299518334));
#29925=CARTESIAN_POINT('Ctrl Pts',(367.458622117423,-13.3772011166241,-0.308355901186887));
#29926=CARTESIAN_POINT('Ctrl Pts',(367.468060504766,-13.3832723982799,-0.411681713281755));
#29927=CARTESIAN_POINT('Ctrl Pts',(367.482250256026,-13.3893436799356,-0.514606913146634));
#29928=CARTESIAN_POINT('Ctrl Pts',(367.501131809253,-13.3954149615913,-0.616665110718218));
#29929=CARTESIAN_POINT('Ctrl Pts',(367.520013029297,-13.4014861361136,-0.718721507377279));
#29930=CARTESIAN_POINT('Ctrl Pts',(367.543585807955,-13.4075573106359,-0.819910510422086));
#29931=CARTESIAN_POINT('Ctrl Pts',(367.571739325754,-13.4136284851582,-0.919775197855785));
#29932=CARTESIAN_POINT('Ctrl Pts',(367.599899692094,-13.4197011365364,-1.01966417807679));
#29933=CARTESIAN_POINT('Ctrl Pts',(367.632642895164,-13.4257737879145,-1.11822778979971));
#29934=CARTESIAN_POINT('Ctrl Pts',(367.66980831523,-13.4318464392927,-1.21502446331179));
#29935=CARTESIAN_POINT('Ctrl Pts',(367.707013316293,-13.4379255580158,-1.31192422482176));
#29936=CARTESIAN_POINT('Ctrl Pts',(367.748649780113,-13.4440046767389,-1.40705289148142));
#29937=CARTESIAN_POINT('Ctrl Pts',(367.794509072048,-13.4500837954619,-1.49998921208925));
#29938=CARTESIAN_POINT('Ctrl Pts',(367.840397119325,-13.456166726,-1.59298380694277));
#29939=CARTESIAN_POINT('Ctrl Pts',(367.890513059632,-13.462249656538,-1.68378294374827));
#29940=CARTESIAN_POINT('Ctrl Pts',(367.9446034245,-13.468332587076,-1.77199198161901));
#29941=CARTESIAN_POINT('Ctrl Pts',(367.998773130277,-13.4744244401874,-1.86033040640288));
#29942=CARTESIAN_POINT('Ctrl Pts',(368.056928655357,-13.4805162932987,-1.94607079582972));
#29943=CARTESIAN_POINT('Ctrl Pts',(368.118774650797,-13.48660814641,-2.0288494715611));
#29944=CARTESIAN_POINT('Ctrl Pts',(368.137717755651,-13.4884740491483,-2.05420414687838));
#29945=CARTESIAN_POINT('Ctrl Pts',(368.157006815312,-13.4903399518866,-2.07928121494589));
#29946=CARTESIAN_POINT('Ctrl Pts',(368.17663264358,-13.4922058546248,-2.10407090872422));
#29947=CARTESIAN_POINT('Ctrl Pts',(368.240978883023,-13.4983234983102,-2.18534766045084));
#29948=CARTESIAN_POINT('Ctrl Pts',(368.309158580173,-13.5044411419956,-2.26379845328729));
#29949=CARTESIAN_POINT('Ctrl Pts',(368.380894663344,-13.5105587856809,-2.33904247799338));
#29950=CARTESIAN_POINT('Ctrl Pts',(368.452540406521,-13.5166687251836,-2.41419174502113));
#29951=CARTESIAN_POINT('Ctrl Pts',(368.527733339203,-13.5227786646863,-2.48614196861558));
#29952=CARTESIAN_POINT('Ctrl Pts',(368.606155516872,-13.5288886041889,-2.55454451230814));
#29953=CARTESIAN_POINT('Ctrl Pts',(368.684500999563,-13.5349925683196,-2.62288015997952));
#29954=CARTESIAN_POINT('Ctrl Pts',(368.766069127339,-13.5410965324503,-2.68767475020128));
#29955=CARTESIAN_POINT('Ctrl Pts',(368.850505007985,-13.547200496581,-2.74861631690664));
#29956=CARTESIAN_POINT('Ctrl Pts',(368.934885235177,-13.5533004374614,-2.80951771575182));
#29957=CARTESIAN_POINT('Ctrl Pts',(369.022129112173,-13.5594003783418,-2.86657089390966));
#29958=CARTESIAN_POINT('Ctrl Pts',(369.111849178056,-13.5655003192222,-2.91950453426009));
#29959=CARTESIAN_POINT('Ctrl Pts',(369.201539239108,-13.5715982201164,-2.97242047216103));
#29960=CARTESIAN_POINT('Ctrl Pts',(369.293703477122,-13.5776961210106,-3.02121939525926));
#29961=CARTESIAN_POINT('Ctrl Pts',(369.387926661105,-13.5837940219048,-3.06567408278523));
#29962=CARTESIAN_POINT('Ctrl Pts',(369.482142343477,-13.5898914373125,-3.1101252310358));
#29963=CARTESIAN_POINT('Ctrl Pts',(369.578416261294,-13.5959888527202,-3.15023265057975));
#29964=CARTESIAN_POINT('Ctrl Pts',(369.676310667713,-13.6020862681279,-3.18581613104176));
#29965=CARTESIAN_POINT('Ctrl Pts',(369.774222224157,-13.6081847517357,-3.22140584533847));
#29966=CARTESIAN_POINT('Ctrl Pts',(369.873754433892,-13.6142832353436,-3.25246990058782));
#29967=CARTESIAN_POINT('Ctrl Pts',(369.974452596192,-13.6203817189514,-3.27887736919951));
#29968=CARTESIAN_POINT('Ctrl Pts',(370.075251760938,-13.626486319471,-3.30531132507639));
#29969=CARTESIAN_POINT('Ctrl Pts',(370.177218801532,-13.6325909199905,-3.32707926086374));
#29970=CARTESIAN_POINT('Ctrl Pts',(370.27988705099,-13.63869552051,-3.34410100745093));
#29971=CARTESIAN_POINT('Ctrl Pts',(370.382612390891,-13.6448035155974,-3.36113221927254));
#29972=CARTESIAN_POINT('Ctrl Pts',(370.486039294524,-13.6509115106849,-3.37341193435571));
#29973=CARTESIAN_POINT('Ctrl Pts',(370.589696042567,-13.6570195057723,-3.38091189359485));
#29974=CARTESIAN_POINT('Ctrl Pts',(370.693506802752,-13.6631365760567,-3.38842299619708));
#29975=CARTESIAN_POINT('Ctrl Pts',(370.797547664726,-13.6692536463411,-3.39114014979097));
#29976=CARTESIAN_POINT('Ctrl Pts',(370.901346919323,-13.6753707166254,-3.38908721734893));
#29977=CARTESIAN_POINT('Ctrl Pts',(370.956452371767,-13.6786181766092,-3.38799734660279));
#29978=CARTESIAN_POINT('Ctrl Pts',(371.011489804652,-13.681865636593,-3.38556396081711));
#29979=CARTESIAN_POINT('Ctrl Pts',(371.066389505618,-13.6851130965768,-3.38179653596353));
#29980=CARTESIAN_POINT('Ctrl Pts',(371.169810991295,-13.6912307462231,-3.37469936296128));
#29981=CARTESIAN_POINT('Ctrl Pts',(371.27307006171,-13.6973483958694,-3.36284244566665));
#29982=CARTESIAN_POINT('Ctrl Pts',(371.375695958858,-13.7034660455157,-3.34623890498568));
#29983=CARTESIAN_POINT('Ctrl Pts',(371.478192616937,-13.70957599107,-3.3296562735119));
#29984=CARTESIAN_POINT('Ctrl Pts',(371.580057270855,-13.7156859366243,-3.30833897176935));
#29985=CARTESIAN_POINT('Ctrl Pts',(371.680822578416,-13.7217958821787,-3.28235202449816));
#29986=CARTESIAN_POINT('Ctrl Pts',(371.781489341391,-13.7278998524418,-3.25639049145967));
#29987=CARTESIAN_POINT('Ctrl Pts',(371.881058486689,-13.7340038227049,-3.22576850120469));
#29988=CARTESIAN_POINT('Ctrl Pts',(371.979072017051,-13.740107792968,-3.19060228905149));
#29989=CARTESIAN_POINT('Ctrl Pts',(372.077020946197,-13.7462077400733,-3.15545925512727));
#29990=CARTESIAN_POINT('Ctrl Pts',(372.173415900603,-13.7523076871786,-3.11577809933216));
#29991=CARTESIAN_POINT('Ctrl Pts',(372.267813985683,-13.7584076342839,-3.07172490642058));
#29992=CARTESIAN_POINT('Ctrl Pts',(372.362180502342,-13.764505541457,-3.02768644569074));
#29993=CARTESIAN_POINT('Ctrl Pts',(372.454551092437,-13.77060344863,-2.97927903395538));
#29994=CARTESIAN_POINT('Ctrl Pts',(372.544503521109,-13.7767013558031,-2.92671659780389));
#29995=CARTESIAN_POINT('Ctrl Pts',(372.634448788861,-13.7827987775349,-2.87415834603511));
#29996=CARTESIAN_POINT('Ctrl Pts',(372.721975911304,-13.7888961992666,-2.81744594242623));
#29997=CARTESIAN_POINT('Ctrl Pts',(372.80668868817,-13.7949936209984,-2.75683847041411));
#29998=CARTESIAN_POINT('Ctrl Pts',(372.891416306276,-13.8010921109668,-2.69622038028676));
#29999=CARTESIAN_POINT('Ctrl Pts',(372.973328253474,-13.8071906009353,-2.63170611310799));
#30000=CARTESIAN_POINT('Ctrl Pts',(373.052059383845,-13.8132890909038,-2.56359660747514));
#30001=CARTESIAN_POINT('Ctrl Pts',(373.130869483377,-13.8193936978,-2.49541878641881));
#30002=CARTESIAN_POINT('Ctrl Pts',(373.206492074138,-13.8254983046962,-2.423638805379));
#30003=CARTESIAN_POINT('Ctrl Pts',(373.278597102448,-13.8316029115924,-2.34859617948939));
#30004=CARTESIAN_POINT('Ctrl Pts',(373.350742226157,-13.8377109130736,-2.27351182469292));
#30005=CARTESIAN_POINT('Ctrl Pts',(373.419365611014,-13.8438189145549,-2.19516153052003));
#30006=CARTESIAN_POINT('Ctrl Pts',(373.48417715561,-13.8499269160361,-2.11391833807689));
#30007=CARTESIAN_POINT('Ctrl Pts',(373.549084996078,-13.8560439926803,-2.03255443590362));
#30008=CARTESIAN_POINT('Ctrl Pts',(373.610169436892,-13.8621610693244,-1.9482893958317));
#30009=CARTESIAN_POINT('Ctrl Pts',(373.667183367057,-13.8682781459686,-1.86152572988874));
#30010=CARTESIAN_POINT('Ctrl Pts',(373.697450585566,-13.8715255434887,-1.81546514735829));
#30011=CARTESIAN_POINT('Ctrl Pts',(373.726571390993,-13.8747729410087,-1.76870081986008));
#30012=CARTESIAN_POINT('Ctrl Pts',(373.754514171867,-13.8780203385288,-1.72129559433642));
#30013=CARTESIAN_POINT('Ctrl Pts',(373.80715409437,-13.8841379384398,-1.63199140485689));
#30014=CARTESIAN_POINT('Ctrl Pts',(373.855776908335,-13.8902555383508,-1.54012915831113));
#30015=CARTESIAN_POINT('Ctrl Pts',(373.900127182339,-13.8963731382619,-1.44610449830167));
#30016=CARTESIAN_POINT('Ctrl Pts',(373.944421603874,-13.9024830339801,-1.35219824814533));
#30017=CARTESIAN_POINT('Ctrl Pts',(373.984454004348,-13.9085929296984,-1.25613538091522));
#30018=CARTESIAN_POINT('Ctrl Pts',(374.020013688675,-13.9147028254167,-1.15833807952949));
#30019=CARTESIAN_POINT('Ctrl Pts',(374.055538596553,-13.9208067458153,-1.0606364213695));
#30020=CARTESIAN_POINT('Ctrl Pts',(374.086599343483,-13.9269106662139,-0.961204100197238));
#30021=CARTESIAN_POINT('Ctrl Pts',(374.113032752499,-13.9330145866125,-0.860484556382313));
#30022=CARTESIAN_POINT('Ctrl Pts',(374.139448739715,-13.9391144840234,-0.759831395067136));
#30023=CARTESIAN_POINT('Ctrl Pts',(374.161243347015,-13.9452143814342,-0.65789310846249));
#30024=CARTESIAN_POINT('Ctrl Pts',(374.17830304957,-13.951314278845,-0.555128876135667));
#30025=CARTESIAN_POINT('Ctrl Pts',(374.195357047372,-13.9574121364541,-0.452399008101695));
#30026=CARTESIAN_POINT('Ctrl Pts',(374.2076792185,-13.9635099940632,-0.348844162284679));
#30027=CARTESIAN_POINT('Ctrl Pts',(374.215207177643,-13.9696078516723,-0.244933539011872));
#30028=CARTESIAN_POINT('Ctrl Pts',(374.222734537736,-13.9757052240352,-0.141031184583188));
#30029=CARTESIAN_POINT('Ctrl Pts',(374.225468414252,-13.9818025963981,-0.0367735329093332));
#30030=CARTESIAN_POINT('Ctrl Pts',(374.223398387063,-13.987899968761,0.0673661462176254));
#30031=CARTESIAN_POINT('Ctrl Pts',(374.221327997124,-13.9939984096205,0.171524074663072));
#30032=CARTESIAN_POINT('Ctrl Pts',(374.214452039208,-14.0000968504799,0.275563564590752));
#30033=CARTESIAN_POINT('Ctrl Pts',(374.202812174589,-14.0061952913394,0.379013283980065));
#30034=CARTESIAN_POINT('Ctrl Pts',(374.191160633504,-14.0122998498157,0.48256677837719));
#30035=CARTESIAN_POINT('Ctrl Pts',(374.174735691732,-14.0184044082921,0.585528898027552));
#30036=CARTESIAN_POINT('Ctrl Pts',(374.153630671847,-14.0245089667684,0.687435433058516));
#30037=CARTESIAN_POINT('Ctrl Pts',(374.132513914873,-14.0306169201598,0.789398641152582));
#30038=CARTESIAN_POINT('Ctrl Pts',(374.106712000254,-14.0367248735511,0.890304683607939));
#30039=CARTESIAN_POINT('Ctrl Pts',(374.076368495392,-14.0428328269425,0.9897033374286));
#30040=CARTESIAN_POINT('Ctrl Pts',(374.045979901539,-14.0489498564594,1.08924969287799));
#30041=CARTESIAN_POINT('Ctrl Pts',(374.011036383171,-14.0550668859764,1.18728378652411));
#30042=CARTESIAN_POINT('Ctrl Pts',(373.971730126654,-14.0611839154933,1.28337418122268));
#30043=CARTESIAN_POINT('Ctrl Pts',(373.950860138787,-14.0644318038224,1.33439418539578));
#30044=CARTESIAN_POINT('Ctrl Pts',(373.928761015634,-14.0676796921516,1.38486661488869));
#30045=CARTESIAN_POINT('Ctrl Pts',(373.905466724033,-14.0709275804807,1.43472982677102));
#30046=CARTESIAN_POINT('Ctrl Pts',(373.861584129846,-14.0770460651272,1.52866387419326));
#30047=CARTESIAN_POINT('Ctrl Pts',(373.813318673387,-14.0831645497737,1.62073127437622));
#30048=CARTESIAN_POINT('Ctrl Pts',(373.760852254909,-14.0892830344203,1.71049743006276));
#30049=CARTESIAN_POINT('Ctrl Pts',(373.708467293901,-14.0953920197282,1.80012421805373));
#30050=CARTESIAN_POINT('Ctrl Pts',(373.651894565734,-14.1015010050362,1.88745650870011));
#30051=CARTESIAN_POINT('Ctrl Pts',(373.591362974889,-14.1076099903442,1.97208196067124));
#30052=CARTESIAN_POINT('Ctrl Pts',(373.530885246039,-14.1137135397775,2.05663211153655));
#30053=CARTESIAN_POINT('Ctrl Pts',(373.466455902736,-14.1198170892108,2.13847986766756));
#30054=CARTESIAN_POINT('Ctrl Pts',(373.398348300586,-14.1259206386441,2.21723993458057));
#30055=CARTESIAN_POINT('Ctrl Pts',(373.330283945048,-14.1320203124772,2.29594999083454));
#30056=CARTESIAN_POINT('Ctrl Pts',(373.258546251999,-14.1381199863104,2.3715759358255));
#30057=CARTESIAN_POINT('Ctrl Pts',(373.183449650411,-14.1442196601435,2.44376448577713));
#30058=CARTESIAN_POINT('Ctrl Pts',(373.108381597546,-14.1503170151246,2.51592559252999));
#30059=CARTESIAN_POINT('Ctrl Pts',(373.029957482597,-14.1564143701058,2.58465160994283));
#30060=CARTESIAN_POINT('Ctrl Pts',(372.948528866113,-14.162511725087,2.6496257953677));
#30061=CARTESIAN_POINT('Ctrl Pts',(372.867087713778,-14.1686100187496,2.71460998350082));
#30062=CARTESIAN_POINT('Ctrl Pts',(372.782641463345,-14.1747083124122,2.77584091462108));
#30063=CARTESIAN_POINT('Ctrl Pts',(372.695574683507,-14.1808066060748,2.83304219421901));
#30064=CARTESIAN_POINT('Ctrl Pts',(372.608500865398,-14.1869053927089,2.89024809783199));
#30065=CARTESIAN_POINT('Ctrl Pts',(372.518806455965,-14.1930041793431,2.94342347496669));
#30066=CARTESIAN_POINT('Ctrl Pts',(372.426903780437,-14.1991029659772,2.9923360651741));
#30067=CARTESIAN_POINT('Ctrl Pts',(372.334933726547,-14.2052062239312,3.04128451560261));
#30068=CARTESIAN_POINT('Ctrl Pts',(372.240752553547,-14.2113094818852,3.0859637473525));
#30069=CARTESIAN_POINT('Ctrl Pts',(372.144795581832,-14.2174127398392,3.12618828372879));
#30070=CARTESIAN_POINT('Ctrl Pts',(372.101091858123,-14.2201924763667,3.14450859951888));
#30071=CARTESIAN_POINT('Ctrl Pts',(372.057020036966,-14.2229722128942,3.16190551592873));
#30072=CARTESIAN_POINT('Ctrl Pts',(372.012622422842,-14.2257519494217,3.17836489467751));
#30073=CARTESIAN_POINT('Ctrl Pts',(372.012622418493,-13.8856567889318,3.1783648962896));
#30074=CARTESIAN_POINT('Ctrl Pts',(372.070513041571,-13.8818627345421,3.15690329962443));
#30075=CARTESIAN_POINT('Ctrl Pts',(372.12780751053,-13.8780066111693,3.13386370550035));
#30076=CARTESIAN_POINT('Ctrl Pts',(372.368620390333,-13.8614490521448,3.02929673523553));
#30077=CARTESIAN_POINT('Ctrl Pts',(372.54532893171,-13.8484466958673,2.93311549986729));
#30078=CARTESIAN_POINT('Ctrl Pts',(372.834081643333,-13.8264705281444,2.74092768553833));
#30079=CARTESIAN_POINT('Ctrl Pts',(372.950327596326,-13.8173803299904,2.6522161874872));
#30080=CARTESIAN_POINT('Ctrl Pts',(373.11669844169,-13.8040520384073,2.50732881780625));
#30081=CARTESIAN_POINT('Ctrl Pts',(373.171272194672,-13.799620172036,2.45654322432826));
#30082=CARTESIAN_POINT('Ctrl Pts',(373.275553136719,-13.7910170791153,2.35287755753538));
#30083=CARTESIAN_POINT('Ctrl Pts',(373.325324664236,-13.7868442728773,2.30011927374733));
#30084=CARTESIAN_POINT('Ctrl Pts',(373.456220449226,-13.7756453699622,2.15213161379069));
#30085=CARTESIAN_POINT('Ctrl Pts',(373.533829785163,-13.7687546485385,2.05394330388658));
#30086=CARTESIAN_POINT('Ctrl Pts',(373.725399276435,-13.7507164409805,1.7819015986162));
#30087=CARTESIAN_POINT('Ctrl Pts',(373.829099798953,-13.7398195621247,1.60150000471844));
#30088=CARTESIAN_POINT('Ctrl Pts',(373.945786505632,-13.7246202110521,1.34699668922024));
#30089=CARTESIAN_POINT('Ctrl Pts',(373.973819360757,-13.7206486476821,1.28029938012707));
#30090=CARTESIAN_POINT('Ctrl Pts',(374.019977543795,-13.7134144162638,1.15982369413772));
#30091=CARTESIAN_POINT('Ctrl Pts',(374.03892686138,-13.7101852452605,1.10639007075722));
#30092=CARTESIAN_POINT('Ctrl Pts',(374.068990447567,-13.7045492733195,1.01435184059395));
#30093=CARTESIAN_POINT('Ctrl Pts',(374.080773977305,-13.7021761506524,0.97598087231898));
#30094=CARTESIAN_POINT('Ctrl Pts',(374.108841876622,-13.6960853273582,0.878443174856708));
#30095=CARTESIAN_POINT('Ctrl Pts',(374.124205002062,-13.6923253328236,0.819030871264247));
#30096=CARTESIAN_POINT('Ctrl Pts',(374.194609012155,-13.6727906785065,0.512686148507764));
#30097=CARTESIAN_POINT('Ctrl Pts',(374.223493580583,-13.656299272527,0.260568479008471));
#30098=CARTESIAN_POINT('Ctrl Pts',(374.224365259854,-13.6316788807919,-0.129190701480439));
#30099=CARTESIAN_POINT('Ctrl Pts',(374.216393176629,-13.6231952762068,-0.265866496446257));
#30100=CARTESIAN_POINT('Ctrl Pts',(374.191449947153,-13.6104994103048,-0.474867275195763));
#30101=CARTESIAN_POINT('Ctrl Pts',(374.180333843797,-13.6061240023498,-0.54773445222052));
#30102=CARTESIAN_POINT('Ctrl Pts',(374.153455770233,-13.597540289508,-0.692162265783858));
#30103=CARTESIAN_POINT('Ctrl Pts',(374.137731965901,-13.5933333741653,-0.763689358469013));
#30104=CARTESIAN_POINT('Ctrl Pts',(374.08722267471,-13.5817242720805,-0.962504994023995));
#30105=CARTESIAN_POINT('Ctrl Pts',(374.047305656414,-13.5744784172473,-1.0883563663356));
#30106=CARTESIAN_POINT('Ctrl Pts',(373.928903596409,-13.5565669101734,-1.39774104190696));
#30107=CARTESIAN_POINT('Ctrl Pts',(373.841375594435,-13.5460939647492,-1.57725731991146));
#30108=CARTESIAN_POINT('Ctrl Pts',(373.70184924996,-13.5313944454596,-1.80907255757174));
#30109=CARTESIAN_POINT('Ctrl Pts',(373.663200171553,-13.5274796950031,-1.86893115289559));
#30110=CARTESIAN_POINT('Ctrl Pts',(373.590789661747,-13.5203344156567,-1.97368099554282));
#30111=CARTESIAN_POINT('Ctrl Pts',(373.557743871837,-13.5171361034214,-2.01903528007202));
#30112=CARTESIAN_POINT('Ctrl Pts',(373.499134539538,-13.5115293513256,-2.0954166428895));
#30113=CARTESIAN_POINT('Ctrl Pts',(373.474118100249,-13.5091531645693,-2.12684580870211));
#30114=CARTESIAN_POINT('Ctrl Pts',(373.409024653371,-13.5030139021602,-2.20570737566982));
#30115=CARTESIAN_POINT('Ctrl Pts',(373.368194640828,-13.4992068230788,-2.25249363136843));
#30116=CARTESIAN_POINT('Ctrl Pts',(373.155335085181,-13.4796825656924,-2.48329044005629));
#30117=CARTESIAN_POINT('Ctrl Pts',(372.964460462119,-13.4632649864131,-2.64883923427552));
#30118=CARTESIAN_POINT('Ctrl Pts',(372.644531091319,-13.438728230231,-2.86917823654959));
#30119=CARTESIAN_POINT('Ctrl Pts',(372.527470123213,-13.4302579685121,-2.93977854851025));
#30120=CARTESIAN_POINT('Ctrl Pts',(372.341191696741,-13.4175761129384,-3.03729537254865));
#30121=CARTESIAN_POINT('Ctrl Pts',(372.274826728343,-13.4132020209173,-3.06932685687098));
#30122=CARTESIAN_POINT('Ctrl Pts',(372.140513486671,-13.404618654692,-3.12883696725013));
#30123=CARTESIAN_POINT('Ctrl Pts',(372.072613462428,-13.4004108427868,-3.15632585566594));
#30124=CARTESIAN_POINT('Ctrl Pts',(371.879889402131,-13.3887907790295,-3.22717123512479));
#30125=CARTESIAN_POINT('Ctrl Pts',(371.753342181182,-13.3815354367505,-3.2654636585629));
#30126=CARTESIAN_POINT('Ctrl Pts',(371.399454321044,-13.3618595177126,-3.35033765181226));
#30127=CARTESIAN_POINT('Ctrl Pts',(371.169099941822,-13.3497538004549,-3.38113161314876));
#30128=CARTESIAN_POINT('Ctrl Pts',(370.859832731438,-13.3327293816378,-3.39054265895115));
#30129=CARTESIAN_POINT('Ctrl Pts',(370.782191860392,-13.328386616616,-3.39023770795044));
#30130=CARTESIAN_POINT('Ctrl Pts',(370.662992540345,-13.3215250644156,-3.38567414188377));
#30131=CARTESIAN_POINT('Ctrl Pts',(370.621383690552,-13.3190929483916,-3.38331209011377));
#30132=CARTESIAN_POINT('Ctrl Pts',(370.531276565446,-13.3137290006523,-3.37652805783786));
#30133=CARTESIAN_POINT('Ctrl Pts',(370.482811430765,-13.3107854808054,-3.37182716544576));
#30134=CARTESIAN_POINT('Ctrl Pts',(370.295843737569,-13.299245024251,-3.34961763941438));
#30135=CARTESIAN_POINT('Ctrl Pts',(370.158379788995,-13.2903709614666,-3.32460442276465));
#30136=CARTESIAN_POINT('Ctrl Pts',(369.837840479298,-13.2692534386837,-3.24557413017229));
#30137=CARTESIAN_POINT('Ctrl Pts',(369.656981361309,-13.2570144628041,-3.18443207195036));
#30138=CARTESIAN_POINT('Ctrl Pts',(369.384529360016,-13.2385061653722,-3.06592003053975));
#30139=CARTESIAN_POINT('Ctrl Pts',(369.288897681958,-13.231989093711,-3.01884618102679));
#30140=CARTESIAN_POINT('Ctrl Pts',(369.133884765843,-13.2213951101897,-2.93324192970972));
#30141=CARTESIAN_POINT('Ctrl Pts',(369.073211804589,-13.2172396716112,-2.89722064228256));
#30142=CARTESIAN_POINT('Ctrl Pts',(368.947499368076,-13.208594598721,-2.8171760768655));
#30143=CARTESIAN_POINT('Ctrl Pts',(368.88277589865,-13.2041228091436,-2.77273337615041));
#30144=CARTESIAN_POINT('Ctrl Pts',(368.622384966883,-13.1859616225786,-2.58029550703354));
#30145=CARTESIAN_POINT('Ctrl Pts',(368.44152685087,-13.1729947798156,-2.41353105079744));
#30146=CARTESIAN_POINT('Ctrl Pts',(368.210693099577,-13.1541956964911,-2.14899688721272));
#30147=CARTESIAN_POINT('Ctrl Pts',(368.144916777435,-13.1485004376562,-2.0660866797941));
#30148=CARTESIAN_POINT('Ctrl Pts',(368.040914673143,-13.1386658089053,-1.92159443589303));
#30149=CARTESIAN_POINT('Ctrl Pts',(368.000590611035,-13.1346073295086,-1.86161623255362));
#30150=CARTESIAN_POINT('Ctrl Pts',(367.940417797524,-13.1280753528127,-1.76562510083742));
#30151=CARTESIAN_POINT('Ctrl Pts',(367.919254974156,-13.1256744277895,-1.73046174111507));
#30152=CARTESIAN_POINT('Ctrl Pts',(367.873477350455,-13.1202286800069,-1.65117534676109));
#30153=CARTESIAN_POINT('Ctrl Pts',(367.849203142064,-13.1171676264391,-1.60687462762368));
#30154=CARTESIAN_POINT('Ctrl Pts',(367.73574006706,-13.1020384936368,-1.38835355838938));
#30155=CARTESIAN_POINT('Ctrl Pts',(367.660768982404,-13.0894265950276,-1.20718219184014));
#30156=CARTESIAN_POINT('Ctrl Pts',(367.542651834828,-13.0643260347919,-0.833067192698608));
#30157=CARTESIAN_POINT('Ctrl Pts',(367.499873045884,-13.0518903585881,-0.640750715244693));
#30158=CARTESIAN_POINT('Ctrl Pts',(367.463644463792,-13.0351363705873,-0.367664290187277));
#30159=CARTESIAN_POINT('Ctrl Pts',(367.456007192223,-13.0304201956665,-0.289196621600946));
#30160=CARTESIAN_POINT('Ctrl Pts',(367.446737283081,-13.0216402382619,-0.140229022906423));
#30161=CARTESIAN_POINT('Ctrl Pts',(367.444554678254,-13.0175624591175,-0.0698064440528915));
#30162=CARTESIAN_POINT('Ctrl Pts',(367.444587737125,-13.0075274155424,0.106152147204749));
#30163=CARTESIAN_POINT('Ctrl Pts',(367.449534158312,-13.0016522954613,0.211614329611914));
#30164=CARTESIAN_POINT('Ctrl Pts',(367.472616562001,-12.9881242758317,0.457607467445845));
#30165=CARTESIAN_POINT('Ctrl Pts',(367.494654575996,-12.9805656122501,0.597571515404709));
#30166=CARTESIAN_POINT('Ctrl Pts',(367.565230946193,-12.9631956814482,0.914979184482697));
#30167=CARTESIAN_POINT('Ctrl Pts',(367.619575199875,-12.9534138893466,1.09065721272535));
#30168=CARTESIAN_POINT('Ctrl Pts',(367.707038470983,-12.940143029684,1.3088866854747));
#30169=CARTESIAN_POINT('Ctrl Pts',(367.727296864628,-12.9371893487096,1.35627454739195));
#30170=CARTESIAN_POINT('Ctrl Pts',(367.765508652112,-12.9317909186456,1.44030499338984));
#30171=CARTESIAN_POINT('Ctrl Pts',(367.783057472938,-12.9293669007204,1.47711809993816));
#30172=CARTESIAN_POINT('Ctrl Pts',(367.832449212682,-12.9226979167539,1.57609231510798));
#30173=CARTESIAN_POINT('Ctrl Pts',(367.86555490037,-12.918390653364,1.63759809453041));
#30174=CARTESIAN_POINT('Ctrl Pts',(367.950627351603,-12.9077682565904,1.78458238135337));
#30175=CARTESIAN_POINT('Ctrl Pts',(368.004524182653,-12.9013955768554,1.86886898487573));
#30176=CARTESIAN_POINT('Ctrl Pts',(368.212063998336,-12.8783199440914,2.16382400185837));
#30177=CARTESIAN_POINT('Ctrl Pts',(368.386176483354,-12.8616300671005,2.35902356048105));
#30178=CARTESIAN_POINT('Ctrl Pts',(368.638456329798,-12.8411462389077,2.58350927174964));
#30179=CARTESIAN_POINT('Ctrl Pts',(368.69767913548,-12.8365520910356,2.63269906327869));
#30180=CARTESIAN_POINT('Ctrl Pts',(368.814743362971,-12.8278597849995,2.72337658936432));
#30181=CARTESIAN_POINT('Ctrl Pts',(368.872316622805,-12.8237526035339,2.765142561834));
#30182=CARTESIAN_POINT('Ctrl Pts',(369.023813935776,-12.8133360112139,2.86792886438516));
#30183=CARTESIAN_POINT('Ctrl Pts',(369.119525748788,-12.8071253121815,2.92616329049916));
#30184=CARTESIAN_POINT('Ctrl Pts',(369.357145420782,-12.7923784464163,3.05506851396676));
#30185=CARTESIAN_POINT('Ctrl Pts',(369.501463512324,-12.7839682936873,3.12073440765705));
#30186=CARTESIAN_POINT('Ctrl Pts',(369.793131937548,-12.767316107652,3.22950831598888));
#30187=CARTESIAN_POINT('Ctrl Pts',(369.939860307399,-12.7590940794592,3.27318344130942));
#30188=CARTESIAN_POINT('Ctrl Pts',(370.140121829912,-12.7475200622096,3.31831898607792));
#30189=CARTESIAN_POINT('Ctrl Pts',(370.191479870665,-12.7445209553623,3.3286495304485));
#30190=CARTESIAN_POINT('Ctrl Pts',(370.282667467491,-12.7391097777666,3.34480274785764));
#30191=CARTESIAN_POINT('Ctrl Pts',(370.322397974328,-12.7367213499059,3.35111340512486));
#30192=CARTESIAN_POINT('Ctrl Pts',(370.429153553032,-12.7302289453937,3.36612749807673));
#30193=CARTESIAN_POINT('Ctrl Pts',(370.496339512593,-12.7260674455509,3.37353551269637));
#30194=CARTESIAN_POINT('Ctrl Pts',(370.658229348029,-12.7159252226104,3.38650137505278));
#30195=CARTESIAN_POINT('Ctrl Pts',(370.753033665052,-12.7098928150693,3.39010177182418));
#30196=CARTESIAN_POINT('Ctrl Pts',(371.107412093876,-12.6872371642439,3.38868606231617));
#30197=CARTESIAN_POINT('Ctrl Pts',(371.366028351237,-12.670575376013,3.35784066164272));
#30198=CARTESIAN_POINT('Ctrl Pts',(371.696309200672,-12.6498999753054,3.27929183180326));
#30199=CARTESIAN_POINT('Ctrl Pts',(371.773337089374,-12.6451144086172,3.25807127194599));
#30200=CARTESIAN_POINT('Ctrl Pts',(371.904370087706,-12.6370269314704,3.21693874071087));
#30201=CARTESIAN_POINT('Ctrl Pts',(371.958745574722,-12.6336868080168,3.19833847805212));
#30202=CARTESIAN_POINT('Ctrl Pts',(372.012622420937,-12.6303878084336,3.17836489538373));
#30203=CARTESIAN_POINT('Origin',(370.834317853224,-11.,0.));
#30204=CARTESIAN_POINT('',(372.012622422842,-11.3828409270354,3.1783648946775));
#30205=CARTESIAN_POINT('',(372.012622422842,-11.7257572018857,3.1783648946775));
#30206=CARTESIAN_POINT('',(372.012622422842,-11.,3.17836489467752));
#30207=CARTESIAN_POINT('',(373.407552280239,-11.,-2.20655152809226));
#30208=CARTESIAN_POINT('Ctrl Pts',(372.012622422842,-11.3828409270354,3.17836489467751));
#30209=CARTESIAN_POINT('Ctrl Pts',(372.109345119701,-11.376754041059,3.1425072132997));
#30210=CARTESIAN_POINT('Ctrl Pts',(372.204587584932,-11.3706671550826,3.10217174787753));
#30211=CARTESIAN_POINT('Ctrl Pts',(372.297905397225,-11.3645802691062,3.05750168659702));
#30212=CARTESIAN_POINT('Ctrl Pts',(372.391108113364,-11.3585008905623,3.01288672039581));
#30213=CARTESIAN_POINT('Ctrl Pts',(372.482390510664,-11.3524215120183,2.96394797056057));
#30214=CARTESIAN_POINT('Ctrl Pts',(372.571325986317,-11.3463421334743,2.91087749794947));
#30215=CARTESIAN_POINT('Ctrl Pts',(372.660174141899,-11.3402687238843,2.85785913185024));
#30216=CARTESIAN_POINT('Ctrl Pts',(372.746679591279,-11.3341953142943,2.800717330631));
#30217=CARTESIAN_POINT('Ctrl Pts',(372.830439152938,-11.3281219047043,2.73969064299737));
#30218=CARTESIAN_POINT('Ctrl Pts',(372.914152482963,-11.3220518473722,2.67869763944042));
#30219=CARTESIAN_POINT('Ctrl Pts',(372.995122590053,-11.3159817900401,2.61382426280361));
#30220=CARTESIAN_POINT('Ctrl Pts',(373.072974790305,-11.309911732708,2.54535266329834));
#30221=CARTESIAN_POINT('Ctrl Pts',(373.150804777861,-11.3038434072773,2.47690060002757));
#30222=CARTESIAN_POINT('Ctrl Pts',(373.225518303846,-11.2977750818467,2.40485263805723));
#30223=CARTESIAN_POINT('Ctrl Pts',(373.296774077596,-11.291706756416,2.32953094110233));
#30224=CARTESIAN_POINT('Ctrl Pts',(373.368028221444,-11.285638569792,2.2542109670526));
#30225=CARTESIAN_POINT('Ctrl Pts',(373.435824475127,-11.279570383168,2.17561771971967));
#30226=CARTESIAN_POINT('Ctrl Pts',(373.499859378019,-11.2735021965439,2.09410922401186));
#30227=CARTESIAN_POINT('Ctrl Pts',(373.563909621778,-11.2674325561622,2.01258120128319));
#30228=CARTESIAN_POINT('Ctrl Pts',(373.624196458741,-11.2613629157804,1.92813688067976));
#30229=CARTESIAN_POINT('Ctrl Pts',(373.680458166391,-11.2552932753986,1.84116549507775));
#30230=CARTESIAN_POINT('Ctrl Pts',(373.736781306444,-11.2492170075501,1.75409914504173));
#30231=CARTESIAN_POINT('Ctrl Pts',(373.78907031061,-11.2431407397016,1.66450058384919));
#30232=CARTESIAN_POINT('Ctrl Pts',(373.837108147384,-11.2370644718531,1.57278590780703));
#30233=CARTESIAN_POINT('Ctrl Pts',(373.885176022134,-11.2309844045249,1.48101388273754));
#30234=CARTESIAN_POINT('Ctrl Pts',(373.928987255592,-11.2249043371967,1.38712349765055));
#30235=CARTESIAN_POINT('Ctrl Pts',(373.968372746856,-11.2188242698685,1.29155138736463));
#30236=CARTESIAN_POINT('Ctrl Pts',(374.007818757728,-11.21273485993,1.19583242130786));
#30237=CARTESIAN_POINT('Ctrl Pts',(374.042825306534,-11.2066454499916,1.09842697564112));
#30238=CARTESIAN_POINT('Ctrl Pts',(374.073272980134,-11.2005560400532,0.999787351572205));
#30239=CARTESIAN_POINT('Ctrl Pts',(374.086021238196,-11.1980064406861,0.958487533422621));
#30240=CARTESIAN_POINT('Ctrl Pts',(374.097970920648,-11.195456841319,0.916971485992314));
#30241=CARTESIAN_POINT('Ctrl Pts',(374.109115940059,-11.1929072419519,0.875272844868533));
#30242=CARTESIAN_POINT('Ctrl Pts',(374.136432135908,-11.1866582303457,0.773070398589751));
#30243=CARTESIAN_POINT('Ctrl Pts',(374.15899710704,-11.1804092187395,0.66944827717487));
#30244=CARTESIAN_POINT('Ctrl Pts',(374.176670633579,-11.1741602071332,0.564874281725621));
#30245=CARTESIAN_POINT('Ctrl Pts',(374.194319493875,-11.1679199170256,0.460446236069472));
#30246=CARTESIAN_POINT('Ctrl Pts',(374.207090429813,-11.1616796269179,0.355069354057219));
#30247=CARTESIAN_POINT('Ctrl Pts',(374.214893580216,-11.1554393368102,0.249224430124238));
#30248=CARTESIAN_POINT('Ctrl Pts',(374.222992272363,-11.1489626977765,0.139370664667613));
#30249=CARTESIAN_POINT('Ctrl Pts',(374.225739291032,-11.1424860587427,0.0290131187424228));
#30250=CARTESIAN_POINT('Ctrl Pts',(374.223092751951,-11.1360094197089,-0.0813003582986123));
#30251=CARTESIAN_POINT('Ctrl Pts',(374.220548538229,-11.1297831924027,-0.18734869284634));
#30252=CARTESIAN_POINT('Ctrl Pts',(374.213020091719,-11.1235569650965,-0.293355855965398));
#30253=CARTESIAN_POINT('Ctrl Pts',(374.200523137763,-11.1173307377903,-0.398832101063093));
#30254=CARTESIAN_POINT('Ctrl Pts',(374.188033748519,-11.1111082793712,-0.504244498819675));
#30255=CARTESIAN_POINT('Ctrl Pts',(374.170581884868,-11.104885820952,-0.609126219935277));
#30256=CARTESIAN_POINT('Ctrl Pts',(374.148235192962,-11.0986633625329,-0.712991534229913));
#30257=CARTESIAN_POINT('Ctrl Pts',(374.125897319379,-11.0924433595844,-0.816815861793191));
#30258=CARTESIAN_POINT('Ctrl Pts',(374.098668547604,-11.086223356636,-0.919624188569452));
#30259=CARTESIAN_POINT('Ctrl Pts',(374.066667714442,-11.0800033536875,-1.02094046701289));
#30260=CARTESIAN_POINT('Ctrl Pts',(374.034672769757,-11.0737844952825,-1.12223810223613));
#30261=CARTESIAN_POINT('Ctrl Pts',(373.997907634394,-11.0675656368775,-1.22204385312564));
#30262=CARTESIAN_POINT('Ctrl Pts',(373.956540975599,-11.0613467784725,-1.31989690378075));
#30263=CARTESIAN_POINT('Ctrl Pts',(373.915161472763,-11.0551259891582,-1.41778033708062));
#30264=CARTESIAN_POINT('Ctrl Pts',(373.869177746436,-11.0489051998439,-1.51370948746967));
#30265=CARTESIAN_POINT('Ctrl Pts',(373.818806512561,-11.0426844105296,-1.60724376022663));
#30266=CARTESIAN_POINT('Ctrl Pts',(373.768426585783,-11.0364625476517,-1.70079417482431));
#30267=CARTESIAN_POINT('Ctrl Pts',(373.713657840655,-11.0302406847738,-1.79194853828177));
#30268=CARTESIAN_POINT('Ctrl Pts',(373.654762289082,-11.0240188218959,-1.88029206421186));
#30269=CARTESIAN_POINT('Ctrl Pts',(373.595824822343,-11.0177925310024,-1.96869846303269));
#30270=CARTESIAN_POINT('Ctrl Pts',(373.532754914756,-11.011566240109,-2.05428970018529));
#30271=CARTESIAN_POINT('Ctrl Pts',(373.465857042497,-11.0053399492156,-2.13668120172826));
#30272=CARTESIAN_POINT('Ctrl Pts',(373.446732160252,-11.0035599661437,-2.16023543016395));
#30273=CARTESIAN_POINT('Ctrl Pts',(373.427294673612,-11.0017799830719,-2.18352836019791));
#30274=CARTESIAN_POINT('Ctrl Pts',(373.407552280239,-11.,-2.2065515280921));
#30275=CARTESIAN_POINT('',(368.26051712127,-11.0000050991267,-2.20589094351711));
#30276=CARTESIAN_POINT('Origin',(370.834317853224,-11.,0.));
#30277=CARTESIAN_POINT('Ctrl Pts',(368.26051712127,-11.0000050991267,-2.20589094351711));
#30278=CARTESIAN_POINT('Ctrl Pts',(368.327238606422,-11.0060529733972,-2.28374057965987));
#30279=CARTESIAN_POINT('Ctrl Pts',(368.397609433174,-11.0121008476677,-2.35869323798605));
#30280=CARTESIAN_POINT('Ctrl Pts',(368.471345744128,-11.0181487219382,-2.43038430585211));
#30281=CARTESIAN_POINT('Ctrl Pts',(368.544992275328,-11.0241892324464,-2.50198808420878));
#30282=CARTESIAN_POINT('Ctrl Pts',(368.621995836498,-11.0302297429547,-2.57033786311652));
#30283=CARTESIAN_POINT('Ctrl Pts',(368.702032769653,-11.0362702534629,-2.63510253783068));
#30284=CARTESIAN_POINT('Ctrl Pts',(368.781992799466,-11.0423049599576,-2.69980498352423));
#30285=CARTESIAN_POINT('Ctrl Pts',(368.864980068054,-11.0483396664523,-2.76092890201313));
#30286=CARTESIAN_POINT('Ctrl Pts',(368.950635343321,-11.0543743729469,-2.81818119793333));
#30287=CARTESIAN_POINT('Ctrl Pts',(369.036246162658,-11.0604059473697,-2.87540377934964));
#30288=CARTESIAN_POINT('Ctrl Pts',(369.124521876229,-11.0664375217924,-2.928758488164));
#30289=CARTESIAN_POINT('Ctrl Pts',(369.21507220216,-11.0724690962151,-2.97799405372326));
#30290=CARTESIAN_POINT('Ctrl Pts',(369.305600031744,-11.0784991721518,-3.02721738718517));
#30291=CARTESIAN_POINT('Ctrl Pts',(369.398400967749,-11.0845292480886,-3.07232340306702));
#30292=CARTESIAN_POINT('Ctrl Pts',(369.493058817224,-11.0905593240253,-3.11310604715739));
#30293=CARTESIAN_POINT('Ctrl Pts',(369.587718761295,-11.096589533396,-3.15388959368942));
#30294=CARTESIAN_POINT('Ctrl Pts',(369.684235299469,-11.1026197427668,-3.19034940715939));
#30295=CARTESIAN_POINT('Ctrl Pts',(369.782171840681,-11.1086499521375,-3.22232739348286));
#30296=CARTESIAN_POINT('Ctrl Pts',(369.880194401973,-11.1146854579899,-3.25433346686037));
#30297=CARTESIAN_POINT('Ctrl Pts',(369.979639042066,-11.1207209638422,-3.28184971538478));
#30298=CARTESIAN_POINT('Ctrl Pts',(370.080053780211,-11.1267564696946,-3.30476788453618));
#30299=CARTESIAN_POINT('Ctrl Pts',(370.180513544078,-11.1327946818529,-3.32769633013833));
#30300=CARTESIAN_POINT('Ctrl Pts',(370.281943843126,-11.1388328940113,-3.34602251246441));
#30301=CARTESIAN_POINT('Ctrl Pts',(370.383884254303,-11.1448711061696,-3.35968966356459));
#30302=CARTESIAN_POINT('Ctrl Pts',(370.485979959136,-11.1509185168003,-3.37337763488563));
#30303=CARTESIAN_POINT('Ctrl Pts',(370.588586893703,-11.1569659274309,-3.38239235982936));
#30304=CARTESIAN_POINT('Ctrl Pts',(370.691241218024,-11.1630133380615,-3.38672912098973));
#30305=CARTESIAN_POINT('Ctrl Pts',(370.772186774208,-11.1677818757749,-3.39014876791141));
#30306=CARTESIAN_POINT('Ctrl Pts',(370.853161697947,-11.1725504134883,-3.39066082917184));
#30307=CARTESIAN_POINT('Ctrl Pts',(370.933940689546,-11.1773189512018,-3.38828575432815));
#30308=CARTESIAN_POINT('Ctrl Pts',(371.037700383489,-11.1834440835401,-3.38523499776391));
#30309=CARTESIAN_POINT('Ctrl Pts',(371.14147946567,-11.1895692158784,-3.37740907499611));
#30310=CARTESIAN_POINT('Ctrl Pts',(371.244805940947,-11.1956943482167,-3.36480379700469));
#30311=CARTESIAN_POINT('Ctrl Pts',(371.34800445609,-11.2018118951539,-3.3522141294661));
#30312=CARTESIAN_POINT('Ctrl Pts',(371.450751061336,-11.2079294420911,-3.33485692743649));
#30313=CARTESIAN_POINT('Ctrl Pts',(371.552575288547,-11.2140469890283,-3.31277999859691));
#30314=CARTESIAN_POINT('Ctrl Pts',(371.654301838623,-11.2201586675737,-3.29072424753808));
#30315=CARTESIAN_POINT('Ctrl Pts',(371.755107358307,-11.2262703461192,-3.26395786434406));
#30316=CARTESIAN_POINT('Ctrl Pts',(371.854528840641,-11.2323820246646,-3.23258017745184));
#30317=CARTESIAN_POINT('Ctrl Pts',(371.953886936492,-11.2384898066899,-3.20122249550376));
#30318=CARTESIAN_POINT('Ctrl Pts',(372.051862346872,-11.2445975887152,-3.16525948434695));
#30319=CARTESIAN_POINT('Ctrl Pts',(372.148005306803,-11.2507053707405,-3.12484084983702));
#30320=CARTESIAN_POINT('Ctrl Pts',(372.244117328946,-11.2568111873462,-3.08443522161612));
#30321=CARTESIAN_POINT('Ctrl Pts',(372.338397682649,-11.2629170039519,-3.03957698459175));
#30322=CARTESIAN_POINT('Ctrl Pts',(372.43041546605,-11.2690228205576,-2.99046442427135));
#30323=CARTESIAN_POINT('Ctrl Pts',(372.522426902253,-11.2751282159966,-2.94135525163432));
#30324=CARTESIAN_POINT('Ctrl Pts',(372.612175704924,-11.2812336114356,-2.88799253923605));
#30325=CARTESIAN_POINT('Ctrl Pts',(372.699255291481,-11.2873390068746,-2.83062067643958));
#30326=CARTESIAN_POINT('Ctrl Pts',(372.78635088544,-11.2934455246377,-2.77323826726252));
#30327=CARTESIAN_POINT('Ctrl Pts',(372.870775934383,-11.2995520424008,-2.71184547624207));
#30328=CARTESIAN_POINT('Ctrl Pts',(372.952153301272,-11.3056585601639,-2.64672969482942));
#30329=CARTESIAN_POINT('Ctrl Pts',(373.033612645684,-11.3117712294801,-2.58154831740837));
#30330=CARTESIAN_POINT('Ctrl Pts',(373.112017846769,-11.3178838987964,-2.51263672652615));
#30331=CARTESIAN_POINT('Ctrl Pts',(373.187025360339,-11.3239965681127,-2.44032220177244));
#30332=CARTESIAN_POINT('Ctrl Pts',(373.262074892831,-11.3301126617228,-2.36796716669925));
#30333=CARTESIAN_POINT('Ctrl Pts',(373.333722654894,-11.336228755333,-2.29220570779313));
#30334=CARTESIAN_POINT('Ctrl Pts',(373.401663732762,-11.3423448489432,-2.21340014396834));
#30335=CARTESIAN_POINT('Ctrl Pts',(373.469705307953,-11.3484699893783,-2.13447801225122));
#30336=CARTESIAN_POINT('Ctrl Pts',(373.534028988151,-11.3545951298134,-2.05250311663614));
#30337=CARTESIAN_POINT('Ctrl Pts',(373.594371677701,-11.3607202702485,-1.96786888498483));
#30338=CARTESIAN_POINT('Ctrl Pts',(373.625587993518,-11.3638889112169,-1.92408613476411));
#30339=CARTESIAN_POINT('Ctrl Pts',(373.655739655371,-11.3670575521853,-1.87959214961196));
#30340=CARTESIAN_POINT('Ctrl Pts',(373.684795056208,-11.3702261931537,-1.83444399690095));
#30341=CARTESIAN_POINT('Ctrl Pts',(373.740856860613,-11.3763400213948,-1.74733155537407));
#30342=CARTESIAN_POINT('Ctrl Pts',(373.79301145112,-11.3824538496358,-1.65750742219757));
#30343=CARTESIAN_POINT('Ctrl Pts',(373.84098795833,-11.3885676778769,-1.56535617083158));
#30344=CARTESIAN_POINT('Ctrl Pts',(373.888903605762,-11.3946737505257,-1.4733218163604));
#30345=CARTESIAN_POINT('Ctrl Pts',(373.932651513083,-11.4007798231745,-1.37896658795512));
#30346=CARTESIAN_POINT('Ctrl Pts',(373.972004434163,-11.4068858958233,-1.28270338827569));
#30347=CARTESIAN_POINT('Ctrl Pts',(374.011318551552,-11.4129859476188,-1.1865351082987));
#30348=CARTESIAN_POINT('Ctrl Pts',(374.046246141194,-11.4190859994143,-1.08846299077901));
#30349=CARTESIAN_POINT('Ctrl Pts',(374.07660657782,-11.4251860512099,-0.988923095522964));
#30350=CARTESIAN_POINT('Ctrl Pts',(374.106946735835,-11.4312820286051,-0.88944968583013));
#30351=CARTESIAN_POINT('Ctrl Pts',(374.13272568395,-11.4373780060003,-0.788510854248488));
#30352=CARTESIAN_POINT('Ctrl Pts',(374.153811776626,-11.4434739833955,-0.686560379718457));
#30353=CARTESIAN_POINT('Ctrl Pts',(374.174890710039,-11.4495678910519,-0.584644519958852));
#30354=CARTESIAN_POINT('Ctrl Pts',(374.191279869243,-11.4556617987083,-0.481718116460937));
#30355=CARTESIAN_POINT('Ctrl Pts',(374.202898305428,-11.4617557063647,-0.378247008616722));
#30356=CARTESIAN_POINT('Ctrl Pts',(374.214515769122,-11.4678491039458,-0.274784561562532));
#30357=CARTESIAN_POINT('Ctrl Pts',(374.221363256811,-11.4739425015269,-0.170777923839477));
#30358=CARTESIAN_POINT('Ctrl Pts',(374.223411581066,-11.480035899108,-0.0666990734491657));
#30359=CARTESIAN_POINT('Ctrl Pts',(374.225460257866,-11.4861303454451,0.0373976903179456));
#30360=CARTESIAN_POINT('Ctrl Pts',(374.222708121683,-11.4922247917823,0.141566265914222));
#30361=CARTESIAN_POINT('Ctrl Pts',(374.215178102404,-11.4983192381195,0.245334543055125));
#30362=CARTESIAN_POINT('Ctrl Pts',(374.20764053214,-11.5044197958714,0.34920687738912));
#30363=CARTESIAN_POINT('Ctrl Pts',(374.195315543526,-11.5105203536233,0.452677686648481));
#30364=CARTESIAN_POINT('Ctrl Pts',(374.178277969535,-11.5166209113752,0.555279932126297));
#30365=CARTESIAN_POINT('Ctrl Pts',(374.16123093833,-11.5227248554238,0.657939130042905));
#30366=CARTESIAN_POINT('Ctrl Pts',(374.139466199945,-11.5288287994724,0.75972838772451));
#30367=CARTESIAN_POINT('Ctrl Pts',(374.113109344737,-11.534932743521,0.860192663117589));
#30368=CARTESIAN_POINT('Ctrl Pts',(374.086713195783,-11.5410457875485,0.960806714259869));
#30369=CARTESIAN_POINT('Ctrl Pts',(374.055711385291,-11.5471588315761,1.06009143237605));
#30370=CARTESIAN_POINT('Ctrl Pts',(374.02027882491,-11.5532718756036,1.15760863394903));
#30371=CARTESIAN_POINT('Ctrl Pts',(374.001225562142,-11.5565590621043,1.21004686720024));
#30372=CARTESIAN_POINT('Ctrl Pts',(373.980891938843,-11.5598462486049,1.2619743706633));
#30373=CARTESIAN_POINT('Ctrl Pts',(373.959310691612,-11.5631334351056,1.31332586303767));
#30374=CARTESIAN_POINT('Ctrl Pts',(373.919141241698,-11.5692519171414,1.4089070488158));
#30375=CARTESIAN_POINT('Ctrl Pts',(373.87451915558,-11.5753703991772,1.50279467947119));
#30376=CARTESIAN_POINT('Ctrl Pts',(373.825609166001,-11.5814888812131,1.59454737922916));
#30377=CARTESIAN_POINT('Ctrl Pts',(373.776774474275,-11.5875979437302,1.68615882397154));
#30378=CARTESIAN_POINT('Ctrl Pts',(373.723665216347,-11.5937070062472,1.77564150736957));
#30379=CARTESIAN_POINT('Ctrl Pts',(373.666493968443,-11.5998160687643,1.86257443203849));
#30380=CARTESIAN_POINT('Ctrl Pts',(373.609373083787,-11.6059197496911,1.94943077582751));
#30381=CARTESIAN_POINT('Ctrl Pts',(373.54819755381,-11.6120234306179,2.03374147229159));
#30382=CARTESIAN_POINT('Ctrl Pts',(373.483225436315,-11.6181271115447,2.11511079585554));
#30383=CARTESIAN_POINT('Ctrl Pts',(373.418294000153,-11.6242269707418,2.19642917121784));
#30384=CARTESIAN_POINT('Ctrl Pts',(373.349570967265,-11.6303268299388,2.27480950428586));
#30385=CARTESIAN_POINT('Ctrl Pts',(373.277356699608,-11.6364266891358,2.34988643503427));
#30386=CARTESIAN_POINT('Ctrl Pts',(373.205169250553,-11.6425242829952,2.42493548405761));
#30387=CARTESIAN_POINT('Ctrl Pts',(373.12949344011,-11.6486218768546,2.49668326527966));
#30388=CARTESIAN_POINT('Ctrl Pts',(373.05066817607,-11.654719470714,2.56479946758382));
#30389=CARTESIAN_POINT('Ctrl Pts',(372.971823960306,-11.6608185305997,2.63293204686428));
#30390=CARTESIAN_POINT('Ctrl Pts',(372.88982909368,-11.6669175904855,2.69743101766755));
#30391=CARTESIAN_POINT('Ctrl Pts',(372.805057149596,-11.6730166503713,2.75800501961741));
#30392=CARTESIAN_POINT('Ctrl Pts',(372.72027809087,-11.6791162221319,2.81858410535232));
#30393=CARTESIAN_POINT('Ctrl Pts',(372.632721841388,-11.6852157938926,2.8752373257988));
#30394=CARTESIAN_POINT('Ctrl Pts',(372.542791456492,-11.6913153656532,2.92771634716142));
#30395=CARTESIAN_POINT('Ctrl Pts',(372.452776154428,-11.6974206969618,2.98024492207464));
#30396=CARTESIAN_POINT('Ctrl Pts',(372.360382609697,-11.7035260282703,3.02859121535317));
#30397=CARTESIAN_POINT('Ctrl Pts',(372.266038973352,-11.7096313595789,3.07255263529865));
#30398=CARTESIAN_POINT('Ctrl Pts',(372.18297656306,-11.7150066403478,3.11125732850278));
#30399=CARTESIAN_POINT('Ctrl Pts',(372.098403070811,-11.7203819211167,3.14656372242825));
#30400=CARTESIAN_POINT('Ctrl Pts',(372.012622422842,-11.7257572018857,3.17836489467751));
#30401=CARTESIAN_POINT('Origin',(370.834317853224,-11.,0.));
#30402=CARTESIAN_POINT('',(367.444568709247,-12.1089821967158,-0.00240902652174493));
#30403=CARTESIAN_POINT('Ctrl Pts',(372.012622422842,-11.7257572018857,3.17836489467751));
#30404=CARTESIAN_POINT('Ctrl Pts',(371.915005782587,-11.7318741625465,3.21455398469513));
#30405=CARTESIAN_POINT('Ctrl Pts',(371.81582598781,-11.7379911232073,3.24620278346893));
#30406=CARTESIAN_POINT('Ctrl Pts',(371.715542697541,-11.7441080838681,3.27320146588291));
#30407=CARTESIAN_POINT('Ctrl Pts',(371.650333858663,-11.7480856149312,3.2907572593431));
#30408=CARTESIAN_POINT('Ctrl Pts',(371.584658684559,-11.7520631459944,3.30634793040135));
#30409=CARTESIAN_POINT('Ctrl Pts',(371.518645161599,-11.7560406770575,3.31995499932034));
#30410=CARTESIAN_POINT('Ctrl Pts',(371.417102457427,-11.7621589577062,3.3408855376696));
#30411=CARTESIAN_POINT('Ctrl Pts',(371.314438573247,-11.7682772383548,3.35718623096852));
#30412=CARTESIAN_POINT('Ctrl Pts',(371.211110629511,-11.7743955190035,3.36874342540923));
#30413=CARTESIAN_POINT('Ctrl Pts',(371.107912570322,-11.7805061088952,3.38028609230866));
#30414=CARTESIAN_POINT('Ctrl Pts',(371.004052530467,-11.7866166987868,3.38709706969832));
#30415=CARTESIAN_POINT('Ctrl Pts',(370.899998259857,-11.7927272886784,3.38911362256926));
#30416=CARTESIAN_POINT('Ctrl Pts',(370.796045530335,-11.7988319155668,3.39112820759235));
#30417=CARTESIAN_POINT('Ctrl Pts',(370.691899369855,-11.8049365424553,3.38835766518394));
#30418=CARTESIAN_POINT('Ctrl Pts',(370.58803226137,-11.8110411693437,3.38079110116927));
#30419=CARTESIAN_POINT('Ctrl Pts',(370.484233341735,-11.8171417885391,3.37322950461059));
#30420=CARTESIAN_POINT('Ctrl Pts',(370.380713532429,-11.8232424077346,3.36087817934067));
#30421=CARTESIAN_POINT('Ctrl Pts',(370.277944140033,-11.8293430269301,3.34377830511685));
#30422=CARTESIAN_POINT('Ctrl Pts',(370.175208956113,-11.8354416154345,3.32668412286631));
#30423=CARTESIAN_POINT('Ctrl Pts',(370.073224111271,-11.8415402039389,3.30484460356575));
#30424=CARTESIAN_POINT('Ctrl Pts',(369.972453844031,-11.8476387924433,3.27835255763599));
#30425=CARTESIAN_POINT('Ctrl Pts',(369.871691460177,-11.8537369038474,3.2518625842125));
#30426=CARTESIAN_POINT('Ctrl Pts',(369.772143875763,-11.8598350152515,3.22072091642667));
#30427=CARTESIAN_POINT('Ctrl Pts',(369.674262364553,-11.8659331266557,3.18507085097094));
#30428=CARTESIAN_POINT('Ctrl Pts',(369.576363587411,-11.8720323137438,3.14941449697693));
#30429=CARTESIAN_POINT('Ctrl Pts',(369.480131866643,-11.878131500832,3.10924831049607));
#30430=CARTESIAN_POINT('Ctrl Pts',(369.38599979111,-11.8842306879202,3.06476424108832));
#30431=CARTESIAN_POINT('Ctrl Pts',(369.291773199658,-11.8903359990662,3.02023550621803));
#30432=CARTESIAN_POINT('Ctrl Pts',(369.199650847426,-11.8964413102121,2.97138041394359));
#30433=CARTESIAN_POINT('Ctrl Pts',(369.110041870335,-11.9025466213581,2.91843749244896));
#30434=CARTESIAN_POINT('Ctrl Pts',(369.02038299778,-11.9086553320221,2.86546509163551));
#30435=CARTESIAN_POINT('Ctrl Pts',(368.933240643547,-11.914764042686,2.80840056001482));
#30436=CARTESIAN_POINT('Ctrl Pts',(368.848994454445,-11.92087275335,2.74752544387843));
#30437=CARTESIAN_POINT('Ctrl Pts',(368.764623093409,-11.9269905402598,2.68655988025695));
#30438=CARTESIAN_POINT('Ctrl Pts',(368.683156823088,-11.9331083271695,2.62177268999682));
#30439=CARTESIAN_POINT('Ctrl Pts',(368.60494178693,-11.9392261140793,2.55348534703728));
#30440=CARTESIAN_POINT('Ctrl Pts',(368.563511155485,-11.9424667157227,2.51731343077369));
#30441=CARTESIAN_POINT('Ctrl Pts',(368.522992146512,-11.9457073173661,2.48016005265332));
#30442=CARTESIAN_POINT('Ctrl Pts',(368.483431780173,-11.9489479190095,2.44207693040921));
#30443=CARTESIAN_POINT('Ctrl Pts',(368.409809033748,-11.9549787527741,2.3712033690256));
#30444=CARTESIAN_POINT('Ctrl Pts',(368.339260858662,-11.9610095865388,2.29686894666904));
#30445=CARTESIAN_POINT('Ctrl Pts',(368.272134796697,-11.9670404203034,2.21937447208579));
#30446=CARTESIAN_POINT('Ctrl Pts',(368.205109404078,-11.9730622095916,2.14199621641739));
#30447=CARTESIAN_POINT('Ctrl Pts',(368.141496201636,-11.9790839988797,2.06146766348274));
#30448=CARTESIAN_POINT('Ctrl Pts',(368.081607009118,-11.9851057881678,1.97812741532029));
#30449=CARTESIAN_POINT('Ctrl Pts',(368.021768662514,-11.9911224649579,1.89485792301379));
#30450=CARTESIAN_POINT('Ctrl Pts',(367.965648301211,-11.997139141748,1.80878183074363));
#30451=CARTESIAN_POINT('Ctrl Pts',(367.913518094768,-12.0031558185381,1.72027144180929));
#30452=CARTESIAN_POINT('Ctrl Pts',(367.861417856758,-12.0091690364819,1.63181193542088));
#30453=CARTESIAN_POINT('Ctrl Pts',(367.813303438478,-12.0151822544257,1.54092128970282));
#30454=CARTESIAN_POINT('Ctrl Pts',(367.769403602583,-12.0211954723694,1.44800058657285));
#30455=CARTESIAN_POINT('Ctrl Pts',(367.725516971768,-12.0272068815359,1.35510783401123));
#30456=CARTESIAN_POINT('Ctrl Pts',(367.685842590214,-12.0332182907024,1.26018663443941));
#30457=CARTESIAN_POINT('Ctrl Pts',(367.65056268499,-12.0392296998688,1.16366150200399));
#30458=CARTESIAN_POINT('Ctrl Pts',(367.615268449658,-12.0452435507693,1.06709716267199));
#30459=CARTESIAN_POINT('Ctrl Pts',(367.584372414241,-12.0512574016698,0.968927999078147));
#30460=CARTESIAN_POINT('Ctrl Pts',(367.55800797976,-12.0572712525702,0.869596846557717));
#30461=CARTESIAN_POINT('Ctrl Pts',(367.531638896956,-12.063286163775,0.770248180925193));
#30462=CARTESIAN_POINT('Ctrl Pts',(367.509803106472,-12.0693010749797,0.669737546039836));
#30463=CARTESIAN_POINT('Ctrl Pts',(367.492583177307,-12.0753159861844,0.568519496830185));
#30464=CARTESIAN_POINT('Ctrl Pts',(367.475343572843,-12.0813377699597,0.467185797005666));
#30465=CARTESIAN_POINT('Ctrl Pts',(367.462730425957,-12.0873595537349,0.365143503568449));
#30466=CARTESIAN_POINT('Ctrl Pts',(367.454774543377,-12.0933813375101,0.262853722376045));
#30467=CARTESIAN_POINT('Ctrl Pts',(367.447904009737,-12.098581623912,0.174518408781142));
#30468=CARTESIAN_POINT('Ctrl Pts',(367.444505879605,-12.1037819103139,0.0859987702498958));
#30469=CARTESIAN_POINT('Ctrl Pts',(367.444568709247,-12.1089821967158,-0.00240902652174046));
#30470=CARTESIAN_POINT('Ctrl Pts',(367.444568709248,-12.1089821967504,-0.00240902711028121));
#30471=CARTESIAN_POINT('Ctrl Pts',(367.444679279279,-12.1181338593118,-0.157992443353066));
#30472=CARTESIAN_POINT('Ctrl Pts',(367.455504799377,-12.1272855218732,-0.313184958602908));
#30473=CARTESIAN_POINT('Ctrl Pts',(367.476864661899,-12.1364371844346,-0.466811664981343));
#30474=CARTESIAN_POINT('Ctrl Pts',(367.481079824371,-12.1382431766102,-0.497128411017277));
#30475=CARTESIAN_POINT('Ctrl Pts',(367.485705090691,-12.1400491687858,-0.527384267298463));
#30476=CARTESIAN_POINT('Ctrl Pts',(367.490738871252,-12.1418551609614,-0.557570312889645));
#30477=CARTESIAN_POINT('Ctrl Pts',(367.507790544157,-12.1479728666244,-0.659823990703624));
#30478=CARTESIAN_POINT('Ctrl Pts',(367.529564114787,-12.1540905722874,-0.761456326808137));
#30479=CARTESIAN_POINT('Ctrl Pts',(367.556001056195,-12.1602082779504,-0.862000023675843));
#30480=CARTESIAN_POINT('Ctrl Pts',(367.582404705976,-12.1663182796823,-0.962417107436716));
#30481=CARTESIAN_POINT('Ctrl Pts',(367.613459942336,-12.1724282814141,-1.06174786995216));
#30482=CARTESIAN_POINT('Ctrl Pts',(367.649056907049,-12.1785382831459,-1.15953342654357));
#30483=CARTESIAN_POINT('Ctrl Pts',(367.684619060071,-12.1846423096636,-1.2572233547437));
#30484=CARTESIAN_POINT('Ctrl Pts',(367.72471396307,-12.1907463361814,-1.3533706849762));
#30485=CARTESIAN_POINT('Ctrl Pts',(367.769181689171,-12.1968503626991,-1.4475307797468));
#30486=CARTESIAN_POINT('Ctrl Pts',(367.813620105697,-12.2029503659299,-1.54162881170132));
#30487=CARTESIAN_POINT('Ctrl Pts',(367.862425431984,-12.2090503691608,-1.63374182994585));
#30488=CARTESIAN_POINT('Ctrl Pts',(367.915389583341,-12.2151503723916,-1.72344504344643));
#30489=CARTESIAN_POINT('Ctrl Pts',(367.968336021748,-12.221248335581,-1.81311825724637));
#30490=CARTESIAN_POINT('Ctrl Pts',(368.02543830442,-12.2273462987704,-1.9003829028048));
#30491=CARTESIAN_POINT('Ctrl Pts',(368.086442723697,-12.2334442619598,-1.98483937260049));
#30492=CARTESIAN_POINT('Ctrl Pts',(368.14744228475,-12.2395417395243,-2.06928911651609));
#30493=CARTESIAN_POINT('Ctrl Pts',(368.212343115232,-12.2456392170888,-2.15093078515682));
#30494=CARTESIAN_POINT('Ctrl Pts',(368.280849075954,-12.2517366946532,-2.22939504485151));
#30495=CARTESIAN_POINT('Ctrl Pts',(368.349367035554,-12.2578352401961,-2.30787304762822));
#30496=CARTESIAN_POINT('Ctrl Pts',(368.421491100579,-12.2639337857389,-2.38317221552238));
#30497=CARTESIAN_POINT('Ctrl Pts',(368.49688647126,-12.2700323312818,-2.45495816606099));
#30498=CARTESIAN_POINT('Ctrl Pts',(368.572357455551,-12.276136993023,-2.52681611034187));
#30499=CARTESIAN_POINT('Ctrl Pts',(368.651105987684,-12.2822416547643,-2.59515350894791));
#30500=CARTESIAN_POINT('Ctrl Pts',(368.732762260525,-12.2883463165056,-2.65967463297596));
#30501=CARTESIAN_POINT('Ctrl Pts',(368.814463934897,-12.2944543724868,-2.72423163125671));
#30502=CARTESIAN_POINT('Ctrl Pts',(368.899076225481,-12.300562428468,-2.78496788031011));
#30503=CARTESIAN_POINT('Ctrl Pts',(368.986199813889,-12.3066704844492,-2.84163065425215));
#30504=CARTESIAN_POINT('Ctrl Pts',(369.073452832902,-12.3127876145445,-2.89837760628197));
#30505=CARTESIAN_POINT('Ctrl Pts',(369.163224233733,-12.3189047446398,-2.95103878339532));
#30506=CARTESIAN_POINT('Ctrl Pts',(369.255089516233,-12.325021874735,-2.99940709510121));
#30507=CARTESIAN_POINT('Ctrl Pts',(369.303849656955,-12.3282687174611,-3.02507996760658));
#30508=CARTESIAN_POINT('Ctrl Pts',(369.353199339037,-12.3315155601872,-3.04954423421724));
#30509=CARTESIAN_POINT('Ctrl Pts',(369.403072991065,-12.3347624029133,-3.07277451288639));
#30510=CARTESIAN_POINT('Ctrl Pts',(369.497044704206,-12.3408800895246,-3.1165449005463));
#30511=CARTESIAN_POINT('Ctrl Pts',(369.593174606421,-12.3469977761359,-3.15606977135722));
#30512=CARTESIAN_POINT('Ctrl Pts',(369.691044219909,-12.3531154627471,-3.19113309999219));
#30513=CARTESIAN_POINT('Ctrl Pts',(369.788790599952,-12.3592254462158,-3.22615227830726));
#30514=CARTESIAN_POINT('Ctrl Pts',(369.888271938434,-12.3653354296845,-3.25672094264121));
#30515=CARTESIAN_POINT('Ctrl Pts',(369.989047663817,-12.3714454131532,-3.2826701584837));
#30516=CARTESIAN_POINT('Ctrl Pts',(370.08972484969,-12.3775494222191,-3.30859400092413));
#30517=CARTESIAN_POINT('Ctrl Pts',(370.191693495577,-12.383653431285,-3.32990727304869));
#30518=CARTESIAN_POINT('Ctrl Pts',(370.294496461912,-12.389757440351,-3.3464903896444));
#30519=CARTESIAN_POINT('Ctrl Pts',(370.397231690275,-12.3958574274201,-3.36306257944745));
#30520=CARTESIAN_POINT('Ctrl Pts',(370.500799727228,-12.4019574144892,-3.37491074498608));
#30521=CARTESIAN_POINT('Ctrl Pts',(370.604732563532,-12.4080574015584,-3.38196624129472));
#30522=CARTESIAN_POINT('Ctrl Pts',(370.708630654981,-12.4141553493955,-3.38901937894357));
#30523=CARTESIAN_POINT('Ctrl Pts',(370.812892879723,-12.4202532972326,-3.39128300367998));
#30524=CARTESIAN_POINT('Ctrl Pts',(370.917046194091,-12.4263512450696,-3.38874033884531));
#30525=CARTESIAN_POINT('Ctrl Pts',(371.021191228166,-12.4324487081138,-3.38619787615503));
#30526=CARTESIAN_POINT('Ctrl Pts',(371.125226944248,-12.4385461711579,-3.37884989457313));
#30527=CARTESIAN_POINT('Ctrl Pts',(371.228681267264,-12.4446436342021,-3.36673173272935));
#30528=CARTESIAN_POINT('Ctrl Pts',(371.332153724948,-12.45074216608,-3.35461144667422));
#30529=CARTESIAN_POINT('Ctrl Pts',(371.435044164988,-12.4568406979578,-3.33771936831974));
#30530=CARTESIAN_POINT('Ctrl Pts',(371.536887471093,-12.4629392298357,-3.31614248706946));
#30531=CARTESIAN_POINT('Ctrl Pts',(371.638832938744,-12.4690438793022,-3.29454396151456));
#30532=CARTESIAN_POINT('Ctrl Pts',(371.739728758831,-12.4751485287686,-3.26825133832305));
#30533=CARTESIAN_POINT('Ctrl Pts',(371.839121893272,-12.481253178235,-3.2374023388518));
#30534=CARTESIAN_POINT('Ctrl Pts',(371.938570303792,-12.4873612227155,-3.2065361831479));
#30535=CARTESIAN_POINT('Ctrl Pts',(372.036513964408,-12.493469267196,-3.17110874785328));
#30536=CARTESIAN_POINT('Ctrl Pts',(372.132518610855,-12.4995773116765,-3.13130641352555));
#30537=CARTESIAN_POINT('Ctrl Pts',(372.228665902626,-12.5056944315925,-3.09144494021768));
#30538=CARTESIAN_POINT('Ctrl Pts',(372.322868042418,-12.5118115515086,-3.047195767398));
#30539=CARTESIAN_POINT('Ctrl Pts',(372.41471415927,-12.5179286714247,-2.9987918531196));
#30540=CARTESIAN_POINT('Ctrl Pts',(372.463466436875,-12.5211756625715,-2.97309886633938));
#30541=CARTESIAN_POINT('Ctrl Pts',(372.511555359975,-12.5244226537184,-2.94623602231471));
#30542=CARTESIAN_POINT('Ctrl Pts',(372.558922902766,-12.5276696448653,-2.91824304772476));
#30543=CARTESIAN_POINT('Ctrl Pts',(372.648167311643,-12.5337872475201,-2.8655019443706));
#30544=CARTESIAN_POINT('Ctrl Pts',(372.735131232971,-12.5399048501749,-2.80857991414978));
#30545=CARTESIAN_POINT('Ctrl Pts',(372.819399833067,-12.5460224528297,-2.74769987367639));
#30546=CARTESIAN_POINT('Ctrl Pts',(372.903562301904,-12.5521323507301,-2.68689650797124));
#30547=CARTESIAN_POINT('Ctrl Pts',(372.985035857425,-12.5582422486304,-2.62214529098456));
#30548=CARTESIAN_POINT('Ctrl Pts',(373.063432003934,-12.5643521465307,-2.55371399448042));
#30549=CARTESIAN_POINT('Ctrl Pts',(373.141751473892,-12.5704560685519,-2.48534962825292));
#30550=CARTESIAN_POINT('Ctrl Pts',(373.216999202493,-12.576559990573,-2.41331261936389));
#30551=CARTESIAN_POINT('Ctrl Pts',(373.288818020092,-12.5826639125942,-2.33791231515347));
#30552=CARTESIAN_POINT('Ctrl Pts',(373.360589493313,-12.5887638107899,-2.26256171630684));
#30553=CARTESIAN_POINT('Ctrl Pts',(373.428936258777,-12.5948637089857,-2.18385253869375));
#30554=CARTESIAN_POINT('Ctrl Pts',(373.493537008161,-12.6009636071814,-2.1021319055941));
#30555=CARTESIAN_POINT('Ctrl Pts',(373.558116149598,-12.607061465056,-2.02043860677535));
#30556=CARTESIAN_POINT('Ctrl Pts',(373.618951502498,-12.6131593229306,-1.93573618799773));
#30557=CARTESIAN_POINT('Ctrl Pts',(373.675761685678,-12.6192571808052,-1.84840526116668));
#30558=CARTESIAN_POINT('Ctrl Pts',(373.732567343268,-12.6253545529148,-1.76108129125671));
#30559=CARTESIAN_POINT('Ctrl Pts',(373.785348237423,-12.6314519250243,-1.67112958618058));
#30560=CARTESIAN_POINT('Ctrl Pts',(373.833866513226,-12.6375492971338,-1.5789594354455));
#30561=CARTESIAN_POINT('Ctrl Pts',(373.882393287187,-12.643647737221,-1.48677314076177));
#30562=CARTESIAN_POINT('Ctrl Pts',(373.926655761318,-12.6497461773082,-1.39236800438883));
#30563=CARTESIAN_POINT('Ctrl Pts',(373.966462612032,-12.6558446173954,-1.29617679055429));
#30564=CARTESIAN_POINT('Ctrl Pts',(374.00630938966,-12.6619491743166,-1.19988909537721));
#30565=CARTESIAN_POINT('Ctrl Pts',(374.04169145814,-12.6680537312378,-1.10181213916787));
#30566=CARTESIAN_POINT('Ctrl Pts',(374.072466163087,-12.674158288159,-1.00239741910693));
#30567=CARTESIAN_POINT('Ctrl Pts',(374.10325798046,-12.680266239549,-0.902927419002685));
#30568=CARTESIAN_POINT('Ctrl Pts',(374.129437223958,-12.6863741909391,-0.802118584415533));
#30569=CARTESIAN_POINT('Ctrl Pts',(374.150911986072,-12.6924821423291,-0.700434451222036));
#30570=CARTESIAN_POINT('Ctrl Pts',(374.172418656284,-12.6985991691683,-0.598599231499183));
#30571=CARTESIAN_POINT('Ctrl Pts',(374.189206817382,-12.7047161960074,-0.495886535152319));
#30572=CARTESIAN_POINT('Ctrl Pts',(374.201236204739,-12.7108332228466,-0.392766949641725));
#30573=CARTESIAN_POINT('Ctrl Pts',(374.207623311376,-12.7140811108368,-0.338014719164696));
#30574=CARTESIAN_POINT('Ctrl Pts',(374.212669720767,-12.717328998827,-0.283147824870211));
#30575=CARTESIAN_POINT('Ctrl Pts',(374.216375377086,-12.7205768868171,-0.228236648652391));
#30576=CARTESIAN_POINT('Ctrl Pts',(374.223355268854,-12.7266945363493,-0.124807179250421));
#30577=CARTESIAN_POINT('Ctrl Pts',(374.225597296935,-12.7328121858815,-0.0208937739322935));
#30578=CARTESIAN_POINT('Ctrl Pts',(374.223050682688,-12.7389298354137,0.0830353720467266));
#30579=CARTESIAN_POINT('Ctrl Pts',(374.220507275439,-12.7450397808774,0.186833638140619));
#30580=CARTESIAN_POINT('Ctrl Pts',(374.213187227127,-12.751149726341,0.290647183804213));
#30581=CARTESIAN_POINT('Ctrl Pts',(374.201091647165,-12.7572596718046,0.394004166137646));
#30582=CARTESIAN_POINT('Ctrl Pts',(374.189007896168,-12.7633636420002,0.497260069718577));
#30583=CARTESIAN_POINT('Ctrl Pts',(374.172157951284,-12.7694676121959,0.600059877867714));
#30584=CARTESIAN_POINT('Ctrl Pts',(374.150594926402,-12.7755715823916,0.701934068423815));
#30585=CARTESIAN_POINT('Ctrl Pts',(374.129046113696,-12.7816715294642,0.80374111376403));
#30586=CARTESIAN_POINT('Ctrl Pts',(374.102790486939,-12.7877714765369,0.904623340137016));
#30587=CARTESIAN_POINT('Ctrl Pts',(374.071932595962,-12.7938714236096,1.00411943517842));
#30588=CARTESIAN_POINT('Ctrl Pts',(374.041085024312,-12.7999693307716,1.10358225728431));
#30589=CARTESIAN_POINT('Ctrl Pts',(374.005638373792,-12.8060672379336,1.20165946400976));
#30590=CARTESIAN_POINT('Ctrl Pts',(373.965747393962,-12.8121651450956,1.2979037305952));
#30591=CARTESIAN_POINT('Ctrl Pts',(373.925859589626,-12.8182625668379,1.39414033572181));
#30592=CARTESIAN_POINT('Ctrl Pts',(373.881528322661,-12.8243599885802,1.48854389844459));
#30593=CARTESIAN_POINT('Ctrl Pts',(373.832956610308,-12.8304574103225,1.5806867706829));
#30594=CARTESIAN_POINT('Ctrl Pts',(373.784376388271,-12.8365559003231,1.67284578620112));
#30595=CARTESIAN_POINT('Ctrl Pts',(373.731554442832,-12.8426543903237,1.76274294830886));
#30596=CARTESIAN_POINT('Ctrl Pts',(373.674739467748,-12.8487528803243,1.84997570639374));
#30597=CARTESIAN_POINT('Ctrl Pts',(373.617867505614,-12.8548574872851,1.9372959614356));
#30598=CARTESIAN_POINT('Ctrl Pts',(373.556994749451,-12.860962094246,2.02194611991554));
#30599=CARTESIAN_POINT('Ctrl Pts',(373.49241286819,-12.8670667012068,2.10355317354001));
#30600=CARTESIAN_POINT('Ctrl Pts',(373.427795074727,-12.8731747027713,2.18520560659621));
#30601=CARTESIAN_POINT('Ctrl Pts',(373.359464326172,-12.8792827043357,2.26381124322872));
#30602=CARTESIAN_POINT('Ctrl Pts',(373.287750921077,-12.8853907059001,2.33903211693762));
#30603=CARTESIAN_POINT('Ctrl Pts',(373.215930965116,-12.8915077826556,2.41436475286438));
#30604=CARTESIAN_POINT('Ctrl Pts',(373.14071862285,-12.8976248594111,2.48630228933271));
#30605=CARTESIAN_POINT('Ctrl Pts',(373.062479216396,-12.9037419361666,2.5545453611489));
#30606=CARTESIAN_POINT('Ctrl Pts',(373.020943942972,-12.9069893337008,2.59077383955402));
#30607=CARTESIAN_POINT('Ctrl Pts',(372.978556096282,-12.9102367312349,2.62596181878191));
#30608=CARTESIAN_POINT('Ctrl Pts',(372.935373661073,-12.9134841287691,2.66006946428179));
#30609=CARTESIAN_POINT('Ctrl Pts',(372.854036840211,-12.9196008053813,2.72431335045043));
#30610=CARTESIAN_POINT('Ctrl Pts',(372.769622249332,-12.9257174819936,2.78492482186272));
#30611=CARTESIAN_POINT('Ctrl Pts',(372.682487112647,-12.9318341586059,2.84159734146523));
#30612=CARTESIAN_POINT('Ctrl Pts',(372.595448309454,-12.9379440728391,2.89820720595616));
#30613=CARTESIAN_POINT('Ctrl Pts',(372.505695289837,-12.9440539870724,2.9508865411481));
#30614=CARTESIAN_POINT('Ctrl Pts',(372.413617795613,-12.9501639013057,2.9993693928008));
#30615=CARTESIAN_POINT('Ctrl Pts',(372.321635227428,-12.9562675166061,3.04780226171774));
#30616=CARTESIAN_POINT('Ctrl Pts',(372.227333326346,-12.9623711319065,3.09204705697198));
#30617=CARTESIAN_POINT('Ctrl Pts',(372.131129266487,-12.9684747472069,3.131882057315));
#30618=CARTESIAN_POINT('Ctrl Pts',(372.091932655392,-12.9709615553057,3.14811211058583));
#30619=CARTESIAN_POINT('Ctrl Pts',(372.05242058511,-12.9734483634045,3.1636106553068));
#30620=CARTESIAN_POINT('Ctrl Pts',(372.012622422842,-12.9759351715034,3.17836489467751));
#30621=CARTESIAN_POINT('',(367.444567879036,-11.766017803207,-0.000418324226323652));
#30622=CARTESIAN_POINT('Ctrl Pts',(372.012622420937,-12.6303878084336,3.17836489538373));
#30623=CARTESIAN_POINT('Ctrl Pts',(372.024541985714,-12.6296579468698,3.1739459950733));
#30624=CARTESIAN_POINT('Ctrl Pts',(372.036437143336,-12.6289300869064,3.16945987625657));
#30625=CARTESIAN_POINT('Ctrl Pts',(372.144170050708,-12.6223418396811,3.12813587321469));
#30626=CARTESIAN_POINT('Ctrl Pts',(372.238317516829,-12.6166147135911,3.08702677986565));
#30627=CARTESIAN_POINT('Ctrl Pts',(372.587203778726,-12.5952877562432,2.91541792870016));
#30628=CARTESIAN_POINT('Ctrl Pts',(372.826901990794,-12.5805117446766,2.75714699729164));
#30629=CARTESIAN_POINT('Ctrl Pts',(373.100889355238,-12.5605982380091,2.52164899902446));
#30630=CARTESIAN_POINT('Ctrl Pts',(373.156267313735,-12.5563838383691,2.47075073252989));
#30631=CARTESIAN_POINT('Ctrl Pts',(373.239129564653,-12.5496953357588,2.38934391166878));
#30632=CARTESIAN_POINT('Ctrl Pts',(373.267832046144,-12.5473020891819,2.3601042932173));
#30633=CARTESIAN_POINT('Ctrl Pts',(373.329787010923,-12.5419494394304,2.29465781631356));
#30634=CARTESIAN_POINT('Ctrl Pts',(373.362794112095,-12.5389760885359,2.25823560716289));
#30635=CARTESIAN_POINT('Ctrl Pts',(373.506301568501,-12.5255427559874,2.09278850339456));
#30636=CARTESIAN_POINT('Ctrl Pts',(373.607796347794,-12.5146641112427,1.95628976816168));
#30637=CARTESIAN_POINT('Ctrl Pts',(373.815885838914,-12.4897407625858,1.62749352155561));
#30638=CARTESIAN_POINT('Ctrl Pts',(373.91490585672,-12.4757778559277,1.43125230674521));
#30639=CARTESIAN_POINT('Ctrl Pts',(374.023531232821,-12.4574762311982,1.15145790770657));
#30640=CARTESIAN_POINT('Ctrl Pts',(374.050079629289,-12.4526279127671,1.07508840826241));
#30641=CARTESIAN_POINT('Ctrl Pts',(374.094457835642,-12.4437416491078,0.931011198078606));
#30642=CARTESIAN_POINT('Ctrl Pts',(374.112969826725,-12.4396846224251,0.863560536736765));
#30643=CARTESIAN_POINT('Ctrl Pts',(374.152908152123,-12.4299585174775,0.698147772515782));
#30644=CARTESIAN_POINT('Ctrl Pts',(374.172101285132,-12.4243586756921,0.599713328662823));
#30645=CARTESIAN_POINT('Ctrl Pts',(374.226845438165,-12.403991383365,0.233059627178938));
#30646=CARTESIAN_POINT('Ctrl Pts',(374.234624679967,-12.3899568418653,-0.038246620854701));
#30647=CARTESIAN_POINT('Ctrl Pts',(374.202045271429,-12.3703371535882,-0.395810311365903));
#30648=CARTESIAN_POINT('Ctrl Pts',(374.190551283893,-12.3654156264134,-0.483682314978925));
#30649=CARTESIAN_POINT('Ctrl Pts',(374.168380716414,-12.3578739319596,-0.613418354381483));
#30650=CARTESIAN_POINT('Ctrl Pts',(374.160324201544,-12.3553719966445,-0.655697196522826));
#30651=CARTESIAN_POINT('Ctrl Pts',(374.141961403044,-12.3500942474341,-0.742987573549507));
#30652=CARTESIAN_POINT('Ctrl Pts',(374.131536247922,-12.3473137480415,-0.787963681452503));
#30653=CARTESIAN_POINT('Ctrl Pts',(374.091156387942,-12.337277161592,-0.94730280752861));
#30654=CARTESIAN_POINT('Ctrl Pts',(374.056143761887,-12.3298184305544,-1.06028923587759));
#30655=CARTESIAN_POINT('Ctrl Pts',(373.93484686775,-12.3074405468112,-1.38973066729631));
#30656=CARTESIAN_POINT('Ctrl Pts',(373.832074768309,-12.2924075616409,-1.59940737685245));
#30657=CARTESIAN_POINT('Ctrl Pts',(373.65589259147,-12.2717981328518,-1.88122611755117));
#30658=CARTESIAN_POINT('Ctrl Pts',(373.599484548662,-12.2657394971227,-1.96319935736157));
#30659=CARTESIAN_POINT('Ctrl Pts',(373.497427743177,-12.255636549475,-2.09836531919811));
#30660=CARTESIAN_POINT('Ctrl Pts',(373.453589272517,-12.2515306801244,-2.15283756022057));
#30661=CARTESIAN_POINT('Ctrl Pts',(373.35519552766,-12.2427840420527,-2.26763945555668));
#30662=CARTESIAN_POINT('Ctrl Pts',(373.300090257508,-12.2381681513635,-2.32744083769161));
#30663=CARTESIAN_POINT('Ctrl Pts',(373.178788291599,-12.2285333713003,-2.4499308197327));
#30664=CARTESIAN_POINT('Ctrl Pts',(373.112106473679,-12.2235372207244,-2.51204759948053));
#30665=CARTESIAN_POINT('Ctrl Pts',(372.890001381342,-12.2076652007979,-2.70282246159297));
#30666=CARTESIAN_POINT('Ctrl Pts',(372.725584470146,-12.1970684666635,-2.82031763257719));
#30667=CARTESIAN_POINT('Ctrl Pts',(372.462451106292,-12.1805269397434,-2.9749460007408));
#30668=CARTESIAN_POINT('Ctrl Pts',(372.370850887397,-12.1748315781369,-3.02327380487728));
#30669=CARTESIAN_POINT('Ctrl Pts',(372.235650033008,-12.1663205469626,-3.08687231732244));
#30670=CARTESIAN_POINT('Ctrl Pts',(372.193718462074,-12.1636667960863,-3.10556630893179));
#30671=CARTESIAN_POINT('Ctrl Pts',(372.1114904902,-12.1584119518731,-3.14024095276223));
#30672=CARTESIAN_POINT('Ctrl Pts',(372.071242236142,-12.1558158016115,-3.1563112459577));
#30673=CARTESIAN_POINT('Ctrl Pts',(371.945821072504,-12.1476750061479,-3.20362220617634));
#30674=CARTESIAN_POINT('Ctrl Pts',(371.859697016181,-12.142014576942,-3.23221746721734));
#30675=CARTESIAN_POINT('Ctrl Pts',(371.618405912662,-12.1261402783332,-3.30171747762077));
#30676=CARTESIAN_POINT('Ctrl Pts',(371.461319782611,-12.1157976081619,-3.33511629259839));
#30677=CARTESIAN_POINT('Ctrl Pts',(371.134604612752,-12.0947822326438,-3.38067393947525));
#30678=CARTESIAN_POINT('Ctrl Pts',(370.965214086299,-12.0841565256868,-3.39146084121734));
#30679=CARTESIAN_POINT('Ctrl Pts',(370.719315785102,-12.0692551819074,-3.38865997171175));
#30680=CARTESIAN_POINT('Ctrl Pts',(370.642968974927,-12.0646988967876,-3.38520735498392));
#30681=CARTESIAN_POINT('Ctrl Pts',(370.495560815927,-12.0560259011502,-3.373537531118));
#30682=CARTESIAN_POINT('Ctrl Pts',(370.424515094832,-12.051901961379,-3.3656462324077));
#30683=CARTESIAN_POINT('Ctrl Pts',(370.240078235639,-12.0413107443668,-3.33923266716984));
#30684=CARTESIAN_POINT('Ctrl Pts',(370.127283562862,-12.0349497918939,-3.3171827490274));
#30685=CARTESIAN_POINT('Ctrl Pts',(369.854246246075,-12.0196243835144,-3.2492439831244));
#30686=CARTESIAN_POINT('Ctrl Pts',(369.695856069102,-12.0108029022286,-3.19719143226251));
#30687=CARTESIAN_POINT('Ctrl Pts',(369.413500394245,-11.9944411268758,-3.08074379185336));
#30688=CARTESIAN_POINT('Ctrl Pts',(369.288458472916,-11.9869418276964,-3.01993661350908));
#30689=CARTESIAN_POINT('Ctrl Pts',(369.121997341835,-11.9761701922901,-2.92593498675344));
#30690=CARTESIAN_POINT('Ctrl Pts',(369.077087351888,-11.9731797615429,-2.89918564597729));
#30691=CARTESIAN_POINT('Ctrl Pts',(368.998652822822,-11.9677739784008,-2.84997640764891));
#30692=CARTESIAN_POINT('Ctrl Pts',(368.964879139731,-11.9653816962809,-2.82793741047045));
#30693=CARTESIAN_POINT('Ctrl Pts',(368.876955795875,-11.9589873337304,-2.76829981613006));
#30694=CARTESIAN_POINT('Ctrl Pts',(368.82349850278,-11.9549319488835,-2.72971692192652));
#30695=CARTESIAN_POINT('Ctrl Pts',(368.698826341713,-11.9451275722923,-2.6340846304576));
#30696=CARTESIAN_POINT('Ctrl Pts',(368.628722693403,-11.9393306095287,-2.57566968285829));
#30697=CARTESIAN_POINT('Ctrl Pts',(368.353015442919,-11.9155744517769,-2.32641447151465));
#30698=CARTESIAN_POINT('Ctrl Pts',(368.169076352201,-11.8975425384769,-2.11319710994955));
#30699=CARTESIAN_POINT('Ctrl Pts',(367.971453027551,-11.8759526132159,-1.81663412427158));
#30700=CARTESIAN_POINT('Ctrl Pts',(367.931532080886,-11.8714315729378,-1.75213887541297));
#30701=CARTESIAN_POINT('Ctrl Pts',(367.858410241795,-11.8628122266085,-1.62463566630747));
#30702=CARTESIAN_POINT('Ctrl Pts',(367.824965147646,-11.8587071669493,-1.5618144904171));
#30703=CARTESIAN_POINT('Ctrl Pts',(367.742903175331,-11.8481534707186,-1.3952346788963));
#30704=CARTESIAN_POINT('Ctrl Pts',(367.697523779782,-11.841811192184,-1.28998092952482));
#30705=CARTESIAN_POINT('Ctrl Pts',(367.588423274243,-11.824783161097,-0.996915563777684));
#30706=CARTESIAN_POINT('Ctrl Pts',(367.535707360988,-11.8143561533316,-0.805506497705102));
#30707=CARTESIAN_POINT('Ctrl Pts',(367.477924655452,-11.7970798734975,-0.489966768151784));
#30708=CARTESIAN_POINT('Ctrl Pts',(367.462399460329,-11.7903875998426,-0.368244433617266));
#30709=CARTESIAN_POINT('Ctrl Pts',(367.450168323851,-11.780803097834,-0.200122982120811));
#30710=CARTESIAN_POINT('Ctrl Pts',(367.447766301528,-11.7781515277329,-0.15422505874192));
#30711=CARTESIAN_POINT('Ctrl Pts',(367.445147143127,-11.7733336456054,-0.0722844906329021));
#30712=CARTESIAN_POINT('Ctrl Pts',(367.444570387077,-11.7711856518553,-0.036260890360518));
#30713=CARTESIAN_POINT('Ctrl Pts',(367.444567861555,-11.7690118023792,-0.000237649104901999));
#30714=CARTESIAN_POINT('Ctrl Pts',(367.444567879036,-11.766017803207,-0.000418324226323596));
#30715=CARTESIAN_POINT('Ctrl Pts',(367.444555127666,-11.7599203887752,0.102908127781684));
#30716=CARTESIAN_POINT('Ctrl Pts',(367.449271066985,-11.7538229743435,0.20640283311262));
#30717=CARTESIAN_POINT('Ctrl Pts',(367.458735803286,-11.7477255599117,0.309597943527872));
#30718=CARTESIAN_POINT('Ctrl Pts',(367.46818869345,-11.741635777051,0.412663894144712));
#30719=CARTESIAN_POINT('Ctrl Pts',(367.482378525081,-11.7355459941903,0.515430572031453));
#30720=CARTESIAN_POINT('Ctrl Pts',(367.501273385533,-11.7294562113296,0.617429865570024));
#30721=CARTESIAN_POINT('Ctrl Pts',(367.52076030823,-11.7231756077682,0.72262526266596));
#30722=CARTESIAN_POINT('Ctrl Pts',(367.545252007484,-11.7168950042068,0.827003927291572));
#30723=CARTESIAN_POINT('Ctrl Pts',(367.574655535011,-11.7106144006454,0.930057328190894));
#30724=CARTESIAN_POINT('Ctrl Pts',(367.603119667462,-11.7045344521942,1.02981833986042));
#30725=CARTESIAN_POINT('Ctrl Pts',(367.636186423178,-11.6984545037431,1.1283370346564));
#30726=CARTESIAN_POINT('Ctrl Pts',(367.673719753446,-11.692374555292,1.22516313778319));
#30727=CARTESIAN_POINT('Ctrl Pts',(367.711241689998,-11.6862964524862,1.32195984812046));
#30728=CARTESIAN_POINT('Ctrl Pts',(367.75322735116,-11.6802183496804,1.41706458906934));
#30729=CARTESIAN_POINT('Ctrl Pts',(367.79949161502,-11.6741402468746,1.51004462397916));
#30730=CARTESIAN_POINT('Ctrl Pts',(367.845753861071,-11.6680624091643,1.60302060357878));
#30731=CARTESIAN_POINT('Ctrl Pts',(367.896294147212,-11.661984571454,1.69387167827921));
#30732=CARTESIAN_POINT('Ctrl Pts',(367.950880634756,-11.6559067337438,1.78218822509042));
#30733=CARTESIAN_POINT('Ctrl Pts',(368.005478930917,-11.6498275812234,1.87052387729691));
#30734=CARTESIAN_POINT('Ctrl Pts',(368.064124942212,-11.643748428703,1.9563235480984));
#30735=CARTESIAN_POINT('Ctrl Pts',(368.126543117109,-11.6376692761826,2.03920598296474));
#30736=CARTESIAN_POINT('Ctrl Pts',(368.189023917612,-11.6315840243072,2.12217157570357));
#30737=CARTESIAN_POINT('Ctrl Pts',(368.25528417705,-11.6254987724318,2.20221374864857));
#30738=CARTESIAN_POINT('Ctrl Pts',(368.325007729987,-11.6194135205565,2.27898393322951));
#30739=CARTESIAN_POINT('Ctrl Pts',(368.394773337554,-11.6133245982855,2.35580042270546));
#30740=CARTESIAN_POINT('Ctrl Pts',(368.468006096334,-11.6072356760145,2.42934069098724));
#30741=CARTESIAN_POINT('Ctrl Pts',(368.544353964849,-11.6011467537435,2.49929399079757));
#30742=CARTESIAN_POINT('Ctrl Pts',(368.620807472042,-11.5950494065392,2.56934408144579));
#30743=CARTESIAN_POINT('Ctrl Pts',(368.700384362463,-11.5889520593348,2.63579702564753));
#30744=CARTESIAN_POINT('Ctrl Pts',(368.782700804078,-11.5828547121305,2.6983833208337));
#30745=CARTESIAN_POINT('Ctrl Pts',(368.801299751674,-11.5814770500389,2.71252435027497));
#30746=CARTESIAN_POINT('Ctrl Pts',(368.820038446072,-11.5800993879474,2.72646816341016));
#30747=CARTESIAN_POINT('Ctrl Pts',(368.838912275429,-11.5787217258558,2.74021197037831));
#30748=CARTESIAN_POINT('Ctrl Pts',(368.92268496215,-11.5726068854265,2.80121472788649));
#30749=CARTESIAN_POINT('Ctrl Pts',(369.009388754275,-11.5664920449973,2.85846789347928));
#30750=CARTESIAN_POINT('Ctrl Pts',(369.098654492841,-11.560377204568,2.911679543137));
#30751=CARTESIAN_POINT('Ctrl Pts',(369.187809743689,-11.5542699327174,2.96482533064221));
#30752=CARTESIAN_POINT('Ctrl Pts',(369.279520273,-11.5481626608668,3.01393933253664));
#30753=CARTESIAN_POINT('Ctrl Pts',(369.373386233634,-11.5420553890161,3.05877162687604));
#30754=CARTESIAN_POINT('Ctrl Pts',(369.467162497687,-11.5359539531618,3.10356108030176));
#30755=CARTESIAN_POINT('Ctrl Pts',(369.563089714454,-11.5298525173075,3.14407678110448));
#30756=CARTESIAN_POINT('Ctrl Pts',(369.660742346388,-11.5237510814532,3.18011408478605));
#30757=CARTESIAN_POINT('Ctrl Pts',(369.758334125979,-11.5176534477153,3.21612893178302));
#30758=CARTESIAN_POINT('Ctrl Pts',(369.857648784432,-11.5115558139773,3.24767078430108));
#30759=CARTESIAN_POINT('Ctrl Pts',(369.958240372104,-11.5054581802393,3.2745829214686));
#30760=CARTESIAN_POINT('Ctrl Pts',(370.058800594723,-11.4993624477796,3.3014866672727));
#30761=CARTESIAN_POINT('Ctrl Pts',(370.160636544409,-11.4932667153199,3.32376345748213));
#30762=CARTESIAN_POINT('Ctrl Pts',(370.26328743465,-11.4871709828601,3.34130652942278));
#30763=CARTESIAN_POINT('Ctrl Pts',(370.365932548757,-11.4810755934054,3.35884861422019));
#30764=CARTESIAN_POINT('Ctrl Pts',(370.469392092768,-11.4749802039507,3.37165743917901));
#30765=CARTESIAN_POINT('Ctrl Pts',(370.57319629566,-11.4688848144959,3.37967758738546));
#30766=CARTESIAN_POINT('Ctrl Pts',(370.677021182592,-11.462788210473,3.38769933368773));
#30767=CARTESIAN_POINT('Ctrl Pts',(370.781190440714,-11.4566916064502,3.39093047427338));
#30768=CARTESIAN_POINT('Ctrl Pts',(370.885231289961,-11.4505950024273,3.38936762309131));
#30769=CARTESIAN_POINT('Ctrl Pts',(370.989380563611,-11.4444920449322,3.38780314321044));
#30770=CARTESIAN_POINT('Ctrl Pts',(371.093400735166,-11.4383890874371,3.38143470324141));
#30771=CARTESIAN_POINT('Ctrl Pts',(371.196821203217,-11.4322861299419,3.37031102181144));
#30772=CARTESIAN_POINT('Ctrl Pts',(371.300301437738,-11.4261796455606,3.35918091202953));
#30773=CARTESIAN_POINT('Ctrl Pts',(371.403180858199,-11.4200731611793,3.34329015203459));
#30774=CARTESIAN_POINT('Ctrl Pts',(371.504998040673,-11.413966676798,3.32273880235326));
#30775=CARTESIAN_POINT('Ctrl Pts',(371.606970257111,-11.4078508942563,3.30215615974923));
#30776=CARTESIAN_POINT('Ctrl Pts',(371.707876593251,-11.4017351117147,3.276898859421));
#30777=CARTESIAN_POINT('Ctrl Pts',(371.807269721178,-11.3956193291731,3.24711714065645));
#30778=CARTESIAN_POINT('Ctrl Pts',(371.860385531707,-11.3923510474167,3.23120175330404));
#30779=CARTESIAN_POINT('Ctrl Pts',(371.913069505805,-11.3890827656602,3.21399509497087));
#30780=CARTESIAN_POINT('Ctrl Pts',(371.965255865135,-11.3858144839038,3.19552566500655));
#30781=CARTESIAN_POINT('Ctrl Pts',(371.981082642912,-11.384823298281,3.18992436291385));
#30782=CARTESIAN_POINT('Ctrl Pts',(371.996872144802,-11.3838321126582,3.18420394249049));
#30783=CARTESIAN_POINT('Ctrl Pts',(372.012622422842,-11.3828409270354,3.17836489467751));
#30784=CARTESIAN_POINT('Origin',(370.834317853224,-8.23961502859548,0.));
#30785=CARTESIAN_POINT('',(366.749317961181,-12.6146150285594,0.000939151365601897));
#30786=CARTESIAN_POINT('Ctrl Pts',(373.320592904309,-11.8073874696441,-3.2412437998941));
#30787=CARTESIAN_POINT('Ctrl Pts',(373.416781140934,-11.813285821701,-3.16746026872723));
#30788=CARTESIAN_POINT('Ctrl Pts',(373.509749908528,-11.8191841737578,-3.08933937017736));
#30789=CARTESIAN_POINT('Ctrl Pts',(373.599093399365,-11.8250825258147,-3.00719822749649));
#30790=CARTESIAN_POINT('Ctrl Pts',(373.687265105201,-11.8309035180056,-2.92613440738434));
#30791=CARTESIAN_POINT('Ctrl Pts',(373.77190575925,-11.8367245101966,-2.84115545631612));
#30792=CARTESIAN_POINT('Ctrl Pts',(373.852659007258,-11.8425455023875,-2.75260634269847));
#30793=CARTESIAN_POINT('Ctrl Pts',(373.933401209199,-11.8483656983371,-2.66406934152782));
#30794=CARTESIAN_POINT('Ctrl Pts',(374.010256789676,-11.8541858942867,-2.5719634488751));
#30795=CARTESIAN_POINT('Ctrl Pts',(374.082907474943,-11.8600060902364,-2.4766692289559));
#30796=CARTESIAN_POINT('Ctrl Pts',(374.155565073807,-11.8658268400484,-2.38136594063285));
#30797=CARTESIAN_POINT('Ctrl Pts',(374.224016735994,-11.8716475898605,-2.2828740443364));
#30798=CARTESIAN_POINT('Ctrl Pts',(374.287985947505,-11.8774683396725,-2.18160530219018));
#30799=CARTESIAN_POINT('Ctrl Pts',(374.35344848064,-11.8834249712839,-2.07797250397809));
#30800=CARTESIAN_POINT('Ctrl Pts',(374.414216440752,-11.8893816028953,-1.9714319762906));
#30801=CARTESIAN_POINT('Ctrl Pts',(374.470042452942,-11.8953382345067,-1.86245312290073));
#30802=CARTESIAN_POINT('Ctrl Pts',(374.524671339382,-11.901167132884,-1.75581119788089));
#30803=CARTESIAN_POINT('Ctrl Pts',(374.574567975965,-11.9069960312612,-1.64683486665082));
#30804=CARTESIAN_POINT('Ctrl Pts',(374.619549142882,-11.9128249296384,-1.53598472772121));
#30805=CARTESIAN_POINT('Ctrl Pts',(374.666008871328,-11.9188454278669,-1.42149086938519));
#30806=CARTESIAN_POINT('Ctrl Pts',(374.707224259818,-11.9248659260954,-1.30499834529334));
#30807=CARTESIAN_POINT('Ctrl Pts',(374.743049388451,-11.9308864243239,-1.18703108026663));
#30808=CARTESIAN_POINT('Ctrl Pts',(374.778874517084,-11.9369069225524,-1.0690638152399));
#30809=CARTESIAN_POINT('Ctrl Pts',(374.809309328429,-11.9429274207809,-0.949622280235242));
#30810=CARTESIAN_POINT('Ctrl Pts',(374.834266080049,-11.9489479190094,-0.829240123678208));
#30811=CARTESIAN_POINT('Ctrl Pts',(374.858468388882,-11.9547864175316,-0.712497120611384));
#30812=CARTESIAN_POINT('Ctrl Pts',(374.877592108987,-11.9606249160538,-0.594517395874913));
#30813=CARTESIAN_POINT('Ctrl Pts',(374.891516289371,-11.9664634145759,-0.475779202702064));
#30814=CARTESIAN_POINT('Ctrl Pts',(374.905423635505,-11.9722948543886,-0.357184563289714));
#30815=CARTESIAN_POINT('Ctrl Pts',(374.914143900232,-11.9781262942012,-0.237833679427054));
#30816=CARTESIAN_POINT('Ctrl Pts',(374.917606972006,-11.9839577340138,-0.118215787594323));
#30817=CARTESIAN_POINT('Ctrl Pts',(374.921066744893,-11.9897836188555,0.00128815743634286));
#30818=CARTESIAN_POINT('Ctrl Pts',(374.919279277512,-11.9956095036971,0.121058200836194));
#30819=CARTESIAN_POINT('Ctrl Pts',(374.912226234157,-12.0014353885387,0.240599743798495));
#30820=CARTESIAN_POINT('Ctrl Pts',(374.905142998665,-12.0072862123897,0.360653011199787));
#30821=CARTESIAN_POINT('Ctrl Pts',(374.892748956364,-12.0131370362406,0.480475405878789));
#30822=CARTESIAN_POINT('Ctrl Pts',(374.875078489537,-12.0189878600916,0.599565242504155));
#30823=CARTESIAN_POINT('Ctrl Pts',(374.857501492598,-12.0248077353632,0.71802514027771));
#30824=CARTESIAN_POINT('Ctrl Pts',(374.834703826155,-12.0306276106347,0.835759807168469));
#30825=CARTESIAN_POINT('Ctrl Pts',(374.806771267674,-12.0364474859063,0.952280877696166));
#30826=CARTESIAN_POINT('Ctrl Pts',(374.778842205623,-12.0422666326808,1.06878736281487));
#30827=CARTESIAN_POINT('Ctrl Pts',(374.745779624748,-12.0480857794553,1.18408015929471));
#30828=CARTESIAN_POINT('Ctrl Pts',(374.707720126321,-12.0539049262298,1.29768248457338));
#30829=CARTESIAN_POINT('Ctrl Pts',(374.669656554385,-12.0597246958277,1.41129696871103));
#30830=CARTESIAN_POINT('Ctrl Pts',(374.626595130418,-12.0655444654256,1.52322023718578));
#30831=CARTESIAN_POINT('Ctrl Pts',(374.578721698208,-12.0713642350235,1.63299260429113));
#30832=CARTESIAN_POINT('Ctrl Pts',(374.53040016091,-12.0772384788517,1.74379246313863));
#30833=CARTESIAN_POINT('Ctrl Pts',(374.477176225592,-12.0831127226798,1.85240055634729));
#30834=CARTESIAN_POINT('Ctrl Pts',(374.41928935173,-12.088986966508,1.95836777825303));
#30835=CARTESIAN_POINT('Ctrl Pts',(374.361858438797,-12.0948149403358,2.06350032193764));
#30836=CARTESIAN_POINT('Ctrl Pts',(374.299838045423,-12.1006429141637,2.16603312997207));
#30837=CARTESIAN_POINT('Ctrl Pts',(374.233506141718,-12.1064708879916,2.26555599784294));
#30838=CARTESIAN_POINT('Ctrl Pts',(374.166384295241,-12.1123682668199,2.36626407774338));
#30839=CARTESIAN_POINT('Ctrl Pts',(374.094847833739,-12.1182656456482,2.46388971553068));
#30840=CARTESIAN_POINT('Ctrl Pts',(374.019226672328,-12.1241630244765,2.55804237924118));
#30841=CARTESIAN_POINT('Ctrl Pts',(373.943605510917,-12.1300604033048,2.65219504295168));
#30842=CARTESIAN_POINT('Ctrl Pts',(373.863899971763,-12.1359577821331,2.74287445019914));
#30843=CARTESIAN_POINT('Ctrl Pts',(373.780477569685,-12.1418551609614,2.82972930244228));
#30844=CARTESIAN_POINT('Ctrl Pts',(373.697882115775,-12.1476940803532,2.91572318138476));
#30845=CARTESIAN_POINT('Ctrl Pts',(373.6113939645,-12.1535329997451,2.99822749085314));
#30846=CARTESIAN_POINT('Ctrl Pts',(373.521339213008,-12.159371919137,3.07687198499739));
#30847=CARTESIAN_POINT('Ctrl Pts',(373.431393249344,-12.1652037850048,3.15542147511918));
#30848=CARTESIAN_POINT('Ctrl Pts',(373.337889559631,-12.1710356508726,3.23012016079347));
#30849=CARTESIAN_POINT('Ctrl Pts',(373.241192047349,-12.1768675167404,3.30063351701688));
#30850=CARTESIAN_POINT('Ctrl Pts',(373.144586565468,-12.1826938322177,3.37107976321517));
#30851=CARTESIAN_POINT('Ctrl Pts',(373.044793635231,-12.188520147695,3.43734836784025));
#30852=CARTESIAN_POINT('Ctrl Pts',(372.942210860599,-12.1943464631723,3.49914447679125));
#30853=CARTESIAN_POINT('Ctrl Pts',(372.83919938364,-12.2001971273282,3.56119883705051));
#30854=CARTESIAN_POINT('Ctrl Pts',(372.733375005362,-12.2060477914841,3.61874296561396));
#30855=CARTESIAN_POINT('Ctrl Pts',(372.625170852556,-12.2118984556399,3.67152155581092));
#30856=CARTESIAN_POINT('Ctrl Pts',(372.517528002055,-12.2177187698398,3.72402636035735));
#30857=CARTESIAN_POINT('Ctrl Pts',(372.407530380524,-12.2235390840396,3.77181477977987));
#30858=CARTESIAN_POINT('Ctrl Pts',(372.295629324332,-12.2293593982395,3.81468134768921));
#30859=CARTESIAN_POINT('Ctrl Pts',(372.183742230063,-12.2351789862372,3.85754256712574));
#30860=CARTESIAN_POINT('Ctrl Pts',(372.069952552326,-12.2409985742349,3.89548301161378));
#30861=CARTESIAN_POINT('Ctrl Pts',(371.954730816777,-12.2468181622326,3.92834568121259));
#30862=CARTESIAN_POINT('Ctrl Pts',(371.839496714967,-12.2526383748221,3.96121187782273));
#30863=CARTESIAN_POINT('Ctrl Pts',(371.722830639862,-12.2584585874116,3.98899910471113));
#30864=CARTESIAN_POINT('Ctrl Pts',(371.605216865551,-12.2642788000011,4.01160064223666));
#30865=CARTESIAN_POINT('Ctrl Pts',(371.486523569872,-12.2701524335771,4.03440962861617));
#30866=CARTESIAN_POINT('Ctrl Pts',(371.366865501073,-12.2760260671531,4.05193715902417));
#30867=CARTESIAN_POINT('Ctrl Pts',(371.246748258264,-12.2818997007292,4.0641267402725));
#30868=CARTESIAN_POINT('Ctrl Pts',(371.127555703666,-12.2877281178184,4.07622248351881));
#30869=CARTESIAN_POINT('Ctrl Pts',(371.007911431417,-12.2935565349076,4.08306221230075));
#30870=CARTESIAN_POINT('Ctrl Pts',(370.888311011204,-12.2993849519968,4.08464315930915));
#30871=CARTESIAN_POINT('Ctrl Pts',(370.767318812382,-12.3052811938163,4.08624250364613));
#30872=CARTESIAN_POINT('Ctrl Pts',(370.646371920567,-12.3111774356357,4.08245991020879));
#30873=CARTESIAN_POINT('Ctrl Pts',(370.525978655253,-12.3170736774551,4.07334652822396));
#30874=CARTESIAN_POINT('Ctrl Pts',(370.405585389938,-12.3229699192745,4.06423314623914));
#30875=CARTESIAN_POINT('Ctrl Pts',(370.285746165596,-12.3288661610939,4.04978908149056));
#30876=CARTESIAN_POINT('Ctrl Pts',(370.166958227814,-12.3347624029133,4.03011862485116));
#30877=CARTESIAN_POINT('Ctrl Pts',(370.049325495705,-12.3406013041295,4.01063946223983));
#30878=CARTESIAN_POINT('Ctrl Pts',(369.932368949583,-12.3464402053458,3.98597640810493));
#30879=CARTESIAN_POINT('Ctrl Pts',(369.816578360685,-12.352279106562,3.95618899009212));
#30880=CARTESIAN_POINT('Ctrl Pts',(369.700927635187,-12.3581109549722,3.92643755228791));
#30881=CARTESIAN_POINT('Ctrl Pts',(369.586440455055,-12.3639428033823,3.89157416417475));
#30882=CARTESIAN_POINT('Ctrl Pts',(369.473598515069,-12.3697746517924,3.85170973500986));
#30883=CARTESIAN_POINT('Ctrl Pts',(369.360863956748,-12.3756009505497,3.81188324128655));
#30884=CARTESIAN_POINT('Ctrl Pts',(369.249771903986,-12.3814272493069,3.7670653101199));
#30885=CARTESIAN_POINT('Ctrl Pts',(369.140790395302,-12.3872535480642,3.7174170803481));
#30886=CARTESIAN_POINT('Ctrl Pts',(369.031353006958,-12.3931042187642,3.66756116747138));
#30887=CARTESIAN_POINT('Ctrl Pts',(368.924044259686,-12.3989548894643,3.61283455966244));
#30888=CARTESIAN_POINT('Ctrl Pts',(368.819319673422,-12.4048055601643,3.55345006091209));
#30889=CARTESIAN_POINT('Ctrl Pts',(368.715138720673,-12.4106258595754,3.49437383173733));
#30890=CARTESIAN_POINT('Ctrl Pts',(368.613515515265,-12.4164461589864,3.43068816584515));
#30891=CARTESIAN_POINT('Ctrl Pts',(368.514874767661,-12.4222664583974,3.36264907072311));
#30892=CARTESIAN_POINT('Ctrl Pts',(368.416246314658,-12.4280860323653,3.2946184560065));
#30893=CARTESIAN_POINT('Ctrl Pts',(368.32059991382,-12.4339056063331,3.22223572178511));
#30894=CARTESIAN_POINT('Ctrl Pts',(368.228331158398,-12.439725180301,3.14580011227508));
#30895=CARTESIAN_POINT('Ctrl Pts',(368.136052487785,-12.4455453796397,3.06935628900222));
#30896=CARTESIAN_POINT('Ctrl Pts',(368.047152496659,-12.4513655789783,2.98885898329061));
#30897=CARTESIAN_POINT('Ctrl Pts',(367.961993087948,-12.457185778317,2.90464721485749));
#30898=CARTESIAN_POINT('Ctrl Pts',(367.87605152407,-12.4630594338627,2.81966199495578));
#30899=CARTESIAN_POINT('Ctrl Pts',(367.793919909523,-12.4689330894084,2.73089402274613));
#30900=CARTESIAN_POINT('Ctrl Pts',(367.715930792127,-12.4748067449541,2.63872831818381));
#30901=CARTESIAN_POINT('Ctrl Pts',(367.638542489789,-12.4806351508442,2.54727264272517));
#30902=CARTESIAN_POINT('Ctrl Pts',(367.565233284147,-12.4864635567344,2.45247176293892));
#30903=CARTESIAN_POINT('Ctrl Pts',(367.49628573707,-12.4922919626245,2.35473280682202));
#30904=CARTESIAN_POINT('Ctrl Pts',(367.426535263906,-12.498188242998,2.25585563533917));
#30905=CARTESIAN_POINT('Ctrl Pts',(367.361248913144,-12.5040845233714,2.153971882455));
#30906=CARTESIAN_POINT('Ctrl Pts',(367.300671998537,-12.5099808037449,2.04952969572403));
#30907=CARTESIAN_POINT('Ctrl Pts',(367.24009508393,-12.5158770841183,1.94508750899306));
#30908=CARTESIAN_POINT('Ctrl Pts',(367.184227752654,-12.5217733644918,1.83808729008043));
#30909=CARTESIAN_POINT('Ctrl Pts',(367.133265227715,-12.5276696448652,1.72899810966225));
#30910=CARTESIAN_POINT('Ctrl Pts',(367.079121526908,-12.533933982058,1.61309937911611));
#30911=CARTESIAN_POINT('Ctrl Pts',(367.030369879211,-12.5401983192508,1.49453584255141));
#30912=CARTESIAN_POINT('Ctrl Pts',(366.987258854716,-12.5464626564436,1.37381296470686));
#30913=CARTESIAN_POINT('Ctrl Pts',(366.944274342146,-12.5527086105576,1.25344435549594));
#30914=CARTESIAN_POINT('Ctrl Pts',(366.906897545925,-12.5589545646716,1.13092933426704));
#30915=CARTESIAN_POINT('Ctrl Pts',(366.875328960634,-12.5652005187856,1.00679290241326));
#30916=CARTESIAN_POINT('Ctrl Pts',(366.843818211393,-12.5714350298365,0.882883897947502));
#30917=CARTESIAN_POINT('Ctrl Pts',(366.818094544775,-12.5776695408873,0.757359701769412));
#30918=CARTESIAN_POINT('Ctrl Pts',(366.798309421592,-12.5839040519381,0.630762189572842));
#30919=CARTESIAN_POINT('Ctrl Pts',(366.778578298236,-12.5901215470465,0.504510201823112));
#30920=CARTESIAN_POINT('Ctrl Pts',(366.764753447751,-12.5963390421549,0.377191045207156));
#30921=CARTESIAN_POINT('Ctrl Pts',(366.75693562444,-12.6025565372633,0.249357495166076));
#30922=CARTESIAN_POINT('Ctrl Pts',(366.751881544369,-12.606576034362,0.166715438429602));
#30923=CARTESIAN_POINT('Ctrl Pts',(366.749337024585,-12.6105955314607,0.0838586970475943));
#30924=CARTESIAN_POINT('Ctrl Pts',(366.749317961181,-12.6146150285594,0.000939151365612782));
#30925=CARTESIAN_POINT('Ctrl Pts',(366.74931796118,-12.6146150285955,0.00093915062137102));
#30926=CARTESIAN_POINT('Ctrl Pts',(366.749289612733,-12.6205922712843,-0.122367381518829));
#30927=CARTESIAN_POINT('Ctrl Pts',(366.754848656197,-12.6265695139731,-0.245621759676924));
#30928=CARTESIAN_POINT('Ctrl Pts',(366.76595478391,-12.6325467566619,-0.368302777942603));
#30929=CARTESIAN_POINT('Ctrl Pts',(366.777068607145,-12.6385281410287,-0.491068802841755));
#30930=CARTESIAN_POINT('Ctrl Pts',(366.79373714086,-12.6445095253955,-0.613260304939521));
#30931=CARTESIAN_POINT('Ctrl Pts',(366.815868431614,-12.6504909097623,-0.734363156729659));
#30932=CARTESIAN_POINT('Ctrl Pts',(366.83803627101,-12.6564821720652,-0.855666003395637));
#30933=CARTESIAN_POINT('Ctrl Pts',(366.865684827507,-12.662473434368,-0.97587623954742));
#30934=CARTESIAN_POINT('Ctrl Pts',(366.898671177634,-12.6684646966709,-1.09449086104898));
#30935=CARTESIAN_POINT('Ctrl Pts',(366.931685318874,-12.6744610066327,-1.21320541577318));
#30936=CARTESIAN_POINT('Ctrl Pts',(366.970046106514,-12.6804573165944,-1.33032132056031));
#30937=CARTESIAN_POINT('Ctrl Pts',(367.013561534935,-12.6864536265562,-1.44535329807331));
#30938=CARTESIAN_POINT('Ctrl Pts',(367.057161999254,-12.6924616542379,-1.56061006591746));
#30939=CARTESIAN_POINT('Ctrl Pts',(367.105937094125,-12.6984696819197,-1.67377442208256));
#30940=CARTESIAN_POINT('Ctrl Pts',(367.159647196542,-12.7044777096014,-1.78438240434055));
#30941=CARTESIAN_POINT('Ctrl Pts',(367.20762125741,-12.7098441020066,-1.88317786058538));
#30942=CARTESIAN_POINT('Ctrl Pts',(367.259531793322,-12.7152104944119,-1.9799339922456));
#30943=CARTESIAN_POINT('Ctrl Pts',(367.315178694938,-12.7205768868172,-2.07433955383816));
#30944=CARTESIAN_POINT('Ctrl Pts',(367.375724918107,-12.7264157526434,-2.17705686665494));
#30945=CARTESIAN_POINT('Ctrl Pts',(367.440863361581,-12.7322546184696,-2.27727604182428));
#30946=CARTESIAN_POINT('Ctrl Pts',(367.510362071704,-12.7380934842958,-2.37456163586078));
#30947=CARTESIAN_POINT('Ctrl Pts',(367.579776823804,-12.7439252964713,-2.47172970388697));
#30948=CARTESIAN_POINT('Ctrl Pts',(367.653541130018,-12.7497571086467,-2.5659709132208));
#30949=CARTESIAN_POINT('Ctrl Pts',(367.73137801369,-12.7555889208222,-2.65687586315837));
#30950=CARTESIAN_POINT('Ctrl Pts',(367.809140815875,-12.7614151825529,-2.7476942940379));
#30951=CARTESIAN_POINT('Ctrl Pts',(367.89096822068,-12.7672414442837,-2.83518247686381));
#30952=CARTESIAN_POINT('Ctrl Pts',(367.976541313123,-12.7730677060145,-2.918961844021));
#30953=CARTESIAN_POINT('Ctrl Pts',(368.062473111248,-12.7789183902959,-3.00309239791412));
#30954=CARTESIAN_POINT('Ctrl Pts',(368.152181827448,-12.7847690745773,-3.08348263761303));
#30955=CARTESIAN_POINT('Ctrl Pts',(368.245304849742,-12.7906197588588,-3.15978427551634));
#30956=CARTESIAN_POINT('Ctrl Pts',(368.337943631764,-12.796440019547,-3.23568914444657));
#30957=CARTESIAN_POINT('Ctrl Pts',(368.433960972766,-12.8022602802352,-3.30754757947248));
#30958=CARTESIAN_POINT('Ctrl Pts',(368.532965065346,-12.8080805409234,-3.37505560631587));
#30959=CARTESIAN_POINT('Ctrl Pts',(368.631956808287,-12.8139000756001,-3.4425552122984));
#30960=CARTESIAN_POINT('Ctrl Pts',(368.733934226552,-12.8197196102768,-3.50570526114235));
#30961=CARTESIAN_POINT('Ctrl Pts',(368.838475667358,-12.8255391449535,-3.56424451589903));
#30962=CARTESIAN_POINT('Ctrl Pts',(368.943028332845,-12.8313593044774,-3.62279005605317));
#30963=CARTESIAN_POINT('Ctrl Pts',(369.050145214291,-12.8371794640013,-3.6767236195874));
#30964=CARTESIAN_POINT('Ctrl Pts',(369.159379689806,-12.8429996235251,-3.72582972621208));
#30965=CARTESIAN_POINT('Ctrl Pts',(369.269619193418,-12.8488733322955,-3.77538764090064));
#30966=CARTESIAN_POINT('Ctrl Pts',(369.382015076121,-12.8547470410658,-3.82002863338509));
#30967=CARTESIAN_POINT('Ctrl Pts',(369.496088355519,-12.8606207498361,-3.85958117047339));
#30968=CARTESIAN_POINT('Ctrl Pts',(369.609281016511,-12.866449114981,-3.89882837144481));
#30969=CARTESIAN_POINT('Ctrl Pts',(369.72412485796,-12.8722774801259,-3.93306534577048));
#30970=CARTESIAN_POINT('Ctrl Pts',(369.840138302784,-12.8781058452708,-3.96217516289817));
#30971=CARTESIAN_POINT('Ctrl Pts',(369.957505592998,-12.8840022258538,-3.99162468368515));
#30972=CARTESIAN_POINT('Ctrl Pts',(370.076069538853,-12.8898986064369,-4.01582653432596));
#30973=CARTESIAN_POINT('Ctrl Pts',(370.195323679133,-12.8957949870199,-4.03471330400041));
#30974=CARTESIAN_POINT('Ctrl Pts',(370.314577819413,-12.901691367603,-4.05360007367485));
#30975=CARTESIAN_POINT('Ctrl Pts',(370.434521726344,-12.907587748186,-4.06717176978063));
#30976=CARTESIAN_POINT('Ctrl Pts',(370.554647464531,-12.9134841287691,-4.0754152516876));
#30977=CARTESIAN_POINT('Ctrl Pts',(370.676637201473,-12.9194720038664,-4.08378664823011));
#30978=CARTESIAN_POINT('Ctrl Pts',(370.79919182361,-12.9254598789638,-4.08668894203072));
#30979=CARTESIAN_POINT('Ctrl Pts',(370.921782419112,-12.9314477540612,-4.08406353399574));
#30980=CARTESIAN_POINT('Ctrl Pts',(371.041157801345,-12.9372785837067,-4.08150698317379));
#30981=CARTESIAN_POINT('Ctrl Pts',(371.160566852821,-12.9431094133522,-4.07370905134738));
#30982=CARTESIAN_POINT('Ctrl Pts',(371.279515472225,-12.9489402429977,-4.06066793520912));
#30983=CARTESIAN_POINT('Ctrl Pts',(371.398360288104,-12.9547659842221,-4.04763819973106));
#30984=CARTESIAN_POINT('Ctrl Pts',(371.516745070039,-12.9605917254464,-4.02937442427085));
#30985=CARTESIAN_POINT('Ctrl Pts',(371.634177461656,-12.9664174666708,-4.00592680996524));
#30986=CARTESIAN_POINT('Ctrl Pts',(371.751534635918,-12.9722394764132,-3.98249421423779));
#30987=CARTESIAN_POINT('Ctrl Pts',(371.867940236911,-12.9780614861556,-3.95388446452583));
#30988=CARTESIAN_POINT('Ctrl Pts',(371.982909365183,-12.983883495898,-3.92019929833372));
#30989=CARTESIAN_POINT('Ctrl Pts',(372.103548474738,-12.9899926321653,-3.88485286650701));
#30990=CARTESIAN_POINT('Ctrl Pts',(372.222605346488,-12.9961017684327,-3.84391770095398));
#30991=CARTESIAN_POINT('Ctrl Pts',(372.339534650271,-13.0022109047,-3.79757124934956));
#30992=CARTESIAN_POINT('Ctrl Pts',(372.45092388261,-13.0080305921269,-3.75342067717669));
#30993=CARTESIAN_POINT('Ctrl Pts',(372.56038212615,-13.0138502795537,-3.70436000839369));
#30994=CARTESIAN_POINT('Ctrl Pts',(372.667456912096,-13.0196699669806,-3.65059258077859));
#30995=CARTESIAN_POINT('Ctrl Pts',(372.774535253417,-13.0254898476478,-3.59682336783856));
#30996=CARTESIAN_POINT('Ctrl Pts',(372.879229620213,-13.031309728315,-3.53834727302077));
#30997=CARTESIAN_POINT('Ctrl Pts',(372.981111631913,-13.0371296089822,-3.47541385618776));
#30998=CARTESIAN_POINT('Ctrl Pts',(373.083044319446,-13.042952384442,-3.41244913644588));
#30999=CARTESIAN_POINT('Ctrl Pts',(373.182161519185,-13.0487751599019,-3.34502288954575));
#31000=CARTESIAN_POINT('Ctrl Pts',(373.278063575703,-13.0545979353618,-3.27342814857261));
#31001=CARTESIAN_POINT('Ctrl Pts',(373.292311340686,-13.0554630006097,-3.26279161917505));
#31002=CARTESIAN_POINT('Ctrl Pts',(373.306488199698,-13.0563280658577,-3.2520631573204));
#31003=CARTESIAN_POINT('Ctrl Pts',(373.320592904309,-13.0571931311057,-3.2412437998941));
#31004=CARTESIAN_POINT('',(366.749318884821,-12.5103849713753,-0.00290312669601772));
#31005=CARTESIAN_POINT('Ctrl Pts',(366.749318884821,-12.5103849714045,-0.00290312729419502));
#31006=CARTESIAN_POINT('Ctrl Pts',(366.749446060986,-12.5191195890899,-0.181853083703761));
#31007=CARTESIAN_POINT('Ctrl Pts',(366.7613354519,-12.5278542067754,-0.360374148224009));
#31008=CARTESIAN_POINT('Ctrl Pts',(366.784798877521,-12.5365888244608,-0.537234646521026));
#31009=CARTESIAN_POINT('Ctrl Pts',(366.790770525782,-12.5388118615124,-0.582247199425974));
#31010=CARTESIAN_POINT('Ctrl Pts',(366.797491656539,-12.5410348985639,-0.627152337215535));
#31011=CARTESIAN_POINT('Ctrl Pts',(366.804958714245,-12.5432579356155,-0.671930003142868));
#31012=CARTESIAN_POINT('Ctrl Pts',(366.824571319474,-12.5490968550161,-0.789540810446197));
#31013=CARTESIAN_POINT('Ctrl Pts',(366.849367068929,-12.5549357744167,-0.906469559074163));
#31014=CARTESIAN_POINT('Ctrl Pts',(366.879285881915,-12.5607746938174,-1.02222654334833));
#31015=CARTESIAN_POINT('Ctrl Pts',(366.909168552415,-12.5666065596941,-1.13784369101978));
#31016=CARTESIAN_POINT('Ctrl Pts',(366.944161874345,-12.5724384255709,-1.25229150054339));
#31017=CARTESIAN_POINT('Ctrl Pts',(366.984154394552,-12.5782702914476,-1.36508840061911));
#31018=CARTESIAN_POINT('Ctrl Pts',(367.02410885248,-12.584096606934,-1.47777794794653));
#31019=CARTESIAN_POINT('Ctrl Pts',(367.069052906905,-12.5899229224203,-1.58881933170769));
#31020=CARTESIAN_POINT('Ctrl Pts',(367.118824890523,-12.5957492379067,-1.69774469344546));
#31021=CARTESIAN_POINT('Ctrl Pts',(367.168804875479,-12.6015999020592,-1.80712526350073));
#31022=CARTESIAN_POINT('Ctrl Pts',(367.223653126755,-12.6074505662118,-1.91437168577231));
#31023=CARTESIAN_POINT('Ctrl Pts',(367.283156328575,-12.6133012303643,-2.01902868376213));
#31024=CARTESIAN_POINT('Ctrl Pts',(367.34235086137,-12.6191215445735,-2.12314278031752));
#31025=CARTESIAN_POINT('Ctrl Pts',(367.406151954314,-12.6249418587826,-2.22469390223052));
#31026=CARTESIAN_POINT('Ctrl Pts',(367.474303120528,-12.6307621729918,-2.32325762584969));
#31027=CARTESIAN_POINT('Ctrl Pts',(367.542445783505,-12.636581760999,-2.42180905164888));
#31028=CARTESIAN_POINT('Ctrl Pts',(367.614937209356,-12.6424013490061,-2.51737348705528));
#31029=CARTESIAN_POINT('Ctrl Pts',(367.691477707239,-12.6482209370132,-2.60955567420667));
#31030=CARTESIAN_POINT('Ctrl Pts',(367.768026419891,-12.6540411496122,-2.70174775488331));
#31031=CARTESIAN_POINT('Ctrl Pts',(367.84862480948,-12.6598613622112,-2.79055655344866));
#31032=CARTESIAN_POINT('Ctrl Pts',(367.932933447541,-12.6656815748101,-2.87562054702316));
#31033=CARTESIAN_POINT('Ctrl Pts',(368.018015914505,-12.6715552083733,-2.96146530254966));
#31034=CARTESIAN_POINT('Ctrl Pts',(368.10687679585,-12.6774288419364,-3.04349585450657));
#31035=CARTESIAN_POINT('Ctrl Pts',(368.199130702685,-12.6833024754995,-3.12138009246459));
#31036=CARTESIAN_POINT('Ctrl Pts',(368.290674419577,-12.6891308925982,-3.19866476120734));
#31037=CARTESIAN_POINT('Ctrl Pts',(368.38555874387,-12.694959309697,-3.27186652911053));
#31038=CARTESIAN_POINT('Ctrl Pts',(368.483376228154,-12.7007877267958,-3.34070329055355));
#31039=CARTESIAN_POINT('Ctrl Pts',(368.582332004546,-12.7066839685911,-3.41034109838219));
#31040=CARTESIAN_POINT('Ctrl Pts',(368.684289279658,-12.7125802103864,-3.47551143355884));
#31041=CARTESIAN_POINT('Ctrl Pts',(368.788799639473,-12.7184764521816,-3.53596949042426));
#31042=CARTESIAN_POINT('Ctrl Pts',(368.893309999287,-12.7243726939769,-3.59642754728969));
#31043=CARTESIAN_POINT('Ctrl Pts',(369.000373041996,-12.7302689357721,-3.65217317911992));
#31044=CARTESIAN_POINT('Ctrl Pts',(369.109519486997,-12.7361651775674,-3.70301169264453));
#31045=CARTESIAN_POINT('Ctrl Pts',(369.217604489732,-12.7420040787845,-3.75335580484406));
#31046=CARTESIAN_POINT('Ctrl Pts',(369.328058479929,-12.7478429800017,-3.79903967485439));
#31047=CARTESIAN_POINT('Ctrl Pts',(369.440443621202,-12.7536818812188,-3.83983588520469));
#31048=CARTESIAN_POINT('Ctrl Pts',(369.552693012516,-12.7595137296299,-3.88058281783165));
#31049=CARTESIAN_POINT('Ctrl Pts',(369.666868536215,-12.765345578041,-3.91645369797176));
#31050=CARTESIAN_POINT('Ctrl Pts',(369.782510009237,-12.7711774264521,-3.94726807543239));
#31051=CARTESIAN_POINT('Ctrl Pts',(369.898041436527,-12.7770037252104,-3.97805312958341));
#31052=CARTESIAN_POINT('Ctrl Pts',(370.015035647441,-12.7828300239686,-4.00379115130258));
#31053=CARTESIAN_POINT('Ctrl Pts',(370.13301536792,-12.7886563227269,-4.02435085748074));
#31054=CARTESIAN_POINT('Ctrl Pts',(370.251488608377,-12.7945069934266,-4.04499656679313));
#31055=CARTESIAN_POINT('Ctrl Pts',(370.370955231997,-12.8003576641263,-4.06042040174536));
#31056=CARTESIAN_POINT('Ctrl Pts',(370.490919124178,-12.806208334826,-4.07054078875142));
#31057=CARTESIAN_POINT('Ctrl Pts',(370.610260274447,-12.8120286342382,-4.08060864004006));
#31058=CARTESIAN_POINT('Ctrl Pts',(370.730093133838,-12.8178489336505,-4.08542794862778));
#31059=CARTESIAN_POINT('Ctrl Pts',(370.849922621117,-12.8236692330628,-4.08497019465488));
#31060=CARTESIAN_POINT('Ctrl Pts',(370.969737172828,-12.8294888070319,-4.08451249773653));
#31061=CARTESIAN_POINT('Ctrl Pts',(371.089547947681,-12.835308381001,-4.07877904825922));
#31062=CARTESIAN_POINT('Ctrl Pts',(371.20885948237,-12.8411279549701,-4.06779345198799));
#31063=CARTESIAN_POINT('Ctrl Pts',(371.328183838266,-12.8469481543101,-4.05680667520559));
#31064=CARTESIAN_POINT('Ctrl Pts',(371.447008443368,-12.8527683536501,-4.04056666664336));
#31065=CARTESIAN_POINT('Ctrl Pts',(371.564843181007,-12.8585885529901,-4.01914888321729));
#31066=CARTESIAN_POINT('Ctrl Pts',(371.683760183603,-12.8644622085342,-3.99753438601298));
#31067=CARTESIAN_POINT('Ctrl Pts',(371.801668627411,-12.8703358640783,-3.97064658452506));
#31068=CARTESIAN_POINT('Ctrl Pts',(371.918076649626,-12.8762095196224,-3.93861547643594));
#31069=CARTESIAN_POINT('Ctrl Pts',(372.033587884055,-12.882037925514,-3.90683113060565));
#31070=CARTESIAN_POINT('Ctrl Pts',(372.147621363606,-12.8878663314056,-3.86998263011797));
#31071=CARTESIAN_POINT('Ctrl Pts',(372.259713997293,-12.8936947372973,-3.82824644353939));
#31072=CARTESIAN_POINT('Ctrl Pts',(372.373112001475,-12.8995910176676,-3.78602421979034));
#31073=CARTESIAN_POINT('Ctrl Pts',(372.484523274168,-12.9054872980379,-3.73879991462816));
#31074=CARTESIAN_POINT('Ctrl Pts',(372.593492304934,-12.9113835784083,-3.68680488342551));
#31075=CARTESIAN_POINT('Ctrl Pts',(372.7024613357,-12.9172798587786,-3.63480985222286));
#31076=CARTESIAN_POINT('Ctrl Pts',(372.808987776272,-12.923176139149,-3.57804434338448));
#31077=CARTESIAN_POINT('Ctrl Pts',(372.912645643586,-12.9290724195193,-3.51678526438691));
#31078=CARTESIAN_POINT('Ctrl Pts',(373.015293460927,-12.934911246095,-3.45612309841373));
#31079=CARTESIAN_POINT('Ctrl Pts',(373.115438001154,-12.9407500726706,-3.39087160201834));
#31080=CARTESIAN_POINT('Ctrl Pts',(373.212644085742,-12.9465888992462,-3.32126321325414));
#31081=CARTESIAN_POINT('Ctrl Pts',(373.249046223612,-12.9487754472479,-3.29519597502075));
#31082=CARTESIAN_POINT('Ctrl Pts',(373.285036497378,-12.9509619952495,-3.26851820839758));
#31083=CARTESIAN_POINT('Ctrl Pts',(373.320592904309,-12.9531485432512,-3.2412437998941));
#31084=CARTESIAN_POINT('Ctrl Pts',(373.320592904309,-11.7029891890582,-3.2412437998941));
#31085=CARTESIAN_POINT('Ctrl Pts',(373.415815346343,-11.7088227556447,-3.16820110500659));
#31086=CARTESIAN_POINT('Ctrl Pts',(373.507775120479,-11.7146563222311,-3.09099036517938));
#31087=CARTESIAN_POINT('Ctrl Pts',(373.596103007177,-11.7204898888176,-3.00994481069077));
#31088=CARTESIAN_POINT('Ctrl Pts',(373.684473431876,-11.7263262648029,-2.92886022531356));
#31089=CARTESIAN_POINT('Ctrl Pts',(373.769208197034,-11.7321626407882,-2.84393743064286));
#31090=CARTESIAN_POINT('Ctrl Pts',(373.849975623245,-11.7379990167735,-2.75554590128941));
#31091=CARTESIAN_POINT('Ctrl Pts',(373.930867304975,-11.74384437165,-2.66701838722159));
#31092=CARTESIAN_POINT('Ctrl Pts',(374.007779190319,-11.7496897265265,-2.57501178458781));
#31093=CARTESIAN_POINT('Ctrl Pts',(374.080420124952,-11.7555350814029,-2.47992843475072));
#31094=CARTESIAN_POINT('Ctrl Pts',(374.147087018295,-11.7608997102045,-2.39266480613139));
#31095=CARTESIAN_POINT('Ctrl Pts',(374.210156927106,-11.7662643390061,-2.30281024446178));
#31096=CARTESIAN_POINT('Ctrl Pts',(374.26943825272,-11.7716289678077,-2.21069510357402));
#31097=CARTESIAN_POINT('Ctrl Pts',(374.333919787428,-11.7774641864821,-2.11049954295302));
#31098=CARTESIAN_POINT('Ctrl Pts',(374.394112426899,-11.7832994051564,-2.00732742361212));
#31099=CARTESIAN_POINT('Ctrl Pts',(374.449731386498,-11.7891346238308,-1.90158091687371));
#31100=CARTESIAN_POINT('Ctrl Pts',(374.505282665015,-11.7949627417986,-1.7959630899606));
#31101=CARTESIAN_POINT('Ctrl Pts',(374.556271147337,-11.8007908597663,-1.68777746407828));
#31102=CARTESIAN_POINT('Ctrl Pts',(374.602455514835,-11.8066189777341,-1.5774547737256));
#31103=CARTESIAN_POINT('Ctrl Pts',(374.648595566398,-11.8124415033659,-1.46723794285413));
#31104=CARTESIAN_POINT('Ctrl Pts',(374.689940518865,-11.8182640289977,-1.35488850035528));
#31105=CARTESIAN_POINT('Ctrl Pts',(374.726295422058,-11.8240865546295,-1.24086083171895));
#31106=CARTESIAN_POINT('Ctrl Pts',(374.762834789011,-11.8299386235933,-1.12625458988658));
#31107=CARTESIAN_POINT('Ctrl Pts',(374.794333134061,-11.835790692557,-1.00995341201883));
#31108=CARTESIAN_POINT('Ctrl Pts',(374.820641806603,-11.8416427615208,-0.892438422924913));
#31109=CARTESIAN_POINT('Ctrl Pts',(374.846790335786,-11.8474592083914,-0.775638758602226));
#31110=CARTESIAN_POINT('Ctrl Pts',(374.867812118546,-11.8532756552619,-0.657640422919713));
#31111=CARTESIAN_POINT('Ctrl Pts',(374.883611621838,-11.8590921021325,-0.538929471695475));
#31112=CARTESIAN_POINT('Ctrl Pts',(374.899409092739,-11.8649078007963,-0.420233791019374));
#31113=CARTESIAN_POINT('Ctrl Pts',(374.909985566918,-11.8707234994602,-0.300826079803791));
#31114=CARTESIAN_POINT('Ctrl Pts',(374.915297099379,-11.876539198124,-0.181199868791646));
#31115=CARTESIAN_POINT('Ctrl Pts',(374.920609186343,-11.882355503923,-0.0615611692937222));
#31116=CARTESIAN_POINT('Ctrl Pts',(374.920655220787,-11.8881718097219,0.0582956694610412));
#31117=CARTESIAN_POINT('Ctrl Pts',(374.915443354271,-11.8939881155208,0.177875362829974));
#31118=CARTESIAN_POINT('Ctrl Pts',(374.910175301793,-11.8998671233741,0.298744172123527));
#31119=CARTESIAN_POINT('Ctrl Pts',(374.899535319673,-11.9057461312273,0.419329400749526));
#31120=CARTESIAN_POINT('Ctrl Pts',(374.883585693937,-11.9116251390805,0.539124247431361));
#31121=CARTESIAN_POINT('Ctrl Pts',(374.867783938921,-11.9174496420105,0.657808463019252));
#31122=CARTESIAN_POINT('Ctrl Pts',(374.846770710325,-11.9232741449405,0.775716497946804));
#31123=CARTESIAN_POINT('Ctrl Pts',(374.820657986065,-11.9290986478705,0.892366149796055));
#31124=CARTESIAN_POINT('Ctrl Pts',(374.794178722707,-11.9350049081854,1.01065318952119));
#31125=CARTESIAN_POINT('Ctrl Pts',(374.76245582688,-11.9409111685002,1.12764583113746));
#31126=CARTESIAN_POINT('Ctrl Pts',(374.725657927696,-11.9468174288151,1.24285856991482));
#31127=CARTESIAN_POINT('Ctrl Pts',(374.688860028511,-11.95272368913,1.35807130869217));
#31128=CARTESIAN_POINT('Ctrl Pts',(374.646987327792,-11.9586299494448,1.47150376096735));
#31129=CARTESIAN_POINT('Ctrl Pts',(374.600258039024,-11.9645362097597,1.58269375337675));
#31130=CARTESIAN_POINT('Ctrl Pts',(374.554060363458,-11.9703752778266,1.69261879891026));
#31131=CARTESIAN_POINT('Ctrl Pts',(374.502976104925,-11.9762143458936,1.80068521392595));
#31132=CARTESIAN_POINT('Ctrl Pts',(374.447176621336,-11.9820534139606,1.90643030863286));
#31133=CARTESIAN_POINT('Ctrl Pts',(374.391444570303,-11.9878854256311,2.01204761251769));
#31134=CARTESIAN_POINT('Ctrl Pts',(374.331008817673,-11.9937174373017,2.11534882070777));
#31135=CARTESIAN_POINT('Ctrl Pts',(374.266088835123,-11.9995494489722,2.21589100088402));
#31136=CARTESIAN_POINT('Ctrl Pts',(374.201230672302,-12.0053759071387,2.31633744027019));
#31137=CARTESIAN_POINT('Ctrl Pts',(374.131896994762,-12.0112023653052,2.41402974012144));
#31138=CARTESIAN_POINT('Ctrl Pts',(374.058352975092,-12.0170288234716,2.50854988648058));
#31139=CARTESIAN_POINT('Ctrl Pts',(373.984504106948,-12.0228794329816,2.60346182978713));
#31140=CARTESIAN_POINT('Ctrl Pts',(373.906410109799,-12.0287300424916,2.69517489856014));
#31141=CARTESIAN_POINT('Ctrl Pts',(373.824383482065,-12.0345806520016,2.78329526554843));
#31142=CARTESIAN_POINT('Ctrl Pts',(373.742779725081,-12.0404010999446,2.87096134681634));
#31143=CARTESIAN_POINT('Ctrl Pts',(373.657284075261,-12.0462215478876,2.95507138812689));
#31144=CARTESIAN_POINT('Ctrl Pts',(373.568243958236,-12.0520419958305,3.03527149565442));
#31145=CARTESIAN_POINT('Ctrl Pts',(373.479215007267,-12.0578617138616,3.11546154570612));
#31146=CARTESIAN_POINT('Ctrl Pts',(373.386642774676,-12.0636814318926,3.19174236597793));
#31147=CARTESIAN_POINT('Ctrl Pts',(373.290910004576,-12.0695011499237,3.2637984009301));
#31148=CARTESIAN_POINT('Ctrl Pts',(373.195167024865,-12.0753214886101,3.33586212044165));
#31149=CARTESIAN_POINT('Ctrl Pts',(373.096263161563,-12.0811418272966,3.40369991485691));
#31150=CARTESIAN_POINT('Ctrl Pts',(372.994612051475,-12.0869621659831,3.46703821395211));
#31151=CARTESIAN_POINT('Ctrl Pts',(372.89203352869,-12.0928356064604,3.53095437926721));
#31152=CARTESIAN_POINT('Ctrl Pts',(372.786657728871,-12.0987090469378,3.59028830160311));
#31153=CARTESIAN_POINT('Ctrl Pts',(372.678936160524,-12.1045824874152,3.6448056601651));
#31154=CARTESIAN_POINT('Ctrl Pts',(372.572038233735,-12.1104110194333,3.69890617776557));
#31155=CARTESIAN_POINT('Ctrl Pts',(372.462830682531,-12.1162395514514,3.74826341729464));
#31156=CARTESIAN_POINT('Ctrl Pts',(372.351775027263,-12.1220680834695,3.79269676153494));
#31157=CARTESIAN_POINT('Ctrl Pts',(372.239435857118,-12.1279639781765,3.83764363980664));
#31158=CARTESIAN_POINT('Ctrl Pts',(372.125205998687,-12.1338598728836,3.87755194849058));
#31159=CARTESIAN_POINT('Ctrl Pts',(372.00957812619,-12.1397557675906,3.91228683646628));
#31160=CARTESIAN_POINT('Ctrl Pts',(371.893950253693,-12.1456516622976,3.94702172444198));
#31161=CARTESIAN_POINT('Ctrl Pts',(371.776924791736,-12.1515475570046,3.97658314152301));
#31162=CARTESIAN_POINT('Ctrl Pts',(371.65900317064,-12.1574434517116,4.00088979193848));
#31163=CARTESIAN_POINT('Ctrl Pts',(371.542210115674,-12.1632829198956,4.02496381612208));
#31164=CARTESIAN_POINT('Ctrl Pts',(371.424186382237,-12.1691223880796,4.04395573241407));
#31165=CARTESIAN_POINT('Ctrl Pts',(371.305410560004,-12.1749618562636,4.05774526820234));
#31166=CARTESIAN_POINT('Ctrl Pts',(371.18677796321,-12.1807942829439,4.07151817592381));
#31167=CARTESIAN_POINT('Ctrl Pts',(371.067395481479,-12.1866267096242,4.08010113631497));
#31168=CARTESIAN_POINT('Ctrl Pts',(370.947752608512,-12.1924591363045,4.08342473376119));
#31169=CARTESIAN_POINT('Ctrl Pts',(370.828223363506,-12.1982860237768,4.08674517470008));
#31170=CARTESIAN_POINT('Ctrl Pts',(370.708434622704,-12.2041129112491,4.08481618009358));
#31171=CARTESIAN_POINT('Ctrl Pts',(370.588881163619,-12.2099397987214,4.07762011857352));
#31172=CARTESIAN_POINT('Ctrl Pts',(370.468844178012,-12.2157902526773,4.07039495303064));
#31173=CARTESIAN_POINT('Ctrl Pts',(370.349044792529,-12.2216407066332,4.05785997917041));
#31174=CARTESIAN_POINT('Ctrl Pts',(370.229984438167,-12.2274911605891,4.04005026249004));
#31175=CARTESIAN_POINT('Ctrl Pts',(370.111525327859,-12.2333120702801,4.02233048327302));
#31176=CARTESIAN_POINT('Ctrl Pts',(369.993798205446,-12.2391329799711,3.99938918136034));
#31177=CARTESIAN_POINT('Ctrl Pts',(369.877291467069,-12.2449538896621,3.97131281772197));
#31178=CARTESIAN_POINT('Ctrl Pts',(369.760799109049,-12.2507740808816,3.94323991953254));
#31179=CARTESIAN_POINT('Ctrl Pts',(369.645527229608,-12.2565942721012,3.91003331549513));
#31180=CARTESIAN_POINT('Ctrl Pts',(369.531952572461,-12.2624144633207,3.87183027461999));
#31181=CARTESIAN_POINT('Ctrl Pts',(369.418365590151,-12.2682352861495,3.83362308793687));
#31182=CARTESIAN_POINT('Ctrl Pts',(369.306476580753,-12.2740561089783,3.79041851562361));
#31183=CARTESIAN_POINT('Ctrl Pts',(369.196745125933,-12.2798769318072,3.74240304655078));
#31184=CARTESIAN_POINT('Ctrl Pts',(369.086033567296,-12.2857497452952,3.6939587109822));
#31185=CARTESIAN_POINT('Ctrl Pts',(368.977518684715,-12.2916225587832,3.64061727279132));
#31186=CARTESIAN_POINT('Ctrl Pts',(368.871648847597,-12.2974953722713,3.58261850806819));
#31187=CARTESIAN_POINT('Ctrl Pts',(368.766568138098,-12.303324411258,3.52505205181276));
#31188=CARTESIAN_POINT('Ctrl Pts',(368.664093494809,-12.3091534502448,3.46289772609776));
#31189=CARTESIAN_POINT('Ctrl Pts',(368.564634915113,-12.3149824892315,3.39643406537638));
#31190=CARTESIAN_POINT('Ctrl Pts',(368.464055974995,-12.3208771899702,3.32922171856612));
#31191=CARTESIAN_POINT('Ctrl Pts',(368.366561810464,-12.3267718907088,3.25760260622925));
#31192=CARTESIAN_POINT('Ctrl Pts',(368.272541956757,-12.3326665914475,3.18190654424048));
#31193=CARTESIAN_POINT('Ctrl Pts',(368.17852210305,-12.3385612921862,3.10621048225171));
#31194=CARTESIAN_POINT('Ctrl Pts',(368.087976841197,-12.3444559929248,3.02643779192481));
#31195=CARTESIAN_POINT('Ctrl Pts',(368.001256533536,-12.3503506936635,2.94295575211157));
#31196=CARTESIAN_POINT('Ctrl Pts',(367.9165766391,-12.3561066999525,2.86143793339836));
#31197=CARTESIAN_POINT('Ctrl Pts',(367.835271661091,-12.3618627062415,2.77612121230425));
#31198=CARTESIAN_POINT('Ctrl Pts',(367.757706503519,-12.3676187125305,2.68731978053693));
#31199=CARTESIAN_POINT('Ctrl Pts',(367.677546125477,-12.373567306649,2.59554717845714));
#31200=CARTESIAN_POINT('Ctrl Pts',(367.601380589502,-12.3795159007675,2.50005283176456));
#31201=CARTESIAN_POINT('Ctrl Pts',(367.529574331816,-12.3854644948861,2.40122786459643));
#31202=CARTESIAN_POINT('Ctrl Pts',(367.460253043918,-12.3912072284413,2.30582289264145));
#31203=CARTESIAN_POINT('Ctrl Pts',(367.394994607325,-12.3969499619965,2.20731436332425));
#31204=CARTESIAN_POINT('Ctrl Pts',(367.334087684944,-12.4026926955517,2.10608968685201));
#31205=CARTESIAN_POINT('Ctrl Pts',(367.27321546527,-12.4084321570915,2.00492268477958));
#31206=CARTESIAN_POINT('Ctrl Pts',(367.21669004701,-12.4141716186312,1.90104296940387));
#31207=CARTESIAN_POINT('Ctrl Pts',(367.164757049688,-12.4199110801709,1.79486726783742));
#31208=CARTESIAN_POINT('Ctrl Pts',(367.112840676174,-12.4256487045029,1.68872555322491));
#31209=CARTESIAN_POINT('Ctrl Pts',(367.065513984074,-12.431386328835,1.58028968977207));
#31210=CARTESIAN_POINT('Ctrl Pts',(367.022976482881,-12.437123953167,1.47000066622797));
#31211=CARTESIAN_POINT('Ctrl Pts',(366.980441978597,-12.4428611732642,1.35971941291494));
#31212=CARTESIAN_POINT('Ctrl Pts',(366.942696142886,-12.4485983933614,1.24758565055968));
#31213=CARTESIAN_POINT('Ctrl Pts',(366.909889918337,-12.4543356134585,1.1340592506042));
#31214=CARTESIAN_POINT('Ctrl Pts',(366.877065297994,-12.4600760506502,1.02046919174208));
#31215=CARTESIAN_POINT('Ctrl Pts',(366.84918593581,-12.4658164878419,0.905485338707638));
#31216=CARTESIAN_POINT('Ctrl Pts',(366.826352499821,-12.4715569250336,0.789581361179868));
#31217=CARTESIAN_POINT('Ctrl Pts',(366.803511276543,-12.4772993199879,0.673637854874063));
#31218=CARTESIAN_POINT('Ctrl Pts',(366.785719471897,-12.4830417149421,0.556774012647749));
#31219=CARTESIAN_POINT('Ctrl Pts',(366.773026140141,-12.4887841098964,0.439470842312813));
#31220=CARTESIAN_POINT('Ctrl Pts',(366.76032005478,-12.4945322745129,0.322049811802265));
#31221=CARTESIAN_POINT('Ctrl Pts',(366.752722693894,-12.5002804391295,0.204188989423663));
#31222=CARTESIAN_POINT('Ctrl Pts',(366.750231054696,-12.506028603746,0.0863714194148228));
#31223=CARTESIAN_POINT('Ctrl Pts',(366.749601607614,-12.5074807262891,0.0566079104001104));
#31224=CARTESIAN_POINT('Ctrl Pts',(366.749297741899,-12.5089328488322,0.0268471468875288));
#31225=CARTESIAN_POINT('Ctrl Pts',(366.749318884821,-12.5103849713753,-0.00290312669603759));
#31226=CARTESIAN_POINT('Ctrl Pts',(373.401623314432,-11.0032428439321,-2.20447834017448));
#31227=CARTESIAN_POINT('Ctrl Pts',(374.114700529909,-11.0675900496771,-1.37412681370391));
#31228=CARTESIAN_POINT('Ctrl Pts',(374.66124545863,-11.196239669406,1.01921189732481));
#31229=CARTESIAN_POINT('Ctrl Pts',(372.15745436975,-11.389191703119,3.73759104365418));
#31230=CARTESIAN_POINT('Ctrl Pts',(368.501159821847,-11.5820989450709,3.2032473452642));
#31231=CARTESIAN_POINT('Ctrl Pts',(366.872921458626,-11.7750061870228,-0.11142543318611));
#31232=CARTESIAN_POINT('Ctrl Pts',(368.685853908291,-11.9679134289748,-3.33036403785688));
#31233=CARTESIAN_POINT('Ctrl Pts',(372.365673949634,-12.1608206709267,-3.65521049942478));
#31234=CARTESIAN_POINT('Ctrl Pts',(374.714873489798,-12.3537279128786,-0.804512557128141));
#31235=CARTESIAN_POINT('Ctrl Pts',(373.692556454241,-12.5466351548306,2.74528784991064));
#31236=CARTESIAN_POINT('Ctrl Pts',(370.186873789973,-12.7395423967825,3.90983325738364));
#31237=CARTESIAN_POINT('Ctrl Pts',(367.243724661677,-12.9324496387344,1.67739797356575));
#31238=CARTESIAN_POINT('Ctrl Pts',(367.420207209062,-13.1253568806864,-2.01243168312488));
#31239=CARTESIAN_POINT('Ctrl Pts',(370.562994506799,-13.3182641226383,-3.95378328020931));
#31240=CARTESIAN_POINT('Ctrl Pts',(373.94151615113,-13.5111713645902,-2.45994757806193));
#31241=CARTESIAN_POINT('Ctrl Pts',(374.620392573799,-13.7040786065421,1.17118017245572));
#31242=CARTESIAN_POINT('Ctrl Pts',(372.009790107051,-13.8969858484941,3.78474415645268));
#31243=CARTESIAN_POINT('Ctrl Pts',(368.377896041367,-14.089893090446,3.10998560565922));
#31244=CARTESIAN_POINT('Ctrl Pts',(366.880227630963,-14.2828003323979,-0.266839434936402));
#31245=CARTESIAN_POINT('Ctrl Pts',(368.818020032292,-14.4757075743499,-3.41182744672225));
#31246=CARTESIAN_POINT('Ctrl Pts',(372.507634480805,-14.6686148163018,-3.59249097137997));
#31247=CARTESIAN_POINT('Ctrl Pts',(374.743433236741,-14.8615220582537,-0.651882042676315));
#31248=CARTESIAN_POINT('Ctrl Pts',(373.582802876223,-15.0544293002057,2.85513267318201));
#31249=CARTESIAN_POINT('Ctrl Pts',(370.034294735369,-15.2473365421576,3.88144023527511));
#31250=CARTESIAN_POINT('Ctrl Pts',(367.180641638276,-15.4402437841095,1.53553640908976));
#31251=CARTESIAN_POINT('Ctrl Pts',(367.501931150595,-15.6331510260615,-2.1448253743439));
#31252=CARTESIAN_POINT('Ctrl Pts',(370.717388069785,-15.8260582680134,-3.96115480385039));
#31253=CARTESIAN_POINT('Ctrl Pts',(374.036763485299,-16.0189655099653,-2.33765246017688));
#31254=CARTESIAN_POINT('Ctrl Pts',(374.568178063822,-16.2118727519173,1.31882301565855));
#31255=CARTESIAN_POINT('Ctrl Pts',(372.767084587514,-16.3404775798852,2.98520783922849));
#31256=CARTESIAN_POINT('Ctrl Pts',(371.710656479833,-16.4047799938692,3.26845729696387));
#31257=CARTESIAN_POINT('Ctrl Pts',(373.579892666462,-10.8675815057962,-2.35755359016106));
#31258=CARTESIAN_POINT('Ctrl Pts',(374.342484758555,-10.9319287115412,-1.46954385713212));
#31259=CARTESIAN_POINT('Ctrl Pts',(374.926980843371,-11.0605783312701,1.08998424882815));
#31260=CARTESIAN_POINT('Ctrl Pts',(372.249330733125,-11.2535303649831,3.99712304854097));
#31261=CARTESIAN_POINT('Ctrl Pts',(368.339149271594,-11.446437606935,3.42567542686938));
#31262=CARTESIAN_POINT('Ctrl Pts',(366.597848788441,-11.6393448488869,-0.119162626938022));
#31263=CARTESIAN_POINT('Ctrl Pts',(368.536668203236,-11.8322520908389,-3.5616188877462));
#31264=CARTESIAN_POINT('Ctrl Pts',(372.472008728708,-12.0251593327908,-3.90902213855786));
#31265=CARTESIAN_POINT('Ctrl Pts',(374.984332714381,-12.2180665747427,-0.860376549327761));
#31266=CARTESIAN_POINT('Ctrl Pts',(373.891027711771,-12.4109738166947,2.93591599819036));
#31267=CARTESIAN_POINT('Ctrl Pts',(370.141916368515,-12.6038810586466,4.18132547047225));
#31268=CARTESIAN_POINT('Ctrl Pts',(366.994399939188,-12.7967883005985,1.79387365375332));
#31269=CARTESIAN_POINT('Ctrl Pts',(367.183137136378,-12.9896955425505,-2.15217153783848));
#31270=CARTESIAN_POINT('Ctrl Pts',(370.544154272207,-13.1826027845024,-4.22832730859968));
#31271=CARTESIAN_POINT('Ctrl Pts',(374.157274749227,-13.3755100264543,-2.6307621801396));
#31272=CARTESIAN_POINT('Ctrl Pts',(374.883291203265,-13.5684172684062,1.25250494413109));
#31273=CARTESIAN_POINT('Ctrl Pts',(372.091412913603,-13.7613245103582,4.04755039379517));
#31274=CARTESIAN_POINT('Ctrl Pts',(368.207326262535,-13.9542317523101,3.32593774969494));
#31275=CARTESIAN_POINT('Ctrl Pts',(366.605662289035,-14.147138994262,-0.285368314292926));
#31276=CARTESIAN_POINT('Ctrl Pts',(368.678011719503,-14.340046236214,-3.64873897803573));
#31277=CARTESIAN_POINT('Ctrl Pts',(372.623826759225,-14.5329534781659,-3.84194747249261));
#31278=CARTESIAN_POINT('Ctrl Pts',(375.014875601881,-14.7258607201178,-0.697147629924748));
#31279=CARTESIAN_POINT('Ctrl Pts',(373.773653030798,-14.9187679620698,3.05338826033268));
#31280=CARTESIAN_POINT('Ctrl Pts',(369.978742482244,-15.1116752040217,4.1509608848977));
#31281=CARTESIAN_POINT('Ctrl Pts',(366.926936537262,-15.3045824459736,1.64216146201104));
#31282=CARTESIAN_POINT('Ctrl Pts',(367.270535850282,-15.4974896879256,-2.29375842320719));
#31283=CARTESIAN_POINT('Ctrl Pts',(370.709268663256,-15.6903969298775,-4.23621069838323));
#31284=CARTESIAN_POINT('Ctrl Pts',(374.259135897296,-15.8833041718294,-2.4999750959688));
#31285=CARTESIAN_POINT('Ctrl Pts',(374.827451005967,-16.0762114137814,1.41039985682362));
#31286=CARTESIAN_POINT('Ctrl Pts',(372.901292642829,-16.2048162417493,3.19249562605957));
#31287=CARTESIAN_POINT('Ctrl Pts',(371.771507952899,-16.2691186557333,3.49541344739883));
#31288=CARTESIAN_POINT('Ctrl Pts',(373.758162018492,-10.7319201676602,-2.51062884014765));
#31289=CARTESIAN_POINT('Ctrl Pts',(374.570268987202,-10.7962673734052,-1.56496090056034));
#31290=CARTESIAN_POINT('Ctrl Pts',(375.192716228111,-10.9249169931341,1.16075660033148));
#31291=CARTESIAN_POINT('Ctrl Pts',(372.3412070965,-11.1178690268471,4.25665505342777));
#31292=CARTESIAN_POINT('Ctrl Pts',(368.177138721342,-11.310776268799,3.64810350847456));
#31293=CARTESIAN_POINT('Ctrl Pts',(366.322776118255,-11.5036835107509,-0.126899820689938));
#31294=CARTESIAN_POINT('Ctrl Pts',(368.38748249818,-11.6965907527029,-3.7928737376355));
#31295=CARTESIAN_POINT('Ctrl Pts',(372.578343507783,-11.8894979946548,-4.16283377769094));
#31296=CARTESIAN_POINT('Ctrl Pts',(375.253791938965,-12.0824052366067,-0.916240541527381));
#31297=CARTESIAN_POINT('Ctrl Pts',(374.089498969301,-12.2753124785587,3.12654414647007));
#31298=CARTESIAN_POINT('Ctrl Pts',(370.096958947057,-12.4682197205106,4.45281768356085));
#31299=CARTESIAN_POINT('Ctrl Pts',(366.7450752167,-12.6611269624625,1.91034933394088));
#31300=CARTESIAN_POINT('Ctrl Pts',(366.946067063693,-12.8540342044145,-2.29191139255208));
#31301=CARTESIAN_POINT('Ctrl Pts',(370.525314037616,-13.0469414463664,-4.50287133699005));
#31302=CARTESIAN_POINT('Ctrl Pts',(374.373033347323,-13.2398486883183,-2.80157678221726));
#31303=CARTESIAN_POINT('Ctrl Pts',(375.146189832731,-13.4327559302702,1.33382971580646));
#31304=CARTESIAN_POINT('Ctrl Pts',(372.173035720154,-13.6256631722222,4.31035663113766));
#31305=CARTESIAN_POINT('Ctrl Pts',(368.036756483703,-13.8185704141741,3.54188989373065));
#31306=CARTESIAN_POINT('Ctrl Pts',(366.331096947107,-14.011477656126,-0.303897193649457));
#31307=CARTESIAN_POINT('Ctrl Pts',(368.538003406714,-14.204384898078,-3.88565050934918));
#31308=CARTESIAN_POINT('Ctrl Pts',(372.740019037646,-14.3972921400299,-4.09140397360527));
#31309=CARTESIAN_POINT('Ctrl Pts',(375.286317967022,-14.5901993819818,-0.742413217173175));
#31310=CARTESIAN_POINT('Ctrl Pts',(373.964503185373,-14.7831066239338,3.25164384748334));
#31311=CARTESIAN_POINT('Ctrl Pts',(369.92319022912,-14.9760138658857,4.42048153452028));
#31312=CARTESIAN_POINT('Ctrl Pts',(366.67323143625,-15.1689211078376,1.74878651493233));
#31313=CARTESIAN_POINT('Ctrl Pts',(367.03914054997,-15.3618283497896,-2.44269147207048));
#31314=CARTESIAN_POINT('Ctrl Pts',(370.701149256725,-15.5547355917415,-4.51126659291607));
#31315=CARTESIAN_POINT('Ctrl Pts',(374.481508309292,-15.7476428336934,-2.66229773176073));
#31316=CARTESIAN_POINT('Ctrl Pts',(375.086723948113,-15.9405500756454,1.50197669798869));
#31317=CARTESIAN_POINT('Ctrl Pts',(373.035500698143,-16.0691549036133,3.39978341289065));
#31318=CARTESIAN_POINT('Ctrl Pts',(371.832359425964,-16.1334573175973,3.72236959783378));
#31319=CARTESIAN_POINT('Ctrl Pts',(373.936431370522,-10.5962588295242,-2.66370409013424));
#31320=CARTESIAN_POINT('Ctrl Pts',(374.798053215848,-10.6606060352692,-1.66037794398857));
#31321=CARTESIAN_POINT('Ctrl Pts',(375.458451612851,-10.7892556549982,1.2315289518348));
#31322=CARTESIAN_POINT('Ctrl Pts',(372.433083459874,-10.9822076887111,4.51618705831456));
#31323=CARTESIAN_POINT('Ctrl Pts',(368.01512817109,-11.175114930663,3.87053159007975));
#31324=CARTESIAN_POINT('Ctrl Pts',(366.047703448069,-11.3680221726149,-0.134637014441852));
#31325=CARTESIAN_POINT('Ctrl Pts',(368.238296793125,-11.5609294145669,-4.02412858752481));
#31326=CARTESIAN_POINT('Ctrl Pts',(372.684678286857,-11.7538366565188,-4.41664541682402));
#31327=CARTESIAN_POINT('Ctrl Pts',(375.52325116355,-11.9467438984707,-0.972104533727002));
#31328=CARTESIAN_POINT('Ctrl Pts',(374.287970226831,-12.1396511404227,3.31717229474979));
#31329=CARTESIAN_POINT('Ctrl Pts',(370.052001525598,-12.3325583823746,4.72430989664947));
#31330=CARTESIAN_POINT('Ctrl Pts',(366.495750494211,-12.5254656243265,2.02682501412844));
#31331=CARTESIAN_POINT('Ctrl Pts',(366.708996991008,-12.7183728662785,-2.43165124726568));
#31332=CARTESIAN_POINT('Ctrl Pts',(370.506473803024,-12.9112801082304,-4.77741536538043));
#31333=CARTESIAN_POINT('Ctrl Pts',(374.588791945419,-13.1041873501823,-2.97239138429492));
#31334=CARTESIAN_POINT('Ctrl Pts',(375.409088462197,-13.2970945921343,1.41515448748183));
#31335=CARTESIAN_POINT('Ctrl Pts',(372.254658526706,-13.4900018340862,4.57316286848015));
#31336=CARTESIAN_POINT('Ctrl Pts',(367.866186704872,-13.6829090760381,3.75784203776637));
#31337=CARTESIAN_POINT('Ctrl Pts',(366.056531605179,-13.8758163179901,-0.322426073005982));
#31338=CARTESIAN_POINT('Ctrl Pts',(368.397995093925,-14.068723559942,-4.12256204066265));
#31339=CARTESIAN_POINT('Ctrl Pts',(372.856211316067,-14.2616308018939,-4.34086047471791));
#31340=CARTESIAN_POINT('Ctrl Pts',(375.557760332163,-14.4545380438458,-0.787678804421608));
#31341=CARTESIAN_POINT('Ctrl Pts',(374.155353339948,-14.6474452857978,3.449899434634));
#31342=CARTESIAN_POINT('Ctrl Pts',(369.867637975995,-14.8403525277497,4.69000218414286));
#31343=CARTESIAN_POINT('Ctrl Pts',(366.419526335239,-15.0332597697016,1.8554115678536));
#31344=CARTESIAN_POINT('Ctrl Pts',(366.807745249658,-15.2261670116536,-2.59162452093377));
#31345=CARTESIAN_POINT('Ctrl Pts',(370.693029850195,-15.4190742536055,-4.78632248744892));
#31346=CARTESIAN_POINT('Ctrl Pts',(374.703880721289,-15.6119814955574,-2.82462036755265));
#31347=CARTESIAN_POINT('Ctrl Pts',(375.345996890258,-15.8048887375094,1.59355353915376));
#31348=CARTESIAN_POINT('Ctrl Pts',(373.169708753457,-15.9334935654773,3.60707119972172));
#31349=CARTESIAN_POINT('Ctrl Pts',(371.89321089903,-15.9977959794613,3.94932574826872));
#31350=CARTESIAN_POINT('',(373.410035938374,-16.0015042489531,-2.20760138325762));
#31351=CARTESIAN_POINT('Ctrl Pts',(371.892222276197,-16.,3.94563850749836));
#31352=CARTESIAN_POINT('Ctrl Pts',(372.00766095465,-15.9999999999999,3.90400799429217));
#31353=CARTESIAN_POINT('Ctrl Pts',(372.120751036376,-16.,3.85687012175642));
#31354=CARTESIAN_POINT('Ctrl Pts',(372.231265838281,-16.,3.80457808135728));
#31355=CARTESIAN_POINT('Ctrl Pts',(372.344397845895,-16.,3.75104766361569));
#31356=CARTESIAN_POINT('Ctrl Pts',(372.454831795132,-15.9999999999999,3.69211553098066));
#31357=CARTESIAN_POINT('Ctrl Pts',(372.562297061756,-16.,3.62811345741236));
#31358=CARTESIAN_POINT('Ctrl Pts',(372.670203120231,-16.,3.5638488656059));
#31359=CARTESIAN_POINT('Ctrl Pts',(372.775116671354,-16.,3.49447195769568));
#31360=CARTESIAN_POINT('Ctrl Pts',(372.876727258344,-16.,3.42028126215052));
#31361=CARTESIAN_POINT('Ctrl Pts',(372.96904895601,-16.,3.35287282404679));
#31362=CARTESIAN_POINT('Ctrl Pts',(373.058643839984,-15.9999999999999,3.28148965541649));
#31363=CARTESIAN_POINT('Ctrl Pts',(373.145247083194,-16.0000000000001,3.20633639014722));
#31364=CARTESIAN_POINT('Ctrl Pts',(373.164880954339,-16.0000000000001,3.18929835009579));
#31365=CARTESIAN_POINT('Ctrl Pts',(373.184360925769,-16.,3.17206647738346));
#31366=CARTESIAN_POINT('Ctrl Pts',(373.203683664656,-15.9999999999999,3.15464306282877));
#31367=CARTESIAN_POINT('Ctrl Pts',(373.216927786189,-15.9999999999999,3.14270076928359));
#31368=CARTESIAN_POINT('Ctrl Pts',(373.23009863355,-16.0000000000001,3.13066785595378));
#31369=CARTESIAN_POINT('Ctrl Pts',(373.243183050314,-16.0000000000001,3.11855646221841));
#31370=CARTESIAN_POINT('Ctrl Pts',(373.33364353757,-16.0000000000001,3.03482307169897));
#31371=CARTESIAN_POINT('Ctrl Pts',(373.42011548176,-16.,2.94721697828212));
#31372=CARTESIAN_POINT('Ctrl Pts',(373.502339350481,-16.,2.85605153031309));
#31373=CARTESIAN_POINT('Ctrl Pts',(373.584244725785,-15.9999999999999,2.76523921088744));
#31374=CARTESIAN_POINT('Ctrl Pts',(373.661935350705,-16.0000000000002,2.67089432715435));
#31375=CARTESIAN_POINT('Ctrl Pts',(373.735112222466,-16.0000000000001,2.57329767500623));
#31376=CARTESIAN_POINT('Ctrl Pts',(373.806575122233,-16.0000000000001,2.47798696272338));
#31377=CARTESIAN_POINT('Ctrl Pts',(373.87373351298,-15.9999999999999,2.37957432698915));
#31378=CARTESIAN_POINT('Ctrl Pts',(373.936263021939,-16.,2.27830427081384));
#31379=CARTESIAN_POINT('Ctrl Pts',(373.987439735759,-16.,2.19542070480252));
#31380=CARTESIAN_POINT('Ctrl Pts',(374.035515083554,-16.,2.11062265575148));
#31381=CARTESIAN_POINT('Ctrl Pts',(374.080285480975,-16.0000000000002,2.02404008054505));
#31382=CARTESIAN_POINT('Ctrl Pts',(374.091160603096,-16.0000000000002,2.00300841379185));
#31383=CARTESIAN_POINT('Ctrl Pts',(374.101840603285,-16.0000000000002,1.98187144431043));
#31384=CARTESIAN_POINT('Ctrl Pts',(374.1123223389,-16.0000000000001,1.96063102654543));
#31385=CARTESIAN_POINT('Ctrl Pts',(374.119864193759,-16.,1.9453480472948));
#31386=CARTESIAN_POINT('Ctrl Pts',(374.127303555414,-16.0000000000001,1.93001104216781));
#31387=CARTESIAN_POINT('Ctrl Pts',(374.134632738564,-16.0000000000001,1.91463475312349));
#31388=CARTESIAN_POINT('Ctrl Pts',(374.18577050072,-16.,1.80735008088746));
#31389=CARTESIAN_POINT('Ctrl Pts',(374.231630364951,-15.9999999999999,1.69799098092543));
#31390=CARTESIAN_POINT('Ctrl Pts',(374.271931697881,-15.9999999999999,1.58681986635038));
#31391=CARTESIAN_POINT('Ctrl Pts',(374.31223303081,-16.,1.47564875177531));
#31392=CARTESIAN_POINT('Ctrl Pts',(374.346976278227,-16.,1.36266495248243));
#31393=CARTESIAN_POINT('Ctrl Pts',(374.375826174163,-16.0000000000001,1.24811885600915));
#31394=CARTESIAN_POINT('Ctrl Pts',(374.404754628375,-16.0000000000001,1.13326085047907));
#31395=CARTESIAN_POINT('Ctrl Pts',(374.427757026081,-15.9999999999998,1.01683097387319));
#31396=CARTESIAN_POINT('Ctrl Pts',(374.444913268172,-15.9999999999999,0.899262695184769));
#31397=CARTESIAN_POINT('Ctrl Pts',(374.454304156307,-15.9999999999999,0.834908826340758));
#31398=CARTESIAN_POINT('Ctrl Pts',(374.461942509795,-16.,0.770213970303242));
#31399=CARTESIAN_POINT('Ctrl Pts',(374.467835068193,-16.,0.705250877016903));
#31400=CARTESIAN_POINT('Ctrl Pts',(374.471057772603,-15.9999999999999,0.669721853270472));
#31401=CARTESIAN_POINT('Ctrl Pts',(374.473758213052,-16.,0.634112624184912));
#31402=CARTESIAN_POINT('Ctrl Pts',(374.475936951666,-16.,0.598435335677741));
#31403=CARTESIAN_POINT('Ctrl Pts',(374.477004684917,-16.,0.580950986248066));
#31404=CARTESIAN_POINT('Ctrl Pts',(374.477947198307,-15.9999999999998,0.563448511156703));
#31405=CARTESIAN_POINT('Ctrl Pts',(374.478764267789,-15.9999999999999,0.545934959024219));
#31406=CARTESIAN_POINT('Ctrl Pts',(374.484180436908,-16.0000000000001,0.429841576206889));
#31407=CARTESIAN_POINT('Ctrl Pts',(374.484072705153,-16.,0.3136354074497));
#31408=CARTESIAN_POINT('Ctrl Pts',(374.47857613537,-15.9999999999999,0.197720257635413));
#31409=CARTESIAN_POINT('Ctrl Pts',(374.47306143737,-15.9999999999998,0.0814228084803152));
#31410=CARTESIAN_POINT('Ctrl Pts',(374.462122003252,-16.0000000000001,-0.0345826156124334));
#31411=CARTESIAN_POINT('Ctrl Pts',(374.44584221609,-16.0000000000001,-0.149879655715812));
#31412=CARTESIAN_POINT('Ctrl Pts',(374.42973649359,-16.,-0.263943931526349));
#31413=CARTESIAN_POINT('Ctrl Pts',(374.408403628591,-16.0000000000001,-0.37731571180236));
#31414=CARTESIAN_POINT('Ctrl Pts',(374.381879673776,-16.,-0.489570606992328));
#31415=CARTESIAN_POINT('Ctrl Pts',(374.365217561952,-15.9999999999999,-0.56008813084572));
#31416=CARTESIAN_POINT('Ctrl Pts',(374.346506033578,-16.0000000000001,-0.630164438406834));
#31417=CARTESIAN_POINT('Ctrl Pts',(374.32574563494,-16.,-0.699687792345608));
#31418=CARTESIAN_POINT('Ctrl Pts',(374.314654561951,-15.9999999999999,-0.736830074941256));
#31419=CARTESIAN_POINT('Ctrl Pts',(374.302978605753,-16.,-0.773814439918066));
#31420=CARTESIAN_POINT('Ctrl Pts',(374.290717142131,-16.,-0.810623111675999));
#31421=CARTESIAN_POINT('Ctrl Pts',(374.284608867747,-15.9999999999999,-0.828960030801155));
#31422=CARTESIAN_POINT('Ctrl Pts',(374.278354559896,-15.9999999999998,-0.847255206523337));
#31423=CARTESIAN_POINT('Ctrl Pts',(374.271960105546,-15.9999999999998,-0.865489809766218));
#31424=CARTESIAN_POINT('Ctrl Pts',(374.234721434297,-16.0000000000001,-0.971680636746369));
#31425=CARTESIAN_POINT('Ctrl Pts',(374.192694947791,-16.0000000000001,-1.075938071221));
#31426=CARTESIAN_POINT('Ctrl Pts',(374.145929614334,-16.0000000000001,-1.17786253481042));
#31427=CARTESIAN_POINT('Ctrl Pts',(374.110855614242,-16.0000000000001,-1.25430588250247));
#31428=CARTESIAN_POINT('Ctrl Pts',(374.073115090259,-15.9999999999998,-1.32943652806763));
#31429=CARTESIAN_POINT('Ctrl Pts',(374.032714072705,-16.,-1.40307333334082));
#31430=CARTESIAN_POINT('Ctrl Pts',(374.012405921882,-16.0000000000001,-1.44008792946224));
#31431=CARTESIAN_POINT('Ctrl Pts',(373.991425351126,-15.9999999999998,-1.47672488375371));
#31432=CARTESIAN_POINT('Ctrl Pts',(373.969772022922,-16.,-1.51295991340807));
#31433=CARTESIAN_POINT('Ctrl Pts',(373.957520800147,-16.0000000000001,-1.53346130776109));
#31434=CARTESIAN_POINT('Ctrl Pts',(373.945054202837,-16.,-1.55383402251675));
#31435=CARTESIAN_POINT('Ctrl Pts',(373.932372070541,-16.,-1.57407352405639));
#31436=CARTESIAN_POINT('Ctrl Pts',(373.922781198224,-16.0000000000001,-1.58937966268586));
#31437=CARTESIAN_POINT('Ctrl Pts',(373.913068078195,-16.0000000000001,-1.60460789185709));
#31438=CARTESIAN_POINT('Ctrl Pts',(373.90323766738,-16.0000000000001,-1.61974887144166));
#31439=CARTESIAN_POINT('Ctrl Pts',(373.844544342933,-15.9999999999998,-1.71014940952207));
#31440=CARTESIAN_POINT('Ctrl Pts',(373.781624617244,-15.9999999999999,-1.79751979106278));
#31441=CARTESIAN_POINT('Ctrl Pts',(373.714499732742,-16.,-1.88147730110623));
#31442=CARTESIAN_POINT('Ctrl Pts',(373.677193093894,-16.0000000000001,-1.92813916919038));
#31443=CARTESIAN_POINT('Ctrl Pts',(373.638586897237,-15.9999999999999,-1.97374619699087));
#31444=CARTESIAN_POINT('Ctrl Pts',(373.598680408904,-15.9999999999999,-2.01822719257774));
#31445=CARTESIAN_POINT('Ctrl Pts',(373.539303779228,-16.,-2.08441020473598));
#31446=CARTESIAN_POINT('Ctrl Pts',(373.477048640108,-16.,-2.14810122424028));
#31447=CARTESIAN_POINT('Ctrl Pts',(373.412117880462,-15.9999999999998,-2.2092048034827));
#31448=CARTESIAN_POINT('Ctrl Pts',(373.407552280239,-11.,-2.20655152809227));
#31449=CARTESIAN_POINT('Ctrl Pts',(373.484164508103,-11.0000000000001,-2.13363933676576));
#31450=CARTESIAN_POINT('Ctrl Pts',(373.556850099011,-10.9999999999999,-2.05708919551984));
#31451=CARTESIAN_POINT('Ctrl Pts',(373.625609529926,-11.,-1.97731684646155));
#31452=CARTESIAN_POINT('Ctrl Pts',(373.696087228626,-11.0000000000001,-1.89555102166244));
#31453=CARTESIAN_POINT('Ctrl Pts',(373.76244049017,-10.9999999999999,-1.81039952484827));
#31454=CARTESIAN_POINT('Ctrl Pts',(373.824643791805,-11.,-1.72226175147527));
#31455=CARTESIAN_POINT('Ctrl Pts',(373.88816280824,-11.,-1.63225970129142));
#31456=CARTESIAN_POINT('Ctrl Pts',(373.947354900361,-10.9999999999999,-1.53914316978695));
#31457=CARTESIAN_POINT('Ctrl Pts',(374.002159551767,-10.9999999999999,-1.44329500707418));
#31458=CARTESIAN_POINT('Ctrl Pts',(374.053687620609,-10.9999999999999,-1.3531772780149));
#31459=CARTESIAN_POINT('Ctrl Pts',(374.101337144399,-11.0000000000001,-1.26064392327993));
#31460=CARTESIAN_POINT('Ctrl Pts',(374.145026500752,-11.0000000000001,-1.16598700574379));
#31461=CARTESIAN_POINT('Ctrl Pts',(374.152708549467,-11.0000000000001,-1.14934315670631));
#31462=CARTESIAN_POINT('Ctrl Pts',(374.160268078308,-11.,-1.13263360147186));
#31463=CARTESIAN_POINT('Ctrl Pts',(374.167704536593,-11.0000000000001,-1.11585986664135));
#31464=CARTESIAN_POINT('Ctrl Pts',(374.174057108471,-11.0000000000002,-1.10153095466744));
#31465=CARTESIAN_POINT('Ctrl Pts',(374.180315995137,-10.9999999999999,-1.08716393738812));
#31466=CARTESIAN_POINT('Ctrl Pts',(374.186480716856,-10.9999999999999,-1.0727610067648));
#31467=CARTESIAN_POINT('Ctrl Pts',(374.231299693678,-10.9999999999999,-0.968048313613609));
#31468=CARTESIAN_POINT('Ctrl Pts',(374.271152113617,-11.0000000000001,-0.861423109955285));
#31469=CARTESIAN_POINT('Ctrl Pts',(374.30600663119,-11.,-0.753314769919725));
#31470=CARTESIAN_POINT('Ctrl Pts',(374.34138484736,-10.9999999999999,-0.643582072697306));
#31471=CARTESIAN_POINT('Ctrl Pts',(374.371614293078,-10.9999999999999,-0.532320624946264));
#31472=CARTESIAN_POINT('Ctrl Pts',(374.396622579182,-11.,-0.419943006692207));
#31473=CARTESIAN_POINT('Ctrl Pts',(374.421855131763,-11.0000000000001,-0.306557621155216));
#31474=CARTESIAN_POINT('Ctrl Pts',(374.441772914412,-10.9999999999999,-0.192035136737321));
#31475=CARTESIAN_POINT('Ctrl Pts',(374.456254753839,-10.9999999999999,-0.0767741815375196));
#31476=CARTESIAN_POINT('Ctrl Pts',(374.467116133409,-10.9999999999999,0.00967153486233469));
#31477=CARTESIAN_POINT('Ctrl Pts',(374.474918871082,-11.,0.0965332453698254));
#31478=CARTESIAN_POINT('Ctrl Pts',(374.47959245864,-11.,0.183647619031922));
#31479=CARTESIAN_POINT('Ctrl Pts',(374.480430050729,-11.,0.199260102872992));
#31480=CARTESIAN_POINT('Ctrl Pts',(374.481167091454,-11.,0.214880707141451));
#31481=CARTESIAN_POINT('Ctrl Pts',(374.481803114277,-11.,0.230508496459851));
#31482=CARTESIAN_POINT('Ctrl Pts',(374.482481222596,-10.9999999999999,0.247170373304957));
#31483=CARTESIAN_POINT('Ctrl Pts',(374.483044115965,-10.9999999999997,0.263831297496222));
#31484=CARTESIAN_POINT('Ctrl Pts',(374.483491541806,-10.9999999999998,0.280486880814511));
#31485=CARTESIAN_POINT('Ctrl Pts',(374.486677685243,-10.9999999999998,0.399092183945026));
#31486=CARTESIAN_POINT('Ctrl Pts',(374.484014434623,-10.9999999999998,0.517476627121978));
#31487=CARTESIAN_POINT('Ctrl Pts',(374.475431647664,-10.9999999999999,0.635212121420028));
#31488=CARTESIAN_POINT('Ctrl Pts',(374.467426874872,-10.9999999999999,0.745018631346651));
#31489=CARTESIAN_POINT('Ctrl Pts',(374.45427284864,-10.9999999999998,0.854261519988693));
#31490=CARTESIAN_POINT('Ctrl Pts',(374.435874189068,-10.9999999999999,0.962607274232096));
#31491=CARTESIAN_POINT('Ctrl Pts',(374.416682752686,-11.,1.07562152082828));
#31492=CARTESIAN_POINT('Ctrl Pts',(374.391785849854,-10.9999999999998,1.18766042245905));
#31493=CARTESIAN_POINT('Ctrl Pts',(374.361479323342,-10.9999999999999,1.29845785681547));
#31494=CARTESIAN_POINT('Ctrl Pts',(374.342689269744,-11.,1.36715229229592));
#31495=CARTESIAN_POINT('Ctrl Pts',(374.321818678637,-10.9999999999999,1.43536952436879));
#31496=CARTESIAN_POINT('Ctrl Pts',(374.298928231114,-11.,1.50304501988366));
#31497=CARTESIAN_POINT('Ctrl Pts',(374.286672454928,-11.,1.53927916189878));
#31498=CARTESIAN_POINT('Ctrl Pts',(374.273837535033,-11.,1.57535798511614));
#31499=CARTESIAN_POINT('Ctrl Pts',(374.260431959166,-11.0000000000001,1.61127137589293));
#31500=CARTESIAN_POINT('Ctrl Pts',(374.252732754366,-11.0000000000001,1.63189746114107));
#31501=CARTESIAN_POINT('Ctrl Pts',(374.244843634651,-11.,1.65247297333473));
#31502=CARTESIAN_POINT('Ctrl Pts',(374.236776829888,-11.,1.6729695185202));
#31503=CARTESIAN_POINT('Ctrl Pts',(374.193756623204,-11.,1.78227743361823));
#31504=CARTESIAN_POINT('Ctrl Pts',(374.145638532941,-10.9999999999999,1.88947606107137));
#31505=CARTESIAN_POINT('Ctrl Pts',(374.092775693224,-11.,1.99429708346387));
#31506=CARTESIAN_POINT('Ctrl Pts',(374.03834197434,-11.,2.10223298127993));
#31507=CARTESIAN_POINT('Ctrl Pts',(373.978877168769,-10.9999999999999,2.20764856732848));
#31508=CARTESIAN_POINT('Ctrl Pts',(373.914710641423,-11.,2.31024771811314));
#31509=CARTESIAN_POINT('Ctrl Pts',(373.850544114076,-11.0000000000001,2.41284686889779));
#31510=CARTESIAN_POINT('Ctrl Pts',(373.781675419372,-11.,2.51263031159976));
#31511=CARTESIAN_POINT('Ctrl Pts',(373.70838352593,-11.,2.60928799789692));
#31512=CARTESIAN_POINT('Ctrl Pts',(373.658795943347,-11.,2.67468432996569));
#31513=CARTESIAN_POINT('Ctrl Pts',(373.607182576977,-11.,2.73864953564559));
#31514=CARTESIAN_POINT('Ctrl Pts',(373.55361831323,-11.,2.80108138650798));
#31515=CARTESIAN_POINT('Ctrl Pts',(373.534988737123,-11.,2.82279509702634));
#31516=CARTESIAN_POINT('Ctrl Pts',(373.516123096266,-10.9999999999999,2.8443232731753));
#31517=CARTESIAN_POINT('Ctrl Pts',(373.497024303559,-11.,2.86566142895363));
#31518=CARTESIAN_POINT('Ctrl Pts',(373.485069089254,-11.,2.87901841068074));
#31519=CARTESIAN_POINT('Ctrl Pts',(373.473022095985,-10.9999999999999,2.89230139020273));
#31520=CARTESIAN_POINT('Ctrl Pts',(373.460885295567,-10.9999999999999,2.90550785313149));
#31521=CARTESIAN_POINT('Ctrl Pts',(373.375975367293,-11.0000000000001,2.99790121723507));
#31522=CARTESIAN_POINT('Ctrl Pts',(373.286963615328,-11.,3.08623632965698));
#31523=CARTESIAN_POINT('Ctrl Pts',(373.194175441271,-11.,3.17018989640025));
#31524=CARTESIAN_POINT('Ctrl Pts',(373.119592675862,-11.,3.23767143957404));
#31525=CARTESIAN_POINT('Ctrl Pts',(373.042568901898,-11.,3.30232200719299));
#31526=CARTESIAN_POINT('Ctrl Pts',(372.963251804661,-11.0000000000001,3.36396181620956));
#31527=CARTESIAN_POINT('Ctrl Pts',(372.897202039085,-11.0000000000002,3.41529116483014));
#31528=CARTESIAN_POINT('Ctrl Pts',(372.829561609887,-11.,3.46453261665077));
#31529=CARTESIAN_POINT('Ctrl Pts',(372.760407137997,-11.0000000000001,3.51157458559606));
#31530=CARTESIAN_POINT('Ctrl Pts',(372.744424821001,-11.0000000000001,3.52244647340364));
#31531=CARTESIAN_POINT('Ctrl Pts',(372.72836292761,-11.0000000000001,3.53319989268987));
#31532=CARTESIAN_POINT('Ctrl Pts',(372.712230322745,-11.0000000000001,3.54382840352593));
#31533=CARTESIAN_POINT('Ctrl Pts',(372.60675817946,-11.,3.61331574467032));
#31534=CARTESIAN_POINT('Ctrl Pts',(372.498175010034,-11.0000000000002,3.67752958060433));
#31535=CARTESIAN_POINT('Ctrl Pts',(372.386777109338,-11.0000000000001,3.73612797973573));
#31536=CARTESIAN_POINT('Ctrl Pts',(372.322300834232,-11.,3.77004429664692));
#31537=CARTESIAN_POINT('Ctrl Pts',(372.256880848245,-11.,3.80207888043325));
#31538=CARTESIAN_POINT('Ctrl Pts',(372.190568937043,-11.0000000000001,3.83215976551742));
#31539=CARTESIAN_POINT('Ctrl Pts',(372.094043909479,-11.0000000000001,3.87594614128781));
#31540=CARTESIAN_POINT('Ctrl Pts',(371.995629603314,-11.,3.91559422951229));
#31541=CARTESIAN_POINT('Ctrl Pts',(371.895579440434,-11.,3.95116325459089));
#31542=CARTESIAN_POINT('Ctrl Pts',(373.408085425102,-16.0015042489531,-2.20592963361204));
#31543=CARTESIAN_POINT('Ctrl Pts',(373.397699055235,-16.0010028326354,-2.21804792675504));
#31544=CARTESIAN_POINT('Ctrl Pts',(373.387227097536,-16.0005014163177,-2.23009286410093));
#31545=CARTESIAN_POINT('Ctrl Pts',(373.376670596656,-16.,-2.2420632440818));
#31546=CARTESIAN_POINT('Ctrl Pts',(369.776711150535,-11.0016404554735,3.94875541723466));
#31547=CARTESIAN_POINT('Ctrl Pts',(368.500032745302,-11.0659606286233,3.60684744968143));
#31548=CARTESIAN_POINT('Ctrl Pts',(366.323554905574,-11.1945832157571,1.59361640613361));
#31549=CARTESIAN_POINT('Ctrl Pts',(366.965591470948,-11.3875082168749,-2.82400952883738));
#31550=CARTESIAN_POINT('Ctrl Pts',(370.975575282479,-11.5804154588268,-4.78528756048741));
#31551=CARTESIAN_POINT('Ctrl Pts',(374.860019939513,-11.7733227007787,-2.59106421286309));
#31552=CARTESIAN_POINT('Ctrl Pts',(375.248154941599,-11.9662299427307,1.85501048073415));
#31553=CARTESIAN_POINT('Ctrl Pts',(371.800788741178,-12.1591371846826,4.68898826029466));
#31554=CARTESIAN_POINT('Ctrl Pts',(367.514000337472,-12.3520444266345,3.44915361081735));
#31555=CARTESIAN_POINT('Ctrl Pts',(366.111896528258,-12.5449516685864,-0.787508517572457));
#31556=CARTESIAN_POINT('Ctrl Pts',(368.812861501212,-12.7378589105384,-4.33992202873321));
#31557=CARTESIAN_POINT('Ctrl Pts',(373.270113906834,-12.9307661524903,-4.1216707895165));
#31558=CARTESIAN_POINT('Ctrl Pts',(375.611071197946,-13.1236733944423,-0.322356367943754));
#31559=CARTESIAN_POINT('Ctrl Pts',(373.801807325092,-13.3165806363942,3.75702963470999));
#31560=CARTESIAN_POINT('Ctrl Pts',(369.41428424138,-13.5094878783461,4.57217420235261));
#31561=CARTESIAN_POINT('Ctrl Pts',(366.260536257966,-13.702395120298,1.41484854707178));
#31562=CARTESIAN_POINT('Ctrl Pts',(367.080655435926,-13.89530236225,-2.97174878689068));
#31563=CARTESIAN_POINT('Ctrl Pts',(371.162091027228,-14.0882096042019,-4.77638254206457));
#31564=CARTESIAN_POINT('Ctrl Pts',(374.958746867641,-14.2811168461538,-2.43112555194102));
#31565=CARTESIAN_POINT('Ctrl Pts',(375.171947262906,-14.4740240881058,2.02638683774903));
#31566=CARTESIAN_POINT('Ctrl Pts',(371.616465052591,-14.6669313300577,4.72328855323263));
#31567=CARTESIAN_POINT('Ctrl Pts',(367.381412119708,-14.8598385720096,3.31645516043818));
#31568=CARTESIAN_POINT('Ctrl Pts',(366.146398234732,-15.0527458139616,-0.971894380569737));
#31569=CARTESIAN_POINT('Ctrl Pts',(368.98435744238,-15.2456530559135,-4.41569058707157));
#31570=CARTESIAN_POINT('Ctrl Pts',(373.429777663597,-15.4385602978654,-4.02325864183314));
#31571=CARTESIAN_POINT('Ctrl Pts',(375.619897415873,-15.6314675398174,-0.134607920621325));
#31572=CARTESIAN_POINT('Ctrl Pts',(373.652897933972,-15.8243747817693,3.86969469419586));
#31573=CARTESIAN_POINT('Ctrl Pts',(369.235897717888,-16.0172820237212,4.51521059429547));
#31574=CARTESIAN_POINT('Ctrl Pts',(366.211885374231,-16.2101892656732,1.23202454967953));
#31575=CARTESIAN_POINT('Ctrl Pts',(366.870979860592,-16.3387940936411,-1.6580058124492));
#31576=CARTESIAN_POINT('Ctrl Pts',(367.731076742204,-16.4030965076251,-2.66103287896124));
#31577=CARTESIAN_POINT('Ctrl Pts',(369.837283293296,-10.8664668332409,3.72259896771894));
#31578=CARTESIAN_POINT('Ctrl Pts',(368.633723890076,-10.9307870063907,3.40027304155158));
#31579=CARTESIAN_POINT('Ctrl Pts',(366.58189912421,-11.0594095935245,1.50234546371763));
#31580=CARTESIAN_POINT('Ctrl Pts',(367.187164430099,-11.2523345946423,-2.66227047413349));
#31581=CARTESIAN_POINT('Ctrl Pts',(370.967485067894,-11.4452418365942,-4.51122053676947));
#31582=CARTESIAN_POINT('Ctrl Pts',(374.629456535493,-11.6381490785461,-2.44266659869565));
#31583=CARTESIAN_POINT('Ctrl Pts',(374.995361942496,-11.8310563204981,1.74876875649206));
#31584=CARTESIAN_POINT('Ctrl Pts',(371.745436205636,-12.02396356245,4.42043657128886));
#31585=CARTESIAN_POINT('Ctrl Pts',(367.704164361648,-12.2168708044019,3.25161077718117));
#31586=CARTESIAN_POINT('Ctrl Pts',(366.382363023932,-12.4097780463539,-0.742405665792816));
#31587=CARTESIAN_POINT('Ctrl Pts',(368.928636053727,-12.6026852883058,-4.09136235524481));
#31588=CARTESIAN_POINT('Ctrl Pts',(373.130608941592,-12.7955925302577,-3.88561098501168));
#31589=CARTESIAN_POINT('Ctrl Pts',(375.337492953028,-12.9884997722097,-0.303894102254988));
#31590=CARTESIAN_POINT('Ctrl Pts',(373.631850766121,-13.1814070141616,3.54185386585814));
#31591=CARTESIAN_POINT('Ctrl Pts',(369.495613603651,-13.3743142561135,4.3103127865611));
#31592=CARTESIAN_POINT('Ctrl Pts',(366.522489733719,-13.5672214980655,1.33381614820207));
#31593=CARTESIAN_POINT('Ctrl Pts',(367.295638354663,-13.7601287400174,-2.80154828483818));
#31594=CARTESIAN_POINT('Ctrl Pts',(371.143318525656,-13.9530359819693,-4.5028255340697));
#31595=CARTESIAN_POINT('Ctrl Pts',(374.722529091754,-14.1459432239212,-2.2918880796088));
#31596=CARTESIAN_POINT('Ctrl Pts',(374.923518894229,-14.3388504658732,1.9103299022978));
#31597=CARTESIAN_POINT('Ctrl Pts',(371.571669258747,-14.5317577078251,4.45277238893056));
#31598=CARTESIAN_POINT('Ctrl Pts',(367.57916984808,-14.724664949777,3.12651234433233));
#31599=CARTESIAN_POINT('Ctrl Pts',(366.414888719584,-14.917572191729,-0.916231226185798));
#31600=CARTESIAN_POINT('Ctrl Pts',(369.090309934762,-15.1104794336809,-4.16279143282831));
#31601=CARTESIAN_POINT('Ctrl Pts',(373.281128301063,-15.3033866756328,-3.79283518082333));
#31602=CARTESIAN_POINT('Ctrl Pts',(375.345813668361,-15.4962939175848,-0.126898542301376));
#31603=CARTESIAN_POINT('Ctrl Pts',(373.491469839196,-15.6892011595367,3.64806627706739));
#31604=CARTESIAN_POINT('Ctrl Pts',(369.327443783533,-15.8821084014886,4.25661164629155));
#31605=CARTESIAN_POINT('Ctrl Pts',(366.476625224416,-16.0750156434406,1.16146300093036));
#31606=CARTESIAN_POINT('Ctrl Pts',(367.097971495661,-16.2036204714085,-1.56304710566696));
#31607=CARTESIAN_POINT('Ctrl Pts',(367.908808183507,-16.2679228853925,-2.50862796035731));
#31608=CARTESIAN_POINT('Ctrl Pts',(369.897855436059,-10.7312932110083,3.49644251820321));
#31609=CARTESIAN_POINT('Ctrl Pts',(368.767415034851,-10.7956133841581,3.19369863342172));
#31610=CARTESIAN_POINT('Ctrl Pts',(366.840243342845,-10.9242359712918,1.41107452130166));
#31611=CARTESIAN_POINT('Ctrl Pts',(367.408737389251,-11.1171609724097,-2.50053141942959));
#31612=CARTESIAN_POINT('Ctrl Pts',(370.95939485331,-11.3100682143616,-4.23715351305153));
#31613=CARTESIAN_POINT('Ctrl Pts',(374.398893131472,-11.5029754563135,-2.29426898452822));
#31614=CARTESIAN_POINT('Ctrl Pts',(374.742568943392,-11.6958826982655,1.64252703224997));
#31615=CARTESIAN_POINT('Ctrl Pts',(371.690083670094,-11.8887899402174,4.15188488228307));
#31616=CARTESIAN_POINT('Ctrl Pts',(367.894328385824,-12.0816971821693,3.05406794354497));
#31617=CARTESIAN_POINT('Ctrl Pts',(366.652829519606,-12.2746044241213,-0.697302814013183));
#31618=CARTESIAN_POINT('Ctrl Pts',(369.044410606242,-12.4675116660732,-3.84280268175641));
#31619=CARTESIAN_POINT('Ctrl Pts',(372.991103976351,-12.6604189080251,-3.64955118050687));
#31620=CARTESIAN_POINT('Ctrl Pts',(375.063914708111,-12.8533261499771,-0.285431836566218));
#31621=CARTESIAN_POINT('Ctrl Pts',(373.461894207149,-13.046233391929,3.32667809700629));
#31622=CARTESIAN_POINT('Ctrl Pts',(369.576942965922,-13.2391406338809,4.0484513707696));
#31623=CARTESIAN_POINT('Ctrl Pts',(366.784443209472,-13.4320478758329,1.25278374933238));
#31624=CARTESIAN_POINT('Ctrl Pts',(367.5106212734,-13.6249551177848,-2.63134778278569));
#31625=CARTESIAN_POINT('Ctrl Pts',(371.124546024083,-13.8178623597367,-4.22926852607485));
#31626=CARTESIAN_POINT('Ctrl Pts',(374.486311315867,-14.0107696016886,-2.15265060727657));
#31627=CARTESIAN_POINT('Ctrl Pts',(374.675090525552,-14.2036768436406,1.79427296684655));
#31628=CARTESIAN_POINT('Ctrl Pts',(371.526873464904,-14.3965840855925,4.18225622462848));
#31629=CARTESIAN_POINT('Ctrl Pts',(367.776927576449,-14.5894913275444,2.93656952822648));
#31630=CARTESIAN_POINT('Ctrl Pts',(366.683379204436,-14.7823985694964,-0.860568071801865));
#31631=CARTESIAN_POINT('Ctrl Pts',(369.196262427144,-14.9753058114483,-3.90989227858506));
#31632=CARTESIAN_POINT('Ctrl Pts',(373.13247893853,-15.1682130534002,-3.56241171981353));
#31633=CARTESIAN_POINT('Ctrl Pts',(375.071729920849,-15.3611202953522,-0.119189163981424));
#31634=CARTESIAN_POINT('Ctrl Pts',(373.330041744421,-15.5540275373041,3.42643785993892));
#31635=CARTESIAN_POINT('Ctrl Pts',(369.418989849177,-15.746934779256,3.99801269828764));
#31636=CARTESIAN_POINT('Ctrl Pts',(366.741365074601,-15.939842021208,1.0909014521812));
#31637=CARTESIAN_POINT('Ctrl Pts',(367.32496313073,-16.0684468491759,-1.46808839888473));
#31638=CARTESIAN_POINT('Ctrl Pts',(368.086539624811,-16.1327492631599,-2.35622304175338));
#31639=CARTESIAN_POINT('Ctrl Pts',(369.958427578821,-10.5961195887756,3.27028606868749));
#31640=CARTESIAN_POINT('Ctrl Pts',(368.901106179625,-10.6604397619255,2.98712422529187));
#31641=CARTESIAN_POINT('Ctrl Pts',(367.09858756148,-10.7890623490592,1.31980357888569));
#31642=CARTESIAN_POINT('Ctrl Pts',(367.630310348403,-10.9819873501771,-2.33879236472568));
#31643=CARTESIAN_POINT('Ctrl Pts',(370.951304638724,-11.174894592129,-3.96308648933358));
#31644=CARTESIAN_POINT('Ctrl Pts',(374.168329727452,-11.3678018340809,-2.14587137036077));
#31645=CARTESIAN_POINT('Ctrl Pts',(374.48977594429,-11.5607090760329,1.53628530800788));
#31646=CARTESIAN_POINT('Ctrl Pts',(371.634731134551,-11.7536163179848,3.88333319327727));
#31647=CARTESIAN_POINT('Ctrl Pts',(368.084492409999,-11.9465235599367,2.85652510990878));
#31648=CARTESIAN_POINT('Ctrl Pts',(366.923296015279,-12.1394308018887,-0.652199962233542));
#31649=CARTESIAN_POINT('Ctrl Pts',(369.160185158757,-12.3323380438406,-3.59424300826801));
#31650=CARTESIAN_POINT('Ctrl Pts',(372.851599011108,-12.5252452857925,-3.41349137600206));
#31651=CARTESIAN_POINT('Ctrl Pts',(374.790336463194,-12.7181525277445,-0.266969570877453));
#31652=CARTESIAN_POINT('Ctrl Pts',(373.291937648178,-12.9110597696964,3.11150232815445));
#31653=CARTESIAN_POINT('Ctrl Pts',(369.658272328193,-13.1039670116483,3.78658995497808));
#31654=CARTESIAN_POINT('Ctrl Pts',(367.046396685226,-13.2968742536003,1.17175135046268));
#31655=CARTESIAN_POINT('Ctrl Pts',(367.725604192137,-13.4897814955522,-2.46114728073319));
#31656=CARTESIAN_POINT('Ctrl Pts',(371.105773522511,-13.6826887375041,-3.95571151807998));
#31657=CARTESIAN_POINT('Ctrl Pts',(374.25009353998,-13.875595979456,-2.01341313494433));
#31658=CARTESIAN_POINT('Ctrl Pts',(374.426662156873,-14.068503221408,1.67821603139532));
#31659=CARTESIAN_POINT('Ctrl Pts',(371.482077671061,-14.2614104633599,3.91174006032641));
#31660=CARTESIAN_POINT('Ctrl Pts',(367.974685304821,-14.4543177053119,2.74662671212062));
#31661=CARTESIAN_POINT('Ctrl Pts',(366.951869689287,-14.6472249472638,-0.804904917417929));
#31662=CARTESIAN_POINT('Ctrl Pts',(369.302214919525,-14.8401321892157,-3.6569931243418));
#31663=CARTESIAN_POINT('Ctrl Pts',(372.983829575995,-15.0330394311676,-3.33198825880372));
#31664=CARTESIAN_POINT('Ctrl Pts',(374.797646173337,-15.2259466731196,-0.111479785661475));
#31665=CARTESIAN_POINT('Ctrl Pts',(373.168613649646,-15.4188539150715,3.20480944281046));
#31666=CARTESIAN_POINT('Ctrl Pts',(369.510535914822,-15.6117611570234,3.73941375028372));
#31667=CARTESIAN_POINT('Ctrl Pts',(367.006104924786,-15.8046683989754,1.02033990343203));
#31668=CARTESIAN_POINT('Ctrl Pts',(367.551954765798,-15.9332732269433,-1.37312969210249));
#31669=CARTESIAN_POINT('Ctrl Pts',(368.264271066114,-15.9975756409273,-2.20381812314945));
#31670=CARTESIAN_POINT('Ctrl Pts',(368.26108342621,-16.,-2.20655152809223));
#31671=CARTESIAN_POINT('Ctrl Pts',(368.18351393423,-16.0000000000001,-2.13272830433258));
#31672=CARTESIAN_POINT('Ctrl Pts',(368.109969768842,-16.,-2.05517575529548));
#31673=CARTESIAN_POINT('Ctrl Pts',(368.040450579516,-16.,-1.9743250932332));
#31674=CARTESIAN_POINT('Ctrl Pts',(367.970931390189,-16.0000000000001,-1.89347443117091));
#31675=CARTESIAN_POINT('Ctrl Pts',(367.90543688921,-15.9999999999999,-1.80932506555908));
#31676=CARTESIAN_POINT('Ctrl Pts',(367.843991843118,-16.0000000000001,-1.72226169762899));
#31677=CARTESIAN_POINT('Ctrl Pts',(367.780009545896,-16.0000000000002,-1.63160322085558));
#31678=CARTESIAN_POINT('Ctrl Pts',(367.720417473432,-15.9999999999999,-1.53778471284877));
#31679=CARTESIAN_POINT('Ctrl Pts',(367.665277613433,-16.,-1.44119732543093));
#31680=CARTESIAN_POINT('Ctrl Pts',(367.614209007617,-16.0000000000002,-1.35174147235489));
#31681=CARTESIAN_POINT('Ctrl Pts',(367.566959548454,-15.9999999999999,-1.25990961252799));
#31682=CARTESIAN_POINT('Ctrl Pts',(367.523609095148,-16.0000000000001,-1.16598698107383));
#31683=CARTESIAN_POINT('Ctrl Pts',(367.515926948415,-16.0000000000002,-1.14934292359788));
#31684=CARTESIAN_POINT('Ctrl Pts',(367.508367324632,-16.0000000000002,-1.13263315829243));
#31685=CARTESIAN_POINT('Ctrl Pts',(367.500930774503,-16.0000000000001,-1.11585921181451));
#31686=CARTESIAN_POINT('Ctrl Pts',(367.494578290699,-16.0000000000001,-1.10153049467122));
#31687=CARTESIAN_POINT('Ctrl Pts',(367.488319489826,-15.9999999999999,-1.08716367391313));
#31688=CARTESIAN_POINT('Ctrl Pts',(367.482154851194,-15.9999999999999,-1.07276094050394));
#31689=CARTESIAN_POINT('Ctrl Pts',(367.437335864243,-15.9999999999999,-0.968048246163189));
#31690=CARTESIAN_POINT('Ctrl Pts',(367.397483434743,-16.0000000000001,-0.861423041830749));
#31691=CARTESIAN_POINT('Ctrl Pts',(367.362628908517,-16.0000000000001,-0.753314701397611));
#31692=CARTESIAN_POINT('Ctrl Pts',(367.327250685275,-16.,-0.643582009079649));
#31693=CARTESIAN_POINT('Ctrl Pts',(367.297021232921,-15.9999999999999,-0.532320566665647));
#31694=CARTESIAN_POINT('Ctrl Pts',(367.272012940965,-15.9999999999999,-0.419942953878413));
#31695=CARTESIAN_POINT('Ctrl Pts',(367.246780388205,-16.,-0.306557599580401));
#31696=CARTESIAN_POINT('Ctrl Pts',(367.226862603766,-16.0000000000001,-0.192035147049314));
#31697=CARTESIAN_POINT('Ctrl Pts',(367.21238076122,-16.,-0.0767742238126385));
#31698=CARTESIAN_POINT('Ctrl Pts',(367.20151937931,-15.9999999999999,0.00967146861486187));
#31699=CARTESIAN_POINT('Ctrl Pts',(367.193716638548,-16.,0.0965331551063391));
#31700=CARTESIAN_POINT('Ctrl Pts',(367.189043047261,-15.9999999999999,0.183647504944786));
#31701=CARTESIAN_POINT('Ctrl Pts',(367.188205453357,-15.9999999999999,0.199260005896969));
#31702=CARTESIAN_POINT('Ctrl Pts',(367.187468411071,-16.0000000000002,0.214880627304962));
#31703=CARTESIAN_POINT('Ctrl Pts',(367.186832386945,-16.0000000000001,0.230508433788787));
#31704=CARTESIAN_POINT('Ctrl Pts',(367.186154279982,-16.0000000000001,0.247170261477932));
#31705=CARTESIAN_POINT('Ctrl Pts',(367.185591387335,-16.0000000000002,0.263831136380812));
#31706=CARTESIAN_POINT('Ctrl Pts',(367.185143961572,-16.0000000000002,0.280486670524623));
#31707=CARTESIAN_POINT('Ctrl Pts',(367.181957809614,-16.0000000000002,0.399091961351293));
#31708=CARTESIAN_POINT('Ctrl Pts',(367.184621052563,-16.0000000000002,0.517476392994406));
#31709=CARTESIAN_POINT('Ctrl Pts',(367.193203833027,-16.0000000000002,0.635211876895126));
#31710=CARTESIAN_POINT('Ctrl Pts',(367.201208598629,-16.0000000000002,0.745018361601917));
#31711=CARTESIAN_POINT('Ctrl Pts',(367.214362617238,-16.0000000000002,0.854261226171659));
#31712=CARTESIAN_POINT('Ctrl Pts',(367.232761268974,-16.0000000000002,0.962606957926316));
#31713=CARTESIAN_POINT('Ctrl Pts',(367.25195269881,-16.0000000000001,1.07562119064931));
#31714=CARTESIAN_POINT('Ctrl Pts',(367.276849595831,-16.0000000000002,1.18766007996308));
#31715=CARTESIAN_POINT('Ctrl Pts',(367.307156117133,-16.0000000000002,1.29845750341952));
#31716=CARTESIAN_POINT('Ctrl Pts',(367.325946168543,-16.0000000000001,1.36715193595241));
#31717=CARTESIAN_POINT('Ctrl Pts',(367.346816757925,-15.9999999999999,1.4353691655699));
#31718=CARTESIAN_POINT('Ctrl Pts',(367.369707204142,-16.0000000000001,1.50304465908003));
#31719=CARTESIAN_POINT('Ctrl Pts',(367.381962978616,-16.0000000000002,1.53927879702795));
#31720=CARTESIAN_POINT('Ctrl Pts',(367.394797896825,-15.9999999999999,1.57535761633311));
#31721=CARTESIAN_POINT('Ctrl Pts',(367.408203471026,-15.9999999999999,1.61127100334885));
#31722=CARTESIAN_POINT('Ctrl Pts',(367.415902678343,-15.9999999999999,1.63189709574459));
#31723=CARTESIAN_POINT('Ctrl Pts',(367.423791800755,-16.0000000000001,1.65247261509346));
#31724=CARTESIAN_POINT('Ctrl Pts',(367.431858608384,-16.0000000000001,1.67296916741837));
#31725=CARTESIAN_POINT('Ctrl Pts',(367.475079373834,-16.0000000000003,1.78278667160836));
#31726=CARTESIAN_POINT('Ctrl Pts',(367.523445625448,-16.0000000000002,1.89047517580507));
#31727=CARTESIAN_POINT('Ctrl Pts',(367.576599392367,-16.0000000000002,1.99576259435056));
#31728=CARTESIAN_POINT('Ctrl Pts',(367.630702043565,-16.0000000000002,2.10292957067731));
#31729=CARTESIAN_POINT('Ctrl Pts',(367.689764924591,-16.0000000000001,2.20760965059624));
#31730=CARTESIAN_POINT('Ctrl Pts',(367.753465513287,-16.0000000000001,2.3095128047873));
#31731=CARTESIAN_POINT('Ctrl Pts',(367.818145691291,-16.0000000000001,2.41298302833227));
#31732=CARTESIAN_POINT('Ctrl Pts',(367.887607634854,-16.,2.5135910393457));
#31733=CARTESIAN_POINT('Ctrl Pts',(367.961565405332,-16.0000000000001,2.61101890964699));
#31734=CARTESIAN_POINT('Ctrl Pts',(368.010750766558,-16.0000000000001,2.67581298014525));
#31735=CARTESIAN_POINT('Ctrl Pts',(368.061925634854,-16.0000000000001,2.73920020650163));
#31736=CARTESIAN_POINT('Ctrl Pts',(368.115017126897,-16.,2.80108101804679));
#31737=CARTESIAN_POINT('Ctrl Pts',(368.133646696693,-16.,2.82279472119189));
#31738=CARTESIAN_POINT('Ctrl Pts',(368.15251233108,-15.9999999999999,2.84432289013815));
#31739=CARTESIAN_POINT('Ctrl Pts',(368.171611117157,-15.9999999999999,2.86566103888692));
#31740=CARTESIAN_POINT('Ctrl Pts',(368.183566345187,-15.9999999999999,2.8790180361859));
#31741=CARTESIAN_POINT('Ctrl Pts',(368.195613352392,-15.9999999999999,2.89230103112425));
#31742=CARTESIAN_POINT('Ctrl Pts',(368.207750166955,-15.9999999999999,2.905507509312));
#31743=CARTESIAN_POINT('Ctrl Pts',(368.292660099036,-15.9999999999999,2.99790087662829));
#31744=CARTESIAN_POINT('Ctrl Pts',(368.381671855022,-16.0000000000001,3.08623599275652));
#31745=CARTESIAN_POINT('Ctrl Pts',(368.47446003312,-16.,3.17018956350407));
#31746=CARTESIAN_POINT('Ctrl Pts',(368.549042802181,-15.9999999999999,3.23767111026241));
#31747=CARTESIAN_POINT('Ctrl Pts',(368.626066579836,-16.0000000000001,3.30232168162783));
#31748=CARTESIAN_POINT('Ctrl Pts',(368.705383680702,-16.,3.36396149445182));
#31749=CARTESIAN_POINT('Ctrl Pts',(368.77143344708,-16.,3.4152908445186));
#31750=CARTESIAN_POINT('Ctrl Pts',(368.839073876932,-15.9999999999999,3.46453229796807));
#31751=CARTESIAN_POINT('Ctrl Pts',(368.908228349274,-15.9999999999999,3.51157426867829));
#31752=CARTESIAN_POINT('Ctrl Pts',(368.924210666199,-15.9999999999999,3.52244615677451));
#31753=CARTESIAN_POINT('Ctrl Pts',(368.940272559512,-15.9999999999999,3.53319957636285));
#31754=CARTESIAN_POINT('Ctrl Pts',(368.956405164286,-15.9999999999999,3.54382808750964));
#31755=CARTESIAN_POINT('Ctrl Pts',(369.061877312563,-16.,3.6133154343693));
#31756=CARTESIAN_POINT('Ctrl Pts',(369.170460486771,-15.9999999999999,3.67752927585838));
#31757=CARTESIAN_POINT('Ctrl Pts',(369.28185839183,-16.,3.73612768018094));
#31758=CARTESIAN_POINT('Ctrl Pts',(369.346334673923,-16.,3.77004400244298));
#31759=CARTESIAN_POINT('Ctrl Pts',(369.411754666887,-16.,3.80207859119799));
#31760=CARTESIAN_POINT('Ctrl Pts',(369.478066585006,-16.,3.83215948081421));
#31761=CARTESIAN_POINT('Ctrl Pts',(369.574591622416,-16.0000000000001,3.87594586308027));
#31762=CARTESIAN_POINT('Ctrl Pts',(369.673005938295,-15.9999999999999,3.91559395689521));
#31763=CARTESIAN_POINT('Ctrl Pts',(369.773056110741,-16.,3.95116298671608));
#31764=CARTESIAN_POINT('Ctrl Pts',(369.776413430251,-11.,3.94563850749837));
#31765=CARTESIAN_POINT('Ctrl Pts',(369.659936027211,-10.9999999999999,3.90363340028023));
#31766=CARTESIAN_POINT('Ctrl Pts',(369.545849642241,-11.,3.85602145237529));
#31767=CARTESIAN_POINT('Ctrl Pts',(369.434387235882,-11.,3.80316525575889));
#31768=CARTESIAN_POINT('Ctrl Pts',(369.32129226132,-11.,3.74953488470336));
#31769=CARTESIAN_POINT('Ctrl Pts',(369.210898085145,-11.0000000000001,3.69050490441186));
#31770=CARTESIAN_POINT('Ctrl Pts',(369.103475688714,-11.,3.6264068078231));
#31771=CARTESIAN_POINT('Ctrl Pts',(368.995626170089,-11.,3.56205385079072));
#31772=CARTESIAN_POINT('Ctrl Pts',(368.890771532536,-11.0000000000001,3.49259169503417));
#31773=CARTESIAN_POINT('Ctrl Pts',(368.789222562421,-11.0000000000001,3.41831855725877));
#31774=CARTESIAN_POINT('Ctrl Pts',(368.69784886467,-11.0000000000001,3.3514876358389));
#31775=CARTESIAN_POINT('Ctrl Pts',(368.609151752929,-11.0000000000001,3.28076071756683));
#31776=CARTESIAN_POINT('Ctrl Pts',(368.523388576094,-11.0000000000001,3.20633646559006));
#31777=CARTESIAN_POINT('Ctrl Pts',(368.503754693478,-11.0000000000001,3.18929841871426));
#31778=CARTESIAN_POINT('Ctrl Pts',(368.484274710755,-11.0000000000001,3.17206653900113));
#31779=CARTESIAN_POINT('Ctrl Pts',(368.46495196076,-11.0000000000001,3.15464311726871));
#31780=CARTESIAN_POINT('Ctrl Pts',(368.451707859823,-11.0000000000001,3.14270084424112));
#31781=CARTESIAN_POINT('Ctrl Pts',(368.43853703285,-11.0000000000001,3.13066795174825));
#31782=CARTESIAN_POINT('Ctrl Pts',(368.425452636208,-11.0000000000001,3.11855657911232));
#31783=CARTESIAN_POINT('Ctrl Pts',(368.334977806957,-11.,3.03480993024135));
#31784=CARTESIAN_POINT('Ctrl Pts',(368.248492784418,-10.9999999999999,2.94718935218984));
#31785=CARTESIAN_POINT('Ctrl Pts',(368.16625722767,-10.9999999999999,2.85600833920122));
#31786=CARTESIAN_POINT('Ctrl Pts',(368.084366229379,-11.,2.76520936520406));
#31787=CARTESIAN_POINT('Ctrl Pts',(368.006688685184,-11.,2.67087899756665));
#31788=CARTESIAN_POINT('Ctrl Pts',(367.933523458788,-11.,2.57329789569913));
#31789=CARTESIAN_POINT('Ctrl Pts',(367.862060559945,-11.,2.47798720296711));
#31790=CARTESIAN_POINT('Ctrl Pts',(367.794902169971,-11.0000000000001,2.37957458681458));
#31791=CARTESIAN_POINT('Ctrl Pts',(367.732372661656,-11.,2.2783045497797));
#31792=CARTESIAN_POINT('Ctrl Pts',(367.681195946289,-10.9999999999999,2.19542099607579));
#31793=CARTESIAN_POINT('Ctrl Pts',(367.633120597113,-11.,2.11062295888144));
#31794=CARTESIAN_POINT('Ctrl Pts',(367.588350198513,-11.0000000000001,2.0240403948292));
#31795=CARTESIAN_POINT('Ctrl Pts',(367.577475074151,-11.0000000000001,2.00300872700656));
#31796=CARTESIAN_POINT('Ctrl Pts',(367.566795071804,-11.,1.98187175637645));
#31797=CARTESIAN_POINT('Ctrl Pts',(367.556313334115,-11.,1.96063133738065));
#31798=CARTESIAN_POINT('Ctrl Pts',(367.548771481207,-11.,1.94534836422111));
#31799=CARTESIAN_POINT('Ctrl Pts',(367.541332121455,-10.9999999999999,1.9300113651976));
#31800=CARTESIAN_POINT('Ctrl Pts',(367.534002940154,-10.9999999999999,1.91463508225276));
#31801=CARTESIAN_POINT('Ctrl Pts',(367.482865177981,-10.9999999999999,1.8073504254668));
#31802=CARTESIAN_POINT('Ctrl Pts',(367.437005313807,-11.0000000000001,1.69799133979778));
#31803=CARTESIAN_POINT('Ctrl Pts',(367.39670398105,-11.0000000000001,1.58682023789595));
#31804=CARTESIAN_POINT('Ctrl Pts',(367.356402648294,-11.0000000000002,1.47564913599412));
#31805=CARTESIAN_POINT('Ctrl Pts',(367.321659401167,-10.9999999999998,1.36266534775552));
#31806=CARTESIAN_POINT('Ctrl Pts',(367.292809505677,-11.,1.24811926023833));
#31807=CARTESIAN_POINT('Ctrl Pts',(367.263881051474,-11.0000000000001,1.13326126194863));
#31808=CARTESIAN_POINT('Ctrl Pts',(367.240878654116,-11.,1.01683139042499));
#31809=CARTESIAN_POINT('Ctrl Pts',(367.223722412658,-11.0000000000001,0.899263114940381));
#31810=CARTESIAN_POINT('Ctrl Pts',(367.214331524928,-11.0000000000001,0.834909248245439));
#31811=CARTESIAN_POINT('Ctrl Pts',(367.206693171909,-11.,0.770214393798156));
#31812=CARTESIAN_POINT('Ctrl Pts',(367.200800614037,-11.0000000000001,0.705251301586698));
#31813=CARTESIAN_POINT('Ctrl Pts',(367.197577909856,-11.0000000000001,0.669722277786365));
#31814=CARTESIAN_POINT('Ctrl Pts',(367.194877469672,-11.,0.634113048489866));
#31815=CARTESIAN_POINT('Ctrl Pts',(367.192698731357,-11.,0.598435759622394));
#31816=CARTESIAN_POINT('Ctrl Pts',(367.191630998276,-10.9999999999999,0.580951410386367));
#31817=CARTESIAN_POINT('Ctrl Pts',(367.190688485058,-11.0000000000002,0.563448935452259));
#31818=CARTESIAN_POINT('Ctrl Pts',(367.189871415751,-11.0000000000002,0.545935383445549));
#31819=CARTESIAN_POINT('Ctrl Pts',(367.184455247748,-11.0000000000001,0.429842000501809));
#31820=CARTESIAN_POINT('Ctrl Pts',(367.184562980828,-11.,0.313635830102158));
#31821=CARTESIAN_POINT('Ctrl Pts',(367.190059552093,-11.,0.197720677411417));
#31822=CARTESIAN_POINT('Ctrl Pts',(367.195570191111,-11.0000000000001,0.0815088550914429));
#31823=CARTESIAN_POINT('Ctrl Pts',(367.206497586919,-11.0000000000002,-0.0344113712345558));
#31824=CARTESIAN_POINT('Ctrl Pts',(367.222757524567,-11.,-0.149624567530818));
#31825=CARTESIAN_POINT('Ctrl Pts',(367.23886744374,-10.9999999999998,-0.263774776481907));
#31826=CARTESIAN_POINT('Ctrl Pts',(367.260212326853,-10.9999999999998,-0.377231769472658));
#31827=CARTESIAN_POINT('Ctrl Pts',(367.286756024338,-11.,-0.489570218199307));
#31828=CARTESIAN_POINT('Ctrl Pts',(367.303418137215,-11.0000000000001,-0.560087745541271));
#31829=CARTESIAN_POINT('Ctrl Pts',(367.322129666626,-11.0000000000001,-0.630164056870382));
#31830=CARTESIAN_POINT('Ctrl Pts',(367.342890066273,-10.9999999999999,-0.699687414794692));
#31831=CARTESIAN_POINT('Ctrl Pts',(367.353981140095,-10.9999999999999,-0.736829700502522));
#31832=CARTESIAN_POINT('Ctrl Pts',(367.365657097148,-10.9999999999998,-0.773814068645216));
#31833=CARTESIAN_POINT('Ctrl Pts',(367.377918561647,-10.9999999999998,-0.810622743611728));
#31834=CARTESIAN_POINT('Ctrl Pts',(367.384026834972,-10.9999999999998,-0.828959659847157));
#31835=CARTESIAN_POINT('Ctrl Pts',(367.390281141698,-10.9999999999999,-0.847254832709461));
#31836=CARTESIAN_POINT('Ctrl Pts',(367.396675594858,-10.9999999999999,-0.865489433129636));
#31837=CARTESIAN_POINT('Ctrl Pts',(367.433931723564,-11.0000000000001,-0.971730045597848));
#31838=CARTESIAN_POINT('Ctrl Pts',(367.475980154013,-10.9999999999999,-1.07603545527335));
#31839=CARTESIAN_POINT('Ctrl Pts',(367.522771858589,-10.9999999999999,-1.17800551424189));
#31840=CARTESIAN_POINT('Ctrl Pts',(367.557827270384,-10.9999999999999,-1.25439944860171));
#31841=CARTESIAN_POINT('Ctrl Pts',(367.595545867583,-10.9999999999998,-1.3294822107516));
#31842=CARTESIAN_POINT('Ctrl Pts',(367.635921634894,-11.,-1.40307299805944));
#31843=CARTESIAN_POINT('Ctrl Pts',(367.656229785332,-11.,-1.44008759565322));
#31844=CARTESIAN_POINT('Ctrl Pts',(367.677210355633,-10.9999999999997,-1.47672455143805));
#31845=CARTESIAN_POINT('Ctrl Pts',(367.698863683305,-10.9999999999999,-1.51295958259568));
#31846=CARTESIAN_POINT('Ctrl Pts',(367.711114888811,-11.0000000000001,-1.53346094940336));
#31847=CARTESIAN_POINT('Ctrl Pts',(367.723581468232,-11.,-1.55383363697344));
#31848=CARTESIAN_POINT('Ctrl Pts',(367.736263582017,-10.9999999999999,-1.57407311170418));
#31849=CARTESIAN_POINT('Ctrl Pts',(367.745854445896,-10.9999999999998,-1.58937923893319));
#31850=CARTESIAN_POINT('Ctrl Pts',(367.755567557301,-10.9999999999999,-1.60460745687454));
#31851=CARTESIAN_POINT('Ctrl Pts',(367.765397959284,-10.9999999999999,-1.6197484253644));
#31852=CARTESIAN_POINT('Ctrl Pts',(367.824091279774,-10.9999999999999,-1.71014897231997));
#31853=CARTESIAN_POINT('Ctrl Pts',(367.887011001249,-10.9999999999998,-1.79751936273579));
#31854=CARTESIAN_POINT('Ctrl Pts',(367.954135881222,-10.9999999999999,-1.88147688145987));
#31855=CARTESIAN_POINT('Ctrl Pts',(367.991442551067,-11.,-1.928138796286));
#31856=CARTESIAN_POINT('Ctrl Pts',(368.030048780959,-10.9999999999999,-1.97374586887409));
#31857=CARTESIAN_POINT('Ctrl Pts',(368.069955304757,-10.9999999999999,-2.0182269070666));
#31858=CARTESIAN_POINT('Ctrl Pts',(368.129331934719,-10.9999999999999,-2.08440992412033));
#31859=CARTESIAN_POINT('Ctrl Pts',(368.191587073976,-10.9999999999998,-2.14810094809532));
#31860=CARTESIAN_POINT('Ctrl Pts',(368.256517833619,-11.,-2.20920453143733));
#31861=CARTESIAN_POINT('Origin',(370.834317853224,-11.,1.11022302462516E-15));
#31862=CARTESIAN_POINT('',(377.834317853224,-11.,4.0414518843274));
#31863=CARTESIAN_POINT('',(377.834317853224,-11.,-4.04145188432739));
#31864=CARTESIAN_POINT('',(377.834317853224,-11.,4.0414518843274));
#31865=CARTESIAN_POINT('',(370.834317853224,-11.,-8.08290376865479));
#31866=CARTESIAN_POINT('',(377.834317853224,-11.,-4.04145188432739));
#31867=CARTESIAN_POINT('',(363.834317853224,-11.,-4.0414518843274));
#31868=CARTESIAN_POINT('',(370.834317853224,-11.,-8.08290376865479));
#31869=CARTESIAN_POINT('',(363.834317853224,-11.,4.0414518843274));
#31870=CARTESIAN_POINT('',(363.834317853224,-11.,-4.0414518843274));
#31871=CARTESIAN_POINT('',(370.834317853224,-11.,8.08290376865479));
#31872=CARTESIAN_POINT('',(363.834317853224,-11.,4.0414518843274));
#31873=CARTESIAN_POINT('',(370.834317853224,-11.,8.08290376865479));
#31874=CARTESIAN_POINT('Origin',(370.834317853224,-11.,-8.08290376865479));
#31875=CARTESIAN_POINT('',(377.834317853224,-16.,-4.04145188432739));
#31876=CARTESIAN_POINT('',(377.834317853224,-11.,-4.04145188432739));
#31877=CARTESIAN_POINT('',(370.834317853224,-16.,-8.08290376865479));
#31878=CARTESIAN_POINT('',(377.834317853224,-16.,-4.04145188432739));
#31879=CARTESIAN_POINT('',(370.834317853224,-11.,-8.08290376865479));
#31880=CARTESIAN_POINT('Origin',(363.834317853224,-11.,-4.0414518843274));
#31881=CARTESIAN_POINT('',(363.834317853224,-16.,-4.0414518843274));
#31882=CARTESIAN_POINT('',(370.834317853224,-16.,-8.08290376865479));
#31883=CARTESIAN_POINT('',(363.834317853224,-11.,-4.0414518843274));
#31884=CARTESIAN_POINT('Origin',(363.834317853224,-11.,4.0414518843274));
#31885=CARTESIAN_POINT('',(363.834317853224,-16.,4.0414518843274));
#31886=CARTESIAN_POINT('',(363.834317853224,-16.,-4.0414518843274));
#31887=CARTESIAN_POINT('',(363.834317853224,-11.,4.0414518843274));
#31888=CARTESIAN_POINT('Origin',(370.834317853224,-11.,8.08290376865479));
#31889=CARTESIAN_POINT('',(370.834317853224,-16.,8.08290376865479));
#31890=CARTESIAN_POINT('',(363.834317853224,-16.,4.0414518843274));
#31891=CARTESIAN_POINT('',(370.834317853224,-11.,8.08290376865479));
#31892=CARTESIAN_POINT('Origin',(377.834317853224,-11.,4.0414518843274));
#31893=CARTESIAN_POINT('',(377.834317853224,-16.,4.0414518843274));
#31894=CARTESIAN_POINT('',(370.834317853224,-16.,8.08290376865479));
#31895=CARTESIAN_POINT('',(377.834317853224,-11.,4.0414518843274));
#31896=CARTESIAN_POINT('Origin',(377.834317853224,-11.,-4.04145188432739));
#31897=CARTESIAN_POINT('',(377.834317853224,-16.,4.0414518843274));
#31898=CARTESIAN_POINT('Origin',(370.834317853224,-16.,1.11022302462516E-15));
#31899=CARTESIAN_POINT('',(0.,0.,0.));
#31900=CARTESIAN_POINT('Origin',(370.834317853224,2.31077344927308,0.));
#31901=CARTESIAN_POINT('',(372.309820613641,-0.653742688831811,2.86513684952401));
#31902=CARTESIAN_POINT('',(372.309820610785,-0.410425323647664,2.8651368509949));
#31903=CARTESIAN_POINT('',(372.309820613641,2.31077344927308,2.86513684952399));
#31904=CARTESIAN_POINT('',(368.962795093421,-8.08730439136318E-5,-2.62364634088498));
#31905=CARTESIAN_POINT('Ctrl Pts',(368.962795093421,-8.08730439141314E-5,
-2.62364634088498));
#31906=CARTESIAN_POINT('Ctrl Pts',(369.042935960825,-0.00619260378656188,
-2.68081313771997));
#31907=CARTESIAN_POINT('Ctrl Pts',(369.125848866233,-0.0123043345292098,
-2.73441167961165));
#31908=CARTESIAN_POINT('Ctrl Pts',(369.211178937621,-0.0184160652718575,
-2.78415833298928));
#31909=CARTESIAN_POINT('Ctrl Pts',(369.2963967607,-0.0245197562763533,-2.83383954662751));
#31910=CARTESIAN_POINT('Ctrl Pts',(369.384025052725,-0.030623447280849,
-2.87967871727806));
#31911=CARTESIAN_POINT('Ctrl Pts',(369.473678013242,-0.0367271382853449,
-2.92143402943727));
#31912=CARTESIAN_POINT('Ctrl Pts',(369.564719999829,-0.0429253960044152,
-2.9638362719021));
#31913=CARTESIAN_POINT('Ctrl Pts',(369.657849557319,-0.0491236537234856,
-3.00202675452611));
#31914=CARTESIAN_POINT('Ctrl Pts',(369.752634214727,-0.0553219114425558,
-3.03579941180366));
#31915=CARTESIAN_POINT('Ctrl Pts',(369.845818119595,-0.0614154910728362,
-3.06900170602479));
#31916=CARTESIAN_POINT('Ctrl Pts',(369.940601220424,-0.0675090707031168,
-3.09793407947053));
#31917=CARTESIAN_POINT('Ctrl Pts',(370.036551456481,-0.0736026503333971,
-3.12244877279476));
#31918=CARTESIAN_POINT('Ctrl Pts',(370.132472827969,-0.0796943968410773,
-3.14695609139985));
#31919=CARTESIAN_POINT('Ctrl Pts',(370.22956020778,-0.0857861433487573,
-3.16704826003044));
#31920=CARTESIAN_POINT('Ctrl Pts',(370.327367221206,-0.0918778898564376,
-3.18262762810807));
#31921=CARTESIAN_POINT('Ctrl Pts',(370.42517220408,-0.0979695098945485,
-3.19820667274545));
#31922=CARTESIAN_POINT('Ctrl Pts',(370.523696352617,-0.10406112993266,-3.20927303428268));
#31923=CARTESIAN_POINT('Ctrl Pts',(370.622485092656,-0.110152749970771,
-3.21578053418605));
#31924=CARTESIAN_POINT('Ctrl Pts',(370.724291754657,-0.116430464435126,
-3.22248683333383));
#31925=CARTESIAN_POINT('Ctrl Pts',(370.826378937163,-0.12270817889948,-3.22435118160919));
#31926=CARTESIAN_POINT('Ctrl Pts',(370.92824739925,-0.128985893363835,-3.22138088447847));
#31927=CARTESIAN_POINT('Ctrl Pts',(371.027231138184,-0.135085834767833,
-3.21849470057305));
#31928=CARTESIAN_POINT('Ctrl Pts',(371.126007932765,-0.141185776171832,
-3.21104412286963));
#31929=CARTESIAN_POINT('Ctrl Pts',(371.224125029667,-0.14728571757583,-3.19908860891562));
#31930=CARTESIAN_POINT('Ctrl Pts',(371.326531325948,-0.153652318570363,
-3.1866104583911));
#31931=CARTESIAN_POINT('Ctrl Pts',(371.428218392319,-0.160018919564898,
-3.16922461802616));
#31932=CARTESIAN_POINT('Ctrl Pts',(371.528685253602,-0.166385520559431,
-3.14705759016134));
#31933=CARTESIAN_POINT('Ctrl Pts',(371.629152114885,-0.172752121553965,
-3.12489056229652));
#31934=CARTESIAN_POINT('Ctrl Pts',(371.728398269154,-0.179118722548498,
-3.09794256249782));
#31935=CARTESIAN_POINT('Ctrl Pts',(371.825944479095,-0.185485323543031,
-3.06639759283822));
#31936=CARTESIAN_POINT('Ctrl Pts',(371.920678070301,-0.191668351836518,
-3.03576218155833));
#31937=CARTESIAN_POINT('Ctrl Pts',(372.014150842681,-0.197851380130005,
-3.00068080518707));
#31938=CARTESIAN_POINT('Ctrl Pts',(372.105916159122,-0.204034408423493,
-2.96127595994333));
#31939=CARTESIAN_POINT('Ctrl Pts',(372.197560363708,-0.210209276356962,
-2.92192312120972));
#31940=CARTESIAN_POINT('Ctrl Pts',(372.28750119774,-0.216384144290432,-2.87825832568418));
#31941=CARTESIAN_POINT('Ctrl Pts',(372.3753076588,-0.222559012223901,-2.83045367063467));
#31942=CARTESIAN_POINT('Ctrl Pts',(372.463023906512,-0.228727536028343,
-2.78269813062746));
#31943=CARTESIAN_POINT('Ctrl Pts',(372.548609763428,-0.234896059832786,
-2.73081139385581));
#31944=CARTESIAN_POINT('Ctrl Pts',(372.631655553263,-0.241064583637228,
-2.67501303819596));
#31945=CARTESIAN_POINT('Ctrl Pts',(372.714643792911,-0.247228832695148,
-2.61925335043047));
#31946=CARTESIAN_POINT('Ctrl Pts',(372.795095107198,-0.253393081753067,
-2.55958767389374));
#31947=CARTESIAN_POINT('Ctrl Pts',(372.872626497259,-0.259557330810986,
-2.49628031962563));
#31948=CARTESIAN_POINT('Ctrl Pts',(372.95013027197,-0.265719384269131,-2.43299551435116));
#31949=CARTESIAN_POINT('Ctrl Pts',(373.024715854482,-0.271881437727276,
-2.36607188230146));
#31950=CARTESIAN_POINT('Ctrl Pts',(373.096031916775,-0.278043491185421,
-2.29581511826106));
#31951=CARTESIAN_POINT('Ctrl Pts',(373.167341459047,-0.284204981282239,
-2.22556477739504));
#31952=CARTESIAN_POINT('Ctrl Pts',(373.23538176733,-0.290366471379056,-2.15198221408947));
#31953=CARTESIAN_POINT('Ctrl Pts',(373.299837822902,-0.296527961475873,
-2.0754105236363));
#31954=CARTESIAN_POINT('Ctrl Pts',(373.364305050632,-0.302690519542834,
-1.99882556102363));
#31955=CARTESIAN_POINT('Ctrl Pts',(373.425186512842,-0.308853077609796,
-1.91925077292984));
#31956=CARTESIAN_POINT('Ctrl Pts',(373.482207625686,-0.315015635676757,
-1.83706214249607));
#31957=CARTESIAN_POINT('Ctrl Pts',(373.539290208567,-0.321184837119358,
-1.75478491087762));
#31958=CARTESIAN_POINT('Ctrl Pts',(373.592503885071,-0.32735403856196,-1.66988856632607));
#31959=CARTESIAN_POINT('Ctrl Pts',(373.641617630156,-0.333523240004562,
-1.58277778760532));
#31960=CARTESIAN_POINT('Ctrl Pts',(373.690759303387,-0.339695949515255,
-1.49561747402238));
#31961=CARTESIAN_POINT('Ctrl Pts',(373.735796207269,-0.345868659025948,
-1.40624060465145));
#31962=CARTESIAN_POINT('Ctrl Pts',(373.776544422404,-0.352041368536641,
-1.31507428615635));
#31963=CARTESIAN_POINT('Ctrl Pts',(373.817360096113,-0.358224296953289,
-1.22375704203721));
#31964=CARTESIAN_POINT('Ctrl Pts',(373.853872741553,-0.364407225369936,
-1.13064483440963));
#31965=CARTESIAN_POINT('Ctrl Pts',(373.885947451266,-0.370590153786584,
-1.0361825895349));
#31966=CARTESIAN_POINT('Ctrl Pts',(373.909138357678,-0.375060582842619,
-0.967883761579969));
#31967=CARTESIAN_POINT('Ctrl Pts',(373.930010291673,-0.379531011898653,
-0.898879524300233));
#31968=CARTESIAN_POINT('Ctrl Pts',(373.948528930951,-0.384001440954687,
-0.82934126019565));
#31969=CARTESIAN_POINT('Ctrl Pts',(373.974081285622,-0.390169820124149,
-0.73339110095887));
#31970=CARTESIAN_POINT('Ctrl Pts',(373.99524054492,-0.39633819929361,-0.636088204984949));
#31971=CARTESIAN_POINT('Ctrl Pts',(374.011865918383,-0.402506578463071,
-0.537871598155227));
#31972=CARTESIAN_POINT('Ctrl Pts',(374.02846865233,-0.408666557873949,-0.439788737284304));
#31973=CARTESIAN_POINT('Ctrl Pts',(374.04054969955,-0.414826537284827,-0.340795063600563));
#31974=CARTESIAN_POINT('Ctrl Pts',(374.048018338277,-0.420986516695705,
-0.241343644769002));
#31975=CARTESIAN_POINT('Ctrl Pts',(374.055479021015,-0.427139934171043,
-0.141998166843434));
#31976=CARTESIAN_POINT('Ctrl Pts',(374.058337030795,-0.433293351646382,
-0.0421963445112613));
#31977=CARTESIAN_POINT('Ctrl Pts',(374.056553059645,-0.43944676912172,0.0576006683885499));
#31978=CARTESIAN_POINT('Ctrl Pts',(374.054770404537,-0.445595647201025,
0.157324060708199));
#31979=CARTESIAN_POINT('Ctrl Pts',(374.048352584441,-0.45174452528033,0.257042217049845));
#31980=CARTESIAN_POINT('Ctrl Pts',(374.037312330982,-0.457893403359635,
0.356291927990994));
#31981=CARTESIAN_POINT('Ctrl Pts',(374.026276302402,-0.464039928388644,
0.455503658090972));
#31982=CARTESIAN_POINT('Ctrl Pts',(374.010621403199,-0.470186453417652,
0.554246867132558));
#31983=CARTESIAN_POINT('Ctrl Pts',(373.990412322606,-0.476332978446661,
0.652062315150099));
#31984=CARTESIAN_POINT('Ctrl Pts',(373.97020555113,-0.482478801165025,0.749866586636176));
#31985=CARTESIAN_POINT('Ctrl Pts',(373.94544572082,-0.488624623883388,0.846742881849301));
#31986=CARTESIAN_POINT('Ctrl Pts',(373.916248665641,-0.494770446601752,
0.942242023035207));
#31987=CARTESIAN_POINT('Ctrl Pts',(373.887047109578,-0.500917216731959,
1.03775588593073));
#31988=CARTESIAN_POINT('Ctrl Pts',(373.853407097286,-0.507063986862167,
1.13189175712116));
#31989=CARTESIAN_POINT('Ctrl Pts',(373.815494063152,-0.513210756992375,
1.22421647099736));
#31990=CARTESIAN_POINT('Ctrl Pts',(373.77754060439,-0.519364081092622,1.31663962574508));
#31991=CARTESIAN_POINT('Ctrl Pts',(373.735305191492,-0.525517405192868,
1.40724736380236));
#31992=CARTESIAN_POINT('Ctrl Pts',(373.689001032213,-0.531670729293115,
1.49562746367374));
#31993=CARTESIAN_POINT('Ctrl Pts',(373.642671032123,-0.53782748735895,1.58405688554031));
#31994=CARTESIAN_POINT('Ctrl Pts',(373.592267983493,-0.543984245424785,
1.67025581806251));
#31995=CARTESIAN_POINT('Ctrl Pts',(373.538049521148,-0.550141003490619,
1.75383939697038));
#31996=CARTESIAN_POINT('Ctrl Pts',(373.48374068311,-0.556308024135873,1.83756229970866));
#31997=CARTESIAN_POINT('Ctrl Pts',(373.425603981768,-0.562475044781126,
1.91866078754878));
#31998=CARTESIAN_POINT('Ctrl Pts',(373.36393864059,-0.568642065426379,1.99678146892028));
#31999=CARTESIAN_POINT('Ctrl Pts',(373.317690646334,-0.573267229739699,
2.05537069837093));
#32000=CARTESIAN_POINT('Ctrl Pts',(373.269458741801,-0.577892394053019,
2.11228565003346));
#32001=CARTESIAN_POINT('Ctrl Pts',(373.219382449764,-0.582517558366338,
2.16739115824313));
#32002=CARTESIAN_POINT('Ctrl Pts',(373.152552371861,-0.588690141814474,
2.24093305315411));
#32003=CARTESIAN_POINT('Ctrl Pts',(373.082200751653,-0.59486272526261,2.31150974165541));
#32004=CARTESIAN_POINT('Ctrl Pts',(373.008621053345,-0.601035308710746,
2.37876504860047));
#32005=CARTESIAN_POINT('Ctrl Pts',(372.935128263089,-0.607200601463062,
2.44594091749672));
#32006=CARTESIAN_POINT('Ctrl Pts',(372.858415284192,-0.613365894215377,
2.50980290584623));
#32007=CARTESIAN_POINT('Ctrl Pts',(372.778814595073,-0.619531186967692,
2.5700291794918));
#32008=CARTESIAN_POINT('Ctrl Pts',(372.699299951336,-0.625689815268,2.63019035077703));
#32009=CARTESIAN_POINT('Ctrl Pts',(372.616904148337,-0.631848443568307,
2.68672336157344));
#32010=CARTESIAN_POINT('Ctrl Pts',(372.531994231394,-0.638007071868615,
2.73934526438414));
#32011=CARTESIAN_POINT('Ctrl Pts',(372.459677807224,-0.643252277523014,
2.78416250106559));
#32012=CARTESIAN_POINT('Ctrl Pts',(372.385538442582,-0.648497483177413,
2.82614329651706));
#32013=CARTESIAN_POINT('Ctrl Pts',(372.309820613641,-0.653742688831811,
2.86513684952399));
#32014=CARTESIAN_POINT('',(372.705904384963,0.,-2.62360084935056));
#32015=CARTESIAN_POINT('Origin',(370.834317853224,0.,0.));
#32016=CARTESIAN_POINT('Ctrl Pts',(372.705904384963,-1.88737914186277E-14,
-2.62360084935056));
#32017=CARTESIAN_POINT('Ctrl Pts',(372.710595199592,-0.000355697368928507,
-2.62025458366962));
#32018=CARTESIAN_POINT('Ctrl Pts',(372.71527706713,-0.000710695953714261,
-2.61689571828344));
#32019=CARTESIAN_POINT('Ctrl Pts',(372.726024488927,-0.00152561838845565,
-2.60914155910339));
#32020=CARTESIAN_POINT('Ctrl Pts',(372.732083798716,-0.0019850712772657,
-2.60473762387074));
#32021=CARTESIAN_POINT('Ctrl Pts',(372.75152913268,-0.00345972216930044,
-2.59050078946874));
#32022=CARTESIAN_POINT('Ctrl Pts',(372.76485471502,-0.00447056845869583,
-2.58058537480191));
#32023=CARTESIAN_POINT('Ctrl Pts',(372.827584205144,-0.00923319459196886,
-2.53315122480681));
#32024=CARTESIAN_POINT('Ctrl Pts',(372.875977245289,-0.012919598606441,
-2.49431226153856));
#32025=CARTESIAN_POINT('Ctrl Pts',(373.062491552304,-0.0272949789361674,
-2.33555318111472));
#32026=CARTESIAN_POINT('Ctrl Pts',(373.191424246573,-0.0376225082491726,
-2.20536226950303));
#32027=CARTESIAN_POINT('Ctrl Pts',(373.411297193783,-0.0573074579025147,
-1.94189968905256));
#32028=CARTESIAN_POINT('Ctrl Pts',(373.504644928321,-0.0665995606112878,
-1.81139252326241));
#32029=CARTESIAN_POINT('Ctrl Pts',(373.603766592501,-0.0780645279400828,
-1.64839445970101));
#32030=CARTESIAN_POINT('Ctrl Pts',(373.619265551378,-0.0799114376741435,
-1.62207177619305));
#32031=CARTESIAN_POINT('Ctrl Pts',(373.643124308413,-0.0828444227877941,
-1.58020102176749));
#32032=CARTESIAN_POINT('Ctrl Pts',(373.651734757191,-0.0839224024414881,
-1.56479741299886));
#32033=CARTESIAN_POINT('Ctrl Pts',(373.667657033818,-0.0859533507183905,
-1.53575586718835));
#32034=CARTESIAN_POINT('Ctrl Pts',(373.674998010408,-0.086905342091268,
-1.52213443177768));
#32035=CARTESIAN_POINT('Ctrl Pts',(373.691269653501,-0.0890513730776003,
-1.49141412385848));
#32036=CARTESIAN_POINT('Ctrl Pts',(373.700145406773,-0.0902471465684238,
-1.4742869759262));
#32037=CARTESIAN_POINT('Ctrl Pts',(373.722442405138,-0.0933171758043124,
-1.43029917307434));
#32038=CARTESIAN_POINT('Ctrl Pts',(373.735642766526,-0.0951984719800697,
-1.40332918718747));
#32039=CARTESIAN_POINT('Ctrl Pts',(373.829711214165,-0.109091545327147,
-1.20413334536655));
#32040=CARTESIAN_POINT('Ctrl Pts',(373.895549522849,-0.12158877127422,-1.02525981580862));
#32041=CARTESIAN_POINT('Ctrl Pts',(373.985444694561,-0.144778976218852,
-0.69299004925008));
#32042=CARTESIAN_POINT('Ctrl Pts',(374.01495630327,-0.155325176176758,-0.5416384720622));
#32043=CARTESIAN_POINT('Ctrl Pts',(374.05066609345,-0.175389091965657,-0.247775798164879));
#32044=CARTESIAN_POINT('Ctrl Pts',(374.05846218053,-0.184898559658955,-0.105791209733848));
#32045=CARTESIAN_POINT('Ctrl Pts',(374.05664542742,-0.195218383926661,0.0556734029323275));
#32046=CARTESIAN_POINT('Ctrl Pts',(374.056251540141,-0.196450884388894,
0.0750858414775472));
#32047=CARTESIAN_POINT('Ctrl Pts',(374.055441860438,-0.198190641023431,
0.102688345798392));
#32048=CARTESIAN_POINT('Ctrl Pts',(374.055170225417,-0.198705467217268,
0.110881766805682));
#32049=CARTESIAN_POINT('Ctrl Pts',(374.054566926671,-0.199727451126924,
0.127198937059484));
#32050=CARTESIAN_POINT('Ctrl Pts',(374.054235779015,-0.20023463366276,0.135322648850631));
#32051=CARTESIAN_POINT('Ctrl Pts',(374.053549122606,-0.201193633047422,
0.150734317590427));
#32052=CARTESIAN_POINT('Ctrl Pts',(374.053199611312,-0.201645760512203,
0.158022241656684));
#32053=CARTESIAN_POINT('Ctrl Pts',(374.05230454207,-0.202723686048867,0.175448907387578));
#32054=CARTESIAN_POINT('Ctrl Pts',(374.051735819817,-0.203348166766796,
0.185586323722907));
#32055=CARTESIAN_POINT('Ctrl Pts',(374.049510339479,-0.20559267071202,0.222163525356412));
#32056=CARTESIAN_POINT('Ctrl Pts',(374.047575449606,-0.207197625732224,
0.248586163341267));
#32057=CARTESIAN_POINT('Ctrl Pts',(374.031446666722,-0.218539957036256,
0.436923222005815));
#32058=CARTESIAN_POINT('Ctrl Pts',(374.005345694926,-0.22770899496835,0.597603616188866));
#32059=CARTESIAN_POINT('Ctrl Pts',(373.910432772169,-0.250374702730624,
0.991113254418384));
#32060=CARTESIAN_POINT('Ctrl Pts',(373.827281499534,-0.263771362180913,
1.21940384889745));
#32061=CARTESIAN_POINT('Ctrl Pts',(373.69846769339,-0.280852199434449,1.4781603786224));
#32062=CARTESIAN_POINT('Ctrl Pts',(373.676678156632,-0.283649918022502,
1.51963810582951));
#32063=CARTESIAN_POINT('Ctrl Pts',(373.644693300662,-0.287640511764521,
1.57742708762179));
#32064=CARTESIAN_POINT('Ctrl Pts',(373.63524367352,-0.288806176561682,1.59414582021381));
#32065=CARTESIAN_POINT('Ctrl Pts',(373.618749342303,-0.290818828170985,
1.62272893775445));
#32066=CARTESIAN_POINT('Ctrl Pts',(373.611776758296,-0.291663116633241,
1.63463449853355));
#32067=CARTESIAN_POINT('Ctrl Pts',(373.598312516365,-0.293281340335338,
1.65728957979945));
#32068=CARTESIAN_POINT('Ctrl Pts',(373.59183404412,-0.294054767673054,1.66804667164073));
#32069=CARTESIAN_POINT('Ctrl Pts',(373.576523354282,-0.295870719838971,
1.69313613547891));
#32070=CARTESIAN_POINT('Ctrl Pts',(373.567641436633,-0.296915124142863,
1.70743759879041));
#32071=CARTESIAN_POINT('Ctrl Pts',(373.536779252183,-0.300513917069573,
1.75627323429129));
#32072=CARTESIAN_POINT('Ctrl Pts',(373.514254047964,-0.30308918526027,1.79045665120519));
#32073=CARTESIAN_POINT('Ctrl Pts',(373.354961334725,-0.320966502662487,
2.02245066841634));
#32074=CARTESIAN_POINT('Ctrl Pts',(373.197101417432,-0.337137514679321,
2.20480414807088));
#32075=CARTESIAN_POINT('Ctrl Pts',(372.879884635299,-0.366556422975145,
2.49767640095164));
#32076=CARTESIAN_POINT('Ctrl Pts',(372.728002084667,-0.379643674779031,
2.61470919996204));
#32077=CARTESIAN_POINT('Ctrl Pts',(372.540420582599,-0.394010056326614,
2.73428169561147));
#32078=CARTESIAN_POINT('Ctrl Pts',(372.513979369807,-0.395996145490956,
2.75060362135331));
#32079=CARTESIAN_POINT('Ctrl Pts',(372.477537012697,-0.39867617672395,2.7723776499127));
#32080=CARTESIAN_POINT('Ctrl Pts',(372.467737949054,-0.399391241965818,
2.77816231347754));
#32081=CARTESIAN_POINT('Ctrl Pts',(372.451103454331,-0.400595424066035,
2.78786368713729));
#32082=CARTESIAN_POINT('Ctrl Pts',(372.444284136164,-0.401086327758437,
2.7918073334043));
#32083=CARTESIAN_POINT('Ctrl Pts',(372.431109945166,-0.402029509338662,
2.79936171238655));
#32084=CARTESIAN_POINT('Ctrl Pts',(372.424757122346,-0.402482019178931,
2.80297590346819));
#32085=CARTESIAN_POINT('Ctrl Pts',(372.409670996141,-0.403551272032026,
2.81149076505466));
#32086=CARTESIAN_POINT('Ctrl Pts',(372.400926977903,-0.404166806379806,
2.81637243694016));
#32087=CARTESIAN_POINT('Ctrl Pts',(372.370008016251,-0.406329039220401,
2.83344554068852));
#32088=CARTESIAN_POINT('Ctrl Pts',(372.347711732291,-0.407862439951093,
2.84541683521823));
#32089=CARTESIAN_POINT('Ctrl Pts',(372.32013108445,-0.409730584608208,2.85980948359887));
#32090=CARTESIAN_POINT('Ctrl Pts',(372.314979276673,-0.410078317270426,
2.86248021498102));
#32091=CARTESIAN_POINT('Ctrl Pts',(372.309820610785,-0.410425323647676,
2.86513685099491));
#32092=CARTESIAN_POINT('Origin',(370.834317853224,2.31077344927308,0.));
#32093=CARTESIAN_POINT('',(372.309820657227,-1.90534924053897,2.86513682707819));
#32094=CARTESIAN_POINT('',(372.309820561356,-1.65539601866286,2.86513687645008));
#32095=CARTESIAN_POINT('',(372.309820613641,2.31077344927308,2.86513684952399));
#32096=CARTESIAN_POINT('',(367.611568223216,-1.06077344924052,0.00154427509180863));
#32097=CARTESIAN_POINT('Ctrl Pts',(372.309820657226,-1.90534924053903,2.86513682707864));
#32098=CARTESIAN_POINT('Ctrl Pts',(372.358965257756,-1.90218876223823,2.83982808956957));
#32099=CARTESIAN_POINT('Ctrl Pts',(372.407491827767,-1.89899741261244,2.81323787201031));
#32100=CARTESIAN_POINT('Ctrl Pts',(372.515632405171,-1.89169475069727,2.75030248885923));
#32101=CARTESIAN_POINT('Ctrl Pts',(372.574756722089,-1.8875660225164,2.71327364968646));
#32102=CARTESIAN_POINT('Ctrl Pts',(372.652227002293,-1.88194537062448,2.66118048270359));
#32103=CARTESIAN_POINT('Ctrl Pts',(372.671677853702,-1.88051578015962,2.64778840148354));
#32104=CARTESIAN_POINT('Ctrl Pts',(372.703310052921,-1.87815965478522,2.62549296325104));
#32105=CARTESIAN_POINT('Ctrl Pts',(372.715579377309,-1.87723793698878,2.61671553831594));
#32106=CARTESIAN_POINT('Ctrl Pts',(372.73925693678,-1.87544368235301,2.59952410699681));
#32107=CARTESIAN_POINT('Ctrl Pts',(372.750672190822,-1.8745715542882,2.59112032477927));
#32108=CARTESIAN_POINT('Ctrl Pts',(372.777281329201,-1.87252170937226,2.57125895545952));
#32109=CARTESIAN_POINT('Ctrl Pts',(372.792429783173,-1.87134167378764,2.5597416529613));
#32110=CARTESIAN_POINT('Ctrl Pts',(372.841651751469,-1.86746377749195,2.52162579260534));
#32111=CARTESIAN_POINT('Ctrl Pts',(372.875291082146,-1.86474422852624,2.4944766995266));
#32112=CARTESIAN_POINT('Ctrl Pts',(372.953780901324,-1.85822886286021,2.42847968696302));
#32113=CARTESIAN_POINT('Ctrl Pts',(372.998123423556,-1.85441068318616,2.38905461252519));
#32114=CARTESIAN_POINT('Ctrl Pts',(373.165708792951,-1.8394365540771,2.23155945434327));
#32115=CARTESIAN_POINT('Ctrl Pts',(373.280575124685,-1.8279627481987,2.10500719673513));
#32116=CARTESIAN_POINT('Ctrl Pts',(373.499302648768,-1.80375852356601,1.82181716839251));
#32117=CARTESIAN_POINT('Ctrl Pts',(373.60061673185,-1.79105943269172,1.66396051308825));
#32118=CARTESIAN_POINT('Ctrl Pts',(373.700070140212,-1.77731752191173,1.47454884321366));
#32119=CARTESIAN_POINT('Ctrl Pts',(373.712188700715,-1.77561705036003,1.45075495997621));
#32120=CARTESIAN_POINT('Ctrl Pts',(373.728566342094,-1.77328485259655,1.41758567057998));
#32121=CARTESIAN_POINT('Ctrl Pts',(373.733077950058,-1.77263864789564,1.40833708909115));
#32122=CARTESIAN_POINT('Ctrl Pts',(373.740755785561,-1.77153264112166,1.39240468282946));
#32123=CARTESIAN_POINT('Ctrl Pts',(373.743943413507,-1.77107154576633,1.38573134367777));
#32124=CARTESIAN_POINT('Ctrl Pts',(373.75057477007,-1.77010836781202,1.37172475041674));
#32125=CARTESIAN_POINT('Ctrl Pts',(373.754013858178,-1.76960658994784,1.36438940059388));
#32126=CARTESIAN_POINT('Ctrl Pts',(373.762385343081,-1.76837937225814,1.34635696984024));
#32127=CARTESIAN_POINT('Ctrl Pts',(373.76728688401,-1.76765580787219,1.33564553300868));
#32128=CARTESIAN_POINT('Ctrl Pts',(373.784966337714,-1.765026553573,1.29644361357424));
#32129=CARTESIAN_POINT('Ctrl Pts',(373.797389204426,-1.76314122303744,1.26779369560465));
#32130=CARTESIAN_POINT('Ctrl Pts',(373.827613233149,-1.75844490671052,1.19521805327377));
#32131=CARTESIAN_POINT('Ctrl Pts',(373.844865962017,-1.75566049989041,1.15107078773375));
#32132=CARTESIAN_POINT('Ctrl Pts',(373.919104361675,-1.74311127397163,0.948002704885711));
#32133=CARTESIAN_POINT('Ctrl Pts',(373.964525400627,-1.73374774983065,0.785127834286161));
#32134=CARTESIAN_POINT('Ctrl Pts',(374.03845215783,-1.71222540834526,0.40767840447732));
#32135=CARTESIAN_POINT('Ctrl Pts',(374.058550192514,-1.70004132606598,0.19232187737371));
#32136=CARTESIAN_POINT('Ctrl Pts',(374.056783881818,-1.68548996994238,-0.0507928044017276));
#32137=CARTESIAN_POINT('Ctrl Pts',(374.056236067526,-1.68384093558131,-0.0781675460567816));
#32138=CARTESIAN_POINT('Ctrl Pts',(374.054766266122,-1.68111974524524,-0.123028731629179));
#32139=CARTESIAN_POINT('Ctrl Pts',(374.054050438088,-1.68005402405042,-0.140520860025591));
#32140=CARTESIAN_POINT('Ctrl Pts',(374.052506903585,-1.67812945151793,-0.171965506213771));
#32141=CARTESIAN_POINT('Ctrl Pts',(374.05173087715,-1.67727223902454,-0.185920205821364));
#32142=CARTESIAN_POINT('Ctrl Pts',(374.049881552839,-1.67543720060339,-0.215681849278053));
#32143=CARTESIAN_POINT('Ctrl Pts',(374.048782416845,-1.67445858620111,-0.231486762674127));
#32144=CARTESIAN_POINT('Ctrl Pts',(374.045488428003,-1.67179684407882,-0.274289619046491));
#32145=CARTESIAN_POINT('Ctrl Pts',(374.043069703146,-1.67010675053642,-0.301268566399799));
#32146=CARTESIAN_POINT('Ctrl Pts',(374.028163648219,-1.66091631187879,-0.44687123367169));
#32147=CARTESIAN_POINT('Ctrl Pts',(374.0094394124,-1.65322214139594,-0.564749648869219));
#32148=CARTESIAN_POINT('Ctrl Pts',(373.951070804538,-1.63502777695632,-0.834606757803964));
#32149=CARTESIAN_POINT('Ctrl Pts',(373.906768675642,-1.62442537289036,-0.985269727399512));
#32150=CARTESIAN_POINT('Ctrl Pts',(373.793126586864,-1.60254174440567,-1.28815845535703));
#32151=CARTESIAN_POINT('Ctrl Pts',(373.722548042371,-1.59129287642241,-1.43945761873371));
#32152=CARTESIAN_POINT('Ctrl Pts',(373.627319453799,-1.57884968316682,-1.60810019270213));
#32153=CARTESIAN_POINT('Ctrl Pts',(373.61377085924,-1.5771326574901,-1.63140591768199));
#32154=CARTESIAN_POINT('Ctrl Pts',(373.594629847911,-1.57478193949283,-1.6634006949898));
#32155=CARTESIAN_POINT('Ctrl Pts',(373.589286119799,-1.57413346665485,-1.67223623841909));
#32156=CARTESIAN_POINT('Ctrl Pts',(373.580037614334,-1.57302462191573,-1.68736344112174));
#32157=CARTESIAN_POINT('Ctrl Pts',(373.576153488163,-1.57256294195627,-1.6936675419275));
#32158=CARTESIAN_POINT('Ctrl Pts',(373.567978616084,-1.57159967929717,-1.70683388016171));
#32159=CARTESIAN_POINT('Ctrl Pts',(373.563683701244,-1.57109839472004,-1.71369341782959));
#32160=CARTESIAN_POINT('Ctrl Pts',(373.553097750191,-1.56987434334923,-1.73045981002238));
#32161=CARTESIAN_POINT('Ctrl Pts',(373.54677827581,-1.56915342915781,-1.74034874322648));
#32162=CARTESIAN_POINT('Ctrl Pts',(373.523610959304,-1.56654503809942,-1.77616902751122));
#32163=CARTESIAN_POINT('Ctrl Pts',(373.506443540912,-1.56467749801854,-1.80189297521584));
#32164=CARTESIAN_POINT('Ctrl Pts',(373.462387008036,-1.56003478393184,-1.86589327534014));
#32165=CARTESIAN_POINT('Ctrl Pts',(373.435029314207,-1.55728541658533,-1.90383967978715));
#32166=CARTESIAN_POINT('Ctrl Pts',(373.205518843448,-1.53515782295162,-2.20799710509426));
#32167=CARTESIAN_POINT('Ctrl Pts',(372.963898410823,-1.51734685381353,-2.44187864696232));
#32168=CARTESIAN_POINT('Ctrl Pts',(372.637020800093,-1.4939564598771,-2.6722046107394));
#32169=CARTESIAN_POINT('Ctrl Pts',(372.582293691837,-1.49006965325307,-2.70831958677603));
#32170=CARTESIAN_POINT('Ctrl Pts',(372.506876953788,-1.48473153999039,-2.75484946657579));
#32171=CARTESIAN_POINT('Ctrl Pts',(372.487118845157,-1.48333470806577,-2.76674869966166));
#32172=CARTESIAN_POINT('Ctrl Pts',(372.45433152374,-1.48101868061711,-2.7860181770424));
#32173=CARTESIAN_POINT('Ctrl Pts',(372.441375447892,-1.48010398125763,-2.79351167010738));
#32174=CARTESIAN_POINT('Ctrl Pts',(372.415999542451,-1.4783131680652,-2.80795354629218));
#32175=CARTESIAN_POINT('Ctrl Pts',(372.403584943946,-1.47743738793837,-2.81491045538196));
#32176=CARTESIAN_POINT('Ctrl Pts',(372.374168278894,-1.47536279228488,-2.83113992442026));
#32177=CARTESIAN_POINT('Ctrl Pts',(372.357128051344,-1.47416149396798,-2.84034182438249));
#32178=CARTESIAN_POINT('Ctrl Pts',(372.30005604942,-1.4701389562297,-2.87050009210162));
#32179=CARTESIAN_POINT('Ctrl Pts',(372.259668057428,-1.46729372929559,-2.89076732053195));
#32180=CARTESIAN_POINT('Ctrl Pts',(372.162091899843,-1.46041986621677,-2.93719031379544));
#32181=CARTESIAN_POINT('Ctrl Pts',(372.104539817312,-1.45636543767094,-2.96253374272594));
#32182=CARTESIAN_POINT('Ctrl Pts',(371.725868913342,-1.42969287408322,-3.11622097019959));
#32183=CARTESIAN_POINT('Ctrl Pts',(371.386677444198,-1.40549755302805,-3.19382820326595));
#32184=CARTESIAN_POINT('Ctrl Pts',(371.01045283922,-1.38118634815374,-3.21808527618487));
#32185=CARTESIAN_POINT('Ctrl Pts',(370.979202609063,-1.37918811537089,-3.21964360675774));
#32186=CARTESIAN_POINT('Ctrl Pts',(370.935788779535,-1.37644590879556,-3.22117507864337));
#32187=CARTESIAN_POINT('Ctrl Pts',(370.92364167345,-1.37568231635751,-3.22153480539511));
#32188=CARTESIAN_POINT('Ctrl Pts',(370.904129631126,-1.37446195725025,-3.22200219158046));
#32189=CARTESIAN_POINT('Ctrl Pts',(370.896765993851,-1.37400282640067,-3.22215332335272));
#32190=CARTESIAN_POINT('Ctrl Pts',(370.88126768742,-1.37303956967436,-3.22241826257151));
#32191=CARTESIAN_POINT('Ctrl Pts',(370.873132998323,-1.37253577189034,-3.22252651387325));
#32192=CARTESIAN_POINT('Ctrl Pts',(370.853059393832,-1.3712968084757,-3.22271762000995));
#32193=CARTESIAN_POINT('Ctrl Pts',(370.84112011722,-1.37056359971414,-3.22276493763734));
#32194=CARTESIAN_POINT('Ctrl Pts',(370.796873188968,-1.36785911869301,-3.22269440584148));
#32195=CARTESIAN_POINT('Ctrl Pts',(370.764566931014,-1.365909745716,-3.2221570921666));
#32196=CARTESIAN_POINT('Ctrl Pts',(370.529252415316,-1.35185965882292,-3.21470236545968));
#32197=CARTESIAN_POINT('Ctrl Pts',(370.327268455537,-1.34058774133008,-3.18909042619886));
#32198=CARTESIAN_POINT('Ctrl Pts',(369.924969777267,-1.31752960102629,-3.09886025870466));
#32199=CARTESIAN_POINT('Ctrl Pts',(369.725882105887,-1.30577769202467,-3.03334894370896));
#32200=CARTESIAN_POINT('Ctrl Pts',(369.496180742314,-1.29087772346656,-2.93210931995807));
#32201=CARTESIAN_POINT('Ctrl Pts',(369.458143958016,-1.28836537950399,-2.91445040410724));
#32202=CARTESIAN_POINT('Ctrl Pts',(369.403749017095,-1.28470194649725,-2.88789479386997));
#32203=CARTESIAN_POINT('Ctrl Pts',(369.387105454044,-1.28357131706961,-2.87959021122137));
#32204=CARTESIAN_POINT('Ctrl Pts',(369.357919342442,-1.28157104828055,-2.86471037312364));
#32205=CARTESIAN_POINT('Ctrl Pts',(369.345346397863,-1.28070354551683,-2.85819559854589));
#32206=CARTESIAN_POINT('Ctrl Pts',(369.331306664723,-1.27972819331574,-2.85080301724165));
#32207=CARTESIAN_POINT('Ctrl Pts',(369.329797010761,-1.27962322992909,-2.85000658077336));
#32208=CARTESIAN_POINT('Ctrl Pts',(369.31480065958,-1.27857970106569,-2.84207983580576));
#32209=CARTESIAN_POINT('Ctrl Pts',(369.301364306594,-1.27763780078315,-2.83485514726422));
#32210=CARTESIAN_POINT('Ctrl Pts',(369.265903631211,-1.27513329932544,-2.81546222073194));
#32211=CARTESIAN_POINT('Ctrl Pts',(369.243969998042,-1.27356492069393,-2.80313116532678));
#32212=CARTESIAN_POINT('Ctrl Pts',(369.196052555179,-1.27009517308511,-2.77544862976222));
#32213=CARTESIAN_POINT('Ctrl Pts',(369.170135689269,-1.26818993601732,-2.75998657778828));
#32214=CARTESIAN_POINT('Ctrl Pts',(369.092861902724,-1.2624216152785,-2.71240077032987));
#32215=CARTESIAN_POINT('Ctrl Pts',(369.042191964607,-1.25852047852587,-2.67919219309292));
#32216=CARTESIAN_POINT('Ctrl Pts',(368.847093909386,-1.24302706700509,-2.5433152903863));
#32217=CARTESIAN_POINT('Ctrl Pts',(368.710310307723,-1.23109204158757,-2.43024510669237));
#32218=CARTESIAN_POINT('Ctrl Pts',(368.456022489768,-1.20705494585068,-2.18210134263997));
#32219=CARTESIAN_POINT('Ctrl Pts',(368.339044748889,-1.1949967853666,-2.04731014431474));
#32220=CARTESIAN_POINT('Ctrl Pts',(368.217903934934,-1.18182015036386,-1.88181298039032));
#32221=CARTESIAN_POINT('Ctrl Pts',(368.202279574723,-1.18010588067814,-1.85989690448217));
#32222=CARTESIAN_POINT('Ctrl Pts',(368.181046223146,-1.17775825134408,-1.82930962764315));
#32223=CARTESIAN_POINT('Ctrl Pts',(368.175202081164,-1.17711016236529,-1.82080404611527));
#32224=CARTESIAN_POINT('Ctrl Pts',(368.165235673742,-1.17600177976766,-1.80614857917896));
#32225=CARTESIAN_POINT('Ctrl Pts',(368.161093601243,-1.17554018077972,-1.80001235332713));
#32226=CARTESIAN_POINT('Ctrl Pts',(368.152469681694,-1.17457720921772,-1.78714112262405));
#32227=CARTESIAN_POINT('Ctrl Pts',(368.147992001893,-1.17407613488385,-1.78040344569922));
#32228=CARTESIAN_POINT('Ctrl Pts',(368.137081197483,-1.17285231355942,-1.76385081588648));
#32229=CARTESIAN_POINT('Ctrl Pts',(368.130676140902,-1.17213142139114,-1.75401732575872));
#32230=CARTESIAN_POINT('Ctrl Pts',(368.107572899926,-1.16952126094381,-1.71812037784747));
#32231=CARTESIAN_POINT('Ctrl Pts',(368.09119612829,-1.16765198804557,-1.69185077241047));
#32232=CARTESIAN_POINT('Ctrl Pts',(368.050994991025,-1.16300365873376,-1.62524627084856));
#32233=CARTESIAN_POINT('Ctrl Pts',(368.027666211943,-1.16025051846008,-1.58461938485034));
#32234=CARTESIAN_POINT('Ctrl Pts',(367.85676982659,-1.13953111491668,-1.27138196596628));
#32235=CARTESIAN_POINT('Ctrl Pts',(367.748336729678,-1.12293168273889,-0.979263670863363));
#32236=CARTESIAN_POINT('Ctrl Pts',(367.665437499162,-1.10004431707633,-0.592922851485402));
#32237=CARTESIAN_POINT('Ctrl Pts',(367.650887003311,-1.09503446001441,-0.509044594904192));
#32238=CARTESIAN_POINT('Ctrl Pts',(367.636330877633,-1.0883951868073,-0.399550051300437));
#32239=CARTESIAN_POINT('Ctrl Pts',(367.633285330436,-1.08686161933463,-0.374368363422848));
#32240=CARTESIAN_POINT('Ctrl Pts',(367.628862282565,-1.08437818070093,-0.333783180586575));
#32241=CARTESIAN_POINT('Ctrl Pts',(367.627297815471,-1.08343420562926,-0.318400834648632));
#32242=CARTESIAN_POINT('Ctrl Pts',(367.624568524469,-1.08165535909282,-0.289501077812639));
#32243=CARTESIAN_POINT('Ctrl Pts',(367.623378248903,-1.08082130833095,-0.275986369158513));
#32244=CARTESIAN_POINT('Ctrl Pts',(367.621167326447,-1.07914695566432,-0.24892908854256));
#32245=CARTESIAN_POINT('Ctrl Pts',(367.620146878716,-1.07830666541041,-0.235386780507604));
#32246=CARTESIAN_POINT('Ctrl Pts',(367.618012431225,-1.07638187314418,-0.20445224183574));
#32247=CARTESIAN_POINT('Ctrl Pts',(367.616953862686,-1.07529565752283,-0.187056729299228));
#32248=CARTESIAN_POINT('Ctrl Pts',(367.613027725727,-1.07062818693322,-0.112579076832374));
#32249=CARTESIAN_POINT('Ctrl Pts',(367.611538005706,-1.06700444690195,-0.0554381735805181));
#32250=CARTESIAN_POINT('Ctrl Pts',(367.611568306237,-1.06333585784792,0.00170877070520201));
#32251=CARTESIAN_POINT('Ctrl Pts',(372.309820613641,-0.653742688831811,
2.86513684952399));
#32252=CARTESIAN_POINT('Ctrl Pts',(372.221003209592,-0.659895342129579,
2.91087648840709));
#32253=CARTESIAN_POINT('Ctrl Pts',(372.130013640704,-0.666047995427347,
2.95250465231268));
#32254=CARTESIAN_POINT('Ctrl Pts',(372.037270397767,-0.672200648725115,
2.98981985043874));
#32255=CARTESIAN_POINT('Ctrl Pts',(371.944541014133,-0.678352382586736,
3.02712947228082));
#32256=CARTESIAN_POINT('Ctrl Pts',(371.850058880057,-0.684504116448356,
3.06012724754406));
#32257=CARTESIAN_POINT('Ctrl Pts',(371.754262553616,-0.690655850309977,
3.08865979200057));
#32258=CARTESIAN_POINT('Ctrl Pts',(371.658454961579,-0.696808307612121,
3.11719569186864));
#32259=CARTESIAN_POINT('Ctrl Pts',(371.561333286326,-0.702960764914265,
3.14126519418015));
#32260=CARTESIAN_POINT('Ctrl Pts',(371.463350361894,-0.709113222216409,
3.16076504434233));
#32261=CARTESIAN_POINT('Ctrl Pts',(371.365265340964,-0.715272090271694,
3.18028521300809));
#32262=CARTESIAN_POINT('Ctrl Pts',(371.266317705121,-0.721430958326981,
3.1952261345892));
#32263=CARTESIAN_POINT('Ctrl Pts',(371.166969482799,-0.727589826382267,
3.20553590774477));
#32264=CARTESIAN_POINT('Ctrl Pts',(371.067569304964,-0.733751915301877,
3.2158510725373));
#32265=CARTESIAN_POINT('Ctrl Pts',(370.967768556964,-0.739914004221487,
3.22153024006408));
#32266=CARTESIAN_POINT('Ctrl Pts',(370.868031268253,-0.746076093141097,
3.22257365596924));
#32267=CARTESIAN_POINT('Ctrl Pts',(370.768124212498,-0.752248670812111,
3.22361884791661));
#32268=CARTESIAN_POINT('Ctrl Pts',(370.668281266254,-0.758421248483125,
3.22001253849878));
#32269=CARTESIAN_POINT('Ctrl Pts',(370.568963573348,-0.764593826154139,
3.21180707214045));
#32270=CARTESIAN_POINT('Ctrl Pts',(370.480790364716,-0.770073776028762,
3.20452234495869));
#32271=CARTESIAN_POINT('Ctrl Pts',(370.393031264093,-0.775553725903385,
3.19361348331574));
#32272=CARTESIAN_POINT('Ctrl Pts',(370.306001381893,-0.781033675778008,
3.17915071498974));
#32273=CARTESIAN_POINT('Ctrl Pts',(370.207941047915,-0.787208172414114,
3.16285488812622));
#32274=CARTESIAN_POINT('Ctrl Pts',(370.110464290368,-0.79338266905022,3.14198940079307));
#32275=CARTESIAN_POINT('Ctrl Pts',(370.01402988079,-0.799557165686327,3.11660796456343));
#32276=CARTESIAN_POINT('Ctrl Pts',(369.917725341106,-0.805723347020595,
3.09126070995472));
#32277=CARTESIAN_POINT('Ctrl Pts',(369.822460775281,-0.811889528354863,
3.061409704322));
#32278=CARTESIAN_POINT('Ctrl Pts',(369.728686991684,-0.818055709689131,
3.02716004871069));
#32279=CARTESIAN_POINT('Ctrl Pts',(369.635011848886,-0.824215404806936,
2.99294642036943));
#32280=CARTESIAN_POINT('Ctrl Pts',(369.542824776041,-0.830375099924741,
2.95434348917374));
#32281=CARTESIAN_POINT('Ctrl Pts',(369.452562653568,-0.836534795042546,
2.91150650535462));
#32282=CARTESIAN_POINT('Ctrl Pts',(369.362365759281,-0.842690038838683,
2.86870047780698));
#32283=CARTESIAN_POINT('Ctrl Pts',(369.274091440567,-0.848845282634821,
2.82166666654779));
#32284=CARTESIAN_POINT('Ctrl Pts',(369.188156918282,-0.855000526430958,
2.77060855025967));
#32285=CARTESIAN_POINT('Ctrl Pts',(369.102254519747,-0.861153469294887,
2.71956952034214));
#32286=CARTESIAN_POINT('Ctrl Pts',(369.01869055236,-0.867306412158817,2.66450939606797));
#32287=CARTESIAN_POINT('Ctrl Pts',(368.937857132645,-0.873459355022746,
2.60567732035315));
#32288=CARTESIAN_POINT('Ctrl Pts',(368.857032353384,-0.879611640185721,
2.54685153332216));
#32289=CARTESIAN_POINT('Ctrl Pts',(368.778937892372,-0.885763925348696,
2.48425485189353));
#32290=CARTESIAN_POINT('Ctrl Pts',(368.703935562196,-0.89191621051167,2.41817883056076));
#32291=CARTESIAN_POINT('Ctrl Pts',(368.628921229419,-0.898069480222924,
2.35209223510286));
#32292=CARTESIAN_POINT('Ctrl Pts',(368.557000336048,-0.904222749934177,
2.28252548067812));
#32293=CARTESIAN_POINT('Ctrl Pts',(368.488499621638,-0.91037601964543,2.20980867652812));
#32294=CARTESIAN_POINT('Ctrl Pts',(368.419925749182,-0.916535860984318,
2.13701421159253));
#32295=CARTESIAN_POINT('Ctrl Pts',(368.35477964779,-0.922695702323206,2.06106329557526));
#32296=CARTESIAN_POINT('Ctrl Pts',(368.293349255475,-0.928855543662094,
1.98232089928827));
#32297=CARTESIAN_POINT('Ctrl Pts',(368.231884417966,-0.935018838941698,
1.9035343506354));
#32298=CARTESIAN_POINT('Ctrl Pts',(368.174139689516,-0.941182134221302,
1.82195355876123));
#32299=CARTESIAN_POINT('Ctrl Pts',(368.120359756326,-0.947345429500906,
1.73797267262242));
#32300=CARTESIAN_POINT('Ctrl Pts',(368.066490578289,-0.95351895243069,1.65385242481322));
#32301=CARTESIAN_POINT('Ctrl Pts',(368.016599554071,-0.959692475360474,
1.56732450350204));
#32302=CARTESIAN_POINT('Ctrl Pts',(367.97088554308,-0.965865998290258,1.47880795498442));
#32303=CARTESIAN_POINT('Ctrl Pts',(367.937110060398,-0.970427263256725,
1.41340811176715));
#32304=CARTESIAN_POINT('Ctrl Pts',(367.90561379285,-0.974988528223193,1.34692320550947));
#32305=CARTESIAN_POINT('Ctrl Pts',(367.876459700432,-0.979549793189661,
1.27952831561645));
#32306=CARTESIAN_POINT('Ctrl Pts',(367.832910215336,-0.986363270276431,
1.1788559053471));
#32307=CARTESIAN_POINT('Ctrl Pts',(367.794457932752,-0.993176747363203,
1.075851191093));
#32308=CARTESIAN_POINT('Ctrl Pts',(367.761333116471,-0.999990224449973,
0.971021302640703));
#32309=CARTESIAN_POINT('Ctrl Pts',(367.728298687738,-1.00678510963019,0.866477463068555));
#32310=CARTESIAN_POINT('Ctrl Pts',(367.700562839212,-1.0135799948104,0.760118637330591));
#32311=CARTESIAN_POINT('Ctrl Pts',(367.678307875351,-1.02037487999061,0.652471135045156));
#32312=CARTESIAN_POINT('Ctrl Pts',(367.656161673856,-1.02713655784738,0.545349717503075));
#32313=CARTESIAN_POINT('Ctrl Pts',(367.63944303279,-1.03389823570415,0.436952446312823));
#32314=CARTESIAN_POINT('Ctrl Pts',(367.628283955551,-1.04065991356092,0.327817341629671));
#32315=CARTESIAN_POINT('Ctrl Pts',(367.617219221671,-1.04736442545412,0.219604909329125));
#32316=CARTESIAN_POINT('Ctrl Pts',(367.611620512735,-1.05406893734732,0.110667337950061));
#32317=CARTESIAN_POINT('Ctrl Pts',(367.611568223216,-1.06077344924052,0.00154427509180863));
#32318=CARTESIAN_POINT('Ctrl Pts',(372.309820610785,-0.410425323647672,
2.8651368509949));
#32319=CARTESIAN_POINT('Ctrl Pts',(372.119941942035,-0.423197833128021,
2.96292153421038));
#32320=CARTESIAN_POINT('Ctrl Pts',(371.920773159846,-0.435011031166651,
3.04160902462825));
#32321=CARTESIAN_POINT('Ctrl Pts',(371.570561117915,-0.455365295974534,
3.14112833017532));
#32322=CARTESIAN_POINT('Ctrl Pts',(371.423184159097,-0.463809664698718,
3.1720613536417));
#32323=CARTESIAN_POINT('Ctrl Pts',(371.191514904662,-0.477376157096664,
3.20398089562839));
#32324=CARTESIAN_POINT('Ctrl Pts',(371.108429490155,-0.482296506753667,
3.21215572210327));
#32325=CARTESIAN_POINT('Ctrl Pts',(371.000727684972,-0.488787789489794,
3.2185435626826));
#32326=CARTESIAN_POINT('Ctrl Pts',(370.976314989707,-0.490266553742547,
3.21971297793058));
#32327=CARTESIAN_POINT('Ctrl Pts',(370.936541031078,-0.492688780240232,
3.22116499829405));
#32328=CARTESIAN_POINT('Ctrl Pts',(370.921186609121,-0.493627005716013,
3.22161563983959));
#32329=CARTESIAN_POINT('Ctrl Pts',(370.891570367116,-0.495442990862056,
3.22227297765019));
#32330=CARTESIAN_POINT('Ctrl Pts',(370.877309218522,-0.496320259239618,
3.22249479829687));
#32331=CARTESIAN_POINT('Ctrl Pts',(370.844475433725,-0.498346687500237,
3.22278750861148));
#32332=CARTESIAN_POINT('Ctrl Pts',(370.825902854575,-0.499497861333115,
3.22279252620998));
#32333=CARTESIAN_POINT('Ctrl Pts',(370.766128421406,-0.503219135805091,
3.22229197662308));
#32334=CARTESIAN_POINT('Ctrl Pts',(370.724937278915,-0.505808507460077,
3.2211567832072));
#32335=CARTESIAN_POINT('Ctrl Pts',(370.468481747744,-0.52209191067235,3.20916445461529));
#32336=CARTESIAN_POINT('Ctrl Pts',(370.25477024742,-0.536427876831839,3.17752557318474));
#32337=CARTESIAN_POINT('Ctrl Pts',(369.923110087315,-0.559479874767384,
3.0938393971939));
#32338=CARTESIAN_POINT('Ctrl Pts',(369.802298286567,-0.568042075491482,
3.0556634690514));
#32339=CARTESIAN_POINT('Ctrl Pts',(369.629762621947,-0.580288959037265,
2.98973923675583));
#32340=CARTESIAN_POINT('Ctrl Pts',(369.576050438681,-0.584103390337076,
2.96753397217963));
#32341=CARTESIAN_POINT('Ctrl Pts',(369.491020414367,-0.590114274140003,
2.92965740609047));
#32342=CARTESIAN_POINT('Ctrl Pts',(369.459307748561,-0.592349721047187,
2.91490788283269));
#32343=CARTESIAN_POINT('Ctrl Pts',(369.41664394902,-0.595342335153094,2.89421372887305));
#32344=CARTESIAN_POINT('Ctrl Pts',(369.405479202283,-0.596124083145451,
2.88871814621087));
#32345=CARTESIAN_POINT('Ctrl Pts',(369.386880512363,-0.597423668686237,
2.87942917074082));
#32346=CARTESIAN_POINT('Ctrl Pts',(369.379429077677,-0.597943614376077,
2.87567137543549));
#32347=CARTESIAN_POINT('Ctrl Pts',(369.365397835357,-0.59892119675938,2.86852685263014));
#32348=CARTESIAN_POINT('Ctrl Pts',(369.358815001273,-0.599379204967817,
2.86514635896507));
#32349=CARTESIAN_POINT('Ctrl Pts',(369.343273293133,-0.60045917451941,2.85709743198338));
#32350=CARTESIAN_POINT('Ctrl Pts',(369.334324520543,-0.601079937244375,
2.85240944189247));
#32351=CARTESIAN_POINT('Ctrl Pts',(369.303158171976,-0.603238654544233,
2.83589510794055));
#32352=CARTESIAN_POINT('Ctrl Pts',(369.281056580626,-0.604763724944505,
2.82385030400531));
#32353=CARTESIAN_POINT('Ctrl Pts',(369.067112382762,-0.619491899769307,
2.70398420051586));
#32354=CARTESIAN_POINT('Ctrl Pts',(368.886621975315,-0.631670572573035,
2.57702410252286));
#32355=CARTESIAN_POINT('Ctrl Pts',(368.608987265892,-0.652267510272439,
2.33577224823941));
#32356=CARTESIAN_POINT('Ctrl Pts',(368.504306348232,-0.660574542953731,
2.23136061940861));
#32357=CARTESIAN_POINT('Ctrl Pts',(368.353043775316,-0.673927048656769,
2.05819411744613));
#32358=CARTESIAN_POINT('Ctrl Pts',(368.301323802834,-0.678780044283537,
1.99419747079431));
#32359=CARTESIAN_POINT('Ctrl Pts',(368.237588639153,-0.685191352666548,
1.90884888262688));
#32360=CARTESIAN_POINT('Ctrl Pts',(368.223286535392,-0.686660402449313,
1.88923849110129));
#32361=CARTESIAN_POINT('Ctrl Pts',(368.200336382318,-0.689068949688434,
1.85701185986968));
#32362=CARTESIAN_POINT('Ctrl Pts',(368.191554075396,-0.690003293275639,
1.84449208152134));
#32363=CARTESIAN_POINT('Ctrl Pts',(368.174775592114,-0.691813283548834,
1.82020736861242));
#32364=CARTESIAN_POINT('Ctrl Pts',(368.166767534539,-0.692688452332769,
1.80845104727943));
#32365=CARTESIAN_POINT('Ctrl Pts',(368.148492857501,-0.6947120996351,1.78123720630651));
#32366=CARTESIAN_POINT('Ctrl Pts',(368.138281465697,-0.695862607645018,
1.76574337516611));
#32367=CARTESIAN_POINT('Ctrl Pts',(368.105781708605,-0.699589366727602,
1.71549202760883));
#32368=CARTESIAN_POINT('Ctrl Pts',(368.084028044846,-0.702185117118837,
1.68039522323594));
#32369=CARTESIAN_POINT('Ctrl Pts',(367.943308335868,-0.719680666495249,
1.44330643755999));
#32370=CARTESIAN_POINT('Ctrl Pts',(367.846032902996,-0.735360211759838,
1.22930300199498));
#32371=CARTESIAN_POINT('Ctrl Pts',(367.728805014992,-0.760744725480299,
0.872796246329542));
#32372=CARTESIAN_POINT('Ctrl Pts',(367.693606705689,-0.770294752523127,
0.736152643239047));
#32373=CARTESIAN_POINT('Ctrl Pts',(367.659483234862,-0.782407371020832,
0.555334170277514));
#32374=CARTESIAN_POINT('Ctrl Pts',(367.652347894886,-0.785214110940032,
0.512872727928576));
#32375=CARTESIAN_POINT('Ctrl Pts',(367.641817908646,-0.789856625837867,
0.44148478900828));
#32376=CARTESIAN_POINT('Ctrl Pts',(367.63796073734,-0.791712165475381,0.41263305780363));
#32377=CARTESIAN_POINT('Ctrl Pts',(367.633126431945,-0.794272213694339,
0.372321261456269));
#32378=CARTESIAN_POINT('Ctrl Pts',(367.631819058225,-0.794993702298846,
0.36090319314314));
#32379=CARTESIAN_POINT('Ctrl Pts',(367.629697688302,-0.79621607773968,0.34145611758651));
#32380=CARTESIAN_POINT('Ctrl Pts',(367.628852727968,-0.796718660978283,
0.333430677237211));
#32381=CARTESIAN_POINT('Ctrl Pts',(367.62718046623,-0.797746581146961,0.316953400114207));
#32382=CARTESIAN_POINT('Ctrl Pts',(367.62635640962,-0.798271731832122,0.308501308231758));
#32383=CARTESIAN_POINT('Ctrl Pts',(367.624292658803,-0.799637694145501,
0.286431138947255));
#32384=CARTESIAN_POINT('Ctrl Pts',(367.623106195881,-0.800475571423377,
0.272808088895184));
#32385=CARTESIAN_POINT('Ctrl Pts',(367.618602485536,-0.803888661164334,
0.216987991109551));
#32386=CARTESIAN_POINT('Ctrl Pts',(367.616029821979,-0.806425348435268,
0.17473308541276));
#32387=CARTESIAN_POINT('Ctrl Pts',(367.606522046713,-0.820106200983126,
-0.0564347744226482));
#32388=CARTESIAN_POINT('Ctrl Pts',(367.61538566553,-0.83060204501898,-0.245645128138436));
#32389=CARTESIAN_POINT('Ctrl Pts',(367.661530625372,-0.849801064754592,
-0.58597804823855));
#32390=CARTESIAN_POINT('Ctrl Pts',(367.693235866667,-0.858453855073586,
-0.737257342582714));
#32391=CARTESIAN_POINT('Ctrl Pts',(367.751034437331,-0.870645748509624,
-0.939474290909169));
#32392=CARTESIAN_POINT('Ctrl Pts',(367.767809934252,-0.87392467487949,-0.992863152935819));
#32393=CARTESIAN_POINT('Ctrl Pts',(367.799364608177,-0.879697793455532,
-1.08484155707613));
#32394=CARTESIAN_POINT('Ctrl Pts',(367.813512005492,-0.882171859061296,
-1.12363437100682));
#32395=CARTESIAN_POINT('Ctrl Pts',(367.835121643227,-0.885798706178858,
-1.17952832453304));
#32396=CARTESIAN_POINT('Ctrl Pts',(367.841993557893,-0.886931732010983,
-1.19685431999605));
#32397=CARTESIAN_POINT('Ctrl Pts',(367.854314131446,-0.888928686346713,
-1.22714840678991));
#32398=CARTESIAN_POINT('Ctrl Pts',(367.859698163615,-0.889790407713328,
-1.24014236535341));
#32399=CARTESIAN_POINT('Ctrl Pts',(367.871054035134,-0.89158576952455,-1.26704946128958));
#32400=CARTESIAN_POINT('Ctrl Pts',(367.877039196298,-0.892519848177695,
-1.28095656667419));
#32401=CARTESIAN_POINT('Ctrl Pts',(367.892790614149,-0.894947355066135,
-1.31685768786658));
#32402=CARTESIAN_POINT('Ctrl Pts',(367.90270548396,-0.896445856722675,-1.33878509626597));
#32403=CARTESIAN_POINT('Ctrl Pts',(367.944129667997,-0.902590502798605,
-1.42773034393341));
#32404=CARTESIAN_POINT('Ctrl Pts',(367.977696876742,-0.90730729189912,-1.49375929552786));
#32405=CARTESIAN_POINT('Ctrl Pts',(368.171128958557,-0.933182627119895,
-1.84384664228556));
#32406=CARTESIAN_POINT('Ctrl Pts',(368.371070091033,-0.955800833142827,
-2.10349441518247));
#32407=CARTESIAN_POINT('Ctrl Pts',(368.640083820829,-0.98037863781435,-2.36085023046784));
#32408=CARTESIAN_POINT('Ctrl Pts',(368.674353426343,-0.983415920881478,
-2.39224390781704));
#32409=CARTESIAN_POINT('Ctrl Pts',(368.732408097809,-0.98839191738177,-2.44316155237734));
#32410=CARTESIAN_POINT('Ctrl Pts',(368.755814516315,-0.990354357634577,
-2.4631051605759));
#32411=CARTESIAN_POINT('Ctrl Pts',(368.788495300124,-0.993030451811923,
-2.49015338328426));
#32412=CARTESIAN_POINT('Ctrl Pts',(368.79752735841,-0.993763452333319,-2.49754645226084));
#32413=CARTESIAN_POINT('Ctrl Pts',(368.812860696712,-0.994996441671589,
-2.50995884783853));
#32414=CARTESIAN_POINT('Ctrl Pts',(368.819140939223,-0.995498250506953,
-2.51500386966016));
#32415=CARTESIAN_POINT('Ctrl Pts',(368.831233118488,-0.996458233722737,
-2.52464333937975));
#32416=CARTESIAN_POINT('Ctrl Pts',(368.837042014871,-0.996916677943237,
-2.52924132374726));
#32417=CARTESIAN_POINT('Ctrl Pts',(368.850986381156,-0.998010835266112,
-2.54020087530193));
#32418=CARTESIAN_POINT('Ctrl Pts',(368.85913673459,-0.998645222558279,-2.54654349468297));
#32419=CARTESIAN_POINT('Ctrl Pts',(368.888686087854,-1.00092729670446,-2.56931163867871));
#32420=CARTESIAN_POINT('Ctrl Pts',(368.910261291199,-1.00255981880434,-2.58550801917814));
#32421=CARTESIAN_POINT('Ctrl Pts',(369.066673026292,-1.01417532589859,-2.69988304614371));
#32422=CARTESIAN_POINT('Ctrl Pts',(369.20876498788,-1.0235770775129,-2.78774606063935));
#32423=CARTESIAN_POINT('Ctrl Pts',(369.584053879852,-1.04722621468534,-2.98130917596579));
#32424=CARTESIAN_POINT('Ctrl Pts',(369.824159291409,-1.06137786718031,-3.07098187056445));
#32425=CARTESIAN_POINT('Ctrl Pts',(370.111057419576,-1.0789288941631,-3.1407962439529));
#32426=CARTESIAN_POINT('Ctrl Pts',(370.149961285456,-1.08131960619163,-3.14950195723821));
#32427=CARTESIAN_POINT('Ctrl Pts',(370.206896899095,-1.08483834895031,-3.16113802495101));
#32428=CARTESIAN_POINT('Ctrl Pts',(370.224808845962,-1.08594819222272,-3.1646404875298));
#32429=CARTESIAN_POINT('Ctrl Pts',(370.256636412491,-1.08792571086705,-3.17058374627483));
#32430=CARTESIAN_POINT('Ctrl Pts',(370.270540252108,-1.08879142452289,-3.17308555598012));
#32431=CARTESIAN_POINT('Ctrl Pts',(370.299558095345,-1.09060221809778,-3.17811018587985));
#32432=CARTESIAN_POINT('Ctrl Pts',(370.314674512214,-1.09154778847688,-3.18061678569745));
#32433=CARTESIAN_POINT('Ctrl Pts',(370.35411655438,-1.09402114511627,-3.18686837266225));
#32434=CARTESIAN_POINT('Ctrl Pts',(370.378467863079,-1.09555427619082,-3.19044260952602));
#32435=CARTESIAN_POINT('Ctrl Pts',(370.488572378034,-1.10251525000373,-3.20531727181961));
#32436=CARTESIAN_POINT('Ctrl Pts',(370.574711758295,-1.10804147832615,-3.2134407039405));
#32437=CARTESIAN_POINT('Ctrl Pts',(370.821568205841,-1.12411413109601,-3.22673056888324));
#32438=CARTESIAN_POINT('Ctrl Pts',(370.982474373337,-1.13488682517902,-3.2233511231144));
#32439=CARTESIAN_POINT('Ctrl Pts',(371.341861005655,-1.15928453935056,-3.188832528809));
#32440=CARTESIAN_POINT('Ctrl Pts',(371.539076727275,-1.17291322313052,-3.15112375449813));
#32441=CARTESIAN_POINT('Ctrl Pts',(371.756682245187,-1.1874581157643,-3.0880491415532));
#32442=CARTESIAN_POINT('Ctrl Pts',(371.781749673725,-1.18912551484148,-3.08045071685477));
#32443=CARTESIAN_POINT('Ctrl Pts',(371.816474160178,-1.19142127359527,-3.06946105514844));
#32444=CARTESIAN_POINT('Ctrl Pts',(371.826211144869,-1.19206347904451,-3.06632840461775));
#32445=CARTESIAN_POINT('Ctrl Pts',(371.842960655554,-1.19316533845838,-3.06085150329645));
#32446=CARTESIAN_POINT('Ctrl Pts',(371.84998026352,-1.19362625193183,-3.05852940133607));
#32447=CARTESIAN_POINT('Ctrl Pts',(371.864712404777,-1.19459165733644,-3.05359966451514));
#32448=CARTESIAN_POINT('Ctrl Pts',(371.87242313574,-1.1950958270013,-3.05098693331585));
#32449=CARTESIAN_POINT('Ctrl Pts',(371.891403844221,-1.19633431212111,-3.04447515704058));
#32450=CARTESIAN_POINT('Ctrl Pts',(371.902662380794,-1.19706668372271,-3.04054267441853));
#32451=CARTESIAN_POINT('Ctrl Pts',(371.944185742159,-1.1997603834005,-3.02577990970987));
#32452=CARTESIAN_POINT('Ctrl Pts',(371.974310973774,-1.20170007273808,-3.01455911480811));
#32453=CARTESIAN_POINT('Ctrl Pts',(372.191003959864,-1.21558069741221,-2.93013400083984));
#32454=CARTESIAN_POINT('Ctrl Pts',(372.370573789216,-1.22671444366037,-2.84010917677809));
#32455=CARTESIAN_POINT('Ctrl Pts',(372.720749727295,-1.24979896747064,-2.62155897384041));
#32456=CARTESIAN_POINT('Ctrl Pts',(372.889296247283,-1.26172030412379,-2.4916354066685));
#32457=CARTESIAN_POINT('Ctrl Pts',(373.071210367654,-1.27655524376267,-2.32031106006873));
#32458=CARTESIAN_POINT('Ctrl Pts',(373.098130216951,-1.27880630825853,-2.29405425897784));
#32459=CARTESIAN_POINT('Ctrl Pts',(373.138959522668,-1.28231197424718,-2.25281199156576));
#32460=CARTESIAN_POINT('Ctrl Pts',(373.153196670712,-1.28355219909704,-2.23815461799345));
#32461=CARTESIAN_POINT('Ctrl Pts',(373.177154786331,-1.28567035139656,-2.21301536224042));
#32462=CARTESIAN_POINT('Ctrl Pts',(373.186947267432,-1.28654515905819,-2.20260226043797));
#32463=CARTESIAN_POINT('Ctrl Pts',(373.206641931004,-1.28832323032658,-2.18137822340416));
#32464=CARTESIAN_POINT('Ctrl Pts',(373.216540258109,-1.28922662740818,-2.17056418608468));
#32465=CARTESIAN_POINT('Ctrl Pts',(373.240805354749,-1.29146575083581,-2.14368837356616));
#32466=CARTESIAN_POINT('Ctrl Pts',(373.255085300534,-1.29280507188753,-2.12754949832327));
#32467=CARTESIAN_POINT('Ctrl Pts',(373.308170328472,-1.29786695920039,-2.06632759840005));
#32468=CARTESIAN_POINT('Ctrl Pts',(373.345884658877,-1.30163365504601,-2.02031859898814));
#32469=CARTESIAN_POINT('Ctrl Pts',(373.438102574751,-1.31129532845678,-1.90124372202778));
#32470=CARTESIAN_POINT('Ctrl Pts',(373.490817073044,-1.3172527418389,-1.82686400301371));
#32471=CARTESIAN_POINT('Ctrl Pts',(373.641287668174,-1.33562447680424,-1.5942418129601));
#32472=CARTESIAN_POINT('Ctrl Pts',(373.728566125857,-1.3482958169094,-1.4296872979638));
#32473=CARTESIAN_POINT('Ctrl Pts',(373.852277799476,-1.36961900811238,-1.13805333331055));
#32474=CARTESIAN_POINT('Ctrl Pts',(373.896008103865,-1.37832321889661,-1.01454819113308));
#32475=CARTESIAN_POINT('Ctrl Pts',(373.936749836048,-1.38773194568131,-0.872534610306835));
#32476=CARTESIAN_POINT('Ctrl Pts',(373.941264569694,-1.38879754095607,-0.856319439980352));
#32477=CARTESIAN_POINT('Ctrl Pts',(373.948289059589,-1.39049251698641,-0.83030308892697));
#32478=CARTESIAN_POINT('Ctrl Pts',(373.950879995614,-1.3911262894118,-0.820524413205781));
#32479=CARTESIAN_POINT('Ctrl Pts',(373.955403725724,-1.39224819039015,-0.803120423362795));
#32480=CARTESIAN_POINT('Ctrl Pts',(373.95735469988,-1.39273734364157,-0.795500029692975));
#32481=CARTESIAN_POINT('Ctrl Pts',(373.961492891511,-1.39378641395246,-0.779086604805082));
#32482=CARTESIAN_POINT('Ctrl Pts',(373.963670937942,-1.39434580655475,-0.770291460256281));
#32483=CARTESIAN_POINT('Ctrl Pts',(373.969633411637,-1.39589796082156,-0.745771740457222));
#32484=CARTESIAN_POINT('Ctrl Pts',(373.973336665247,-1.3968862002701,-0.730027439506591));
#32485=CARTESIAN_POINT('Ctrl Pts',(373.994609544274,-1.40271489282909,-0.6364303745155));
#32486=CARTESIAN_POINT('Ctrl Pts',(374.009402291824,-1.40741200451704,-0.557967959226293));
#32487=CARTESIAN_POINT('Ctrl Pts',(374.053625446024,-1.42459400019484,-0.26375515789267));
#32488=CARTESIAN_POINT('Ctrl Pts',(374.06408995392,-1.43650525950244,-0.0457438994967078));
#32489=CARTESIAN_POINT('Ctrl Pts',(374.044090560933,-1.45770381222186,0.329173123690029));
#32490=CARTESIAN_POINT('Ctrl Pts',(374.024138625789,-1.46677328981929,0.485829420408144));
#32491=CARTESIAN_POINT('Ctrl Pts',(373.987440996958,-1.47783059516145,0.666828332581764));
#32492=CARTESIAN_POINT('Ctrl Pts',(373.981747739896,-1.47945607316099,0.69320316397698));
#32493=CARTESIAN_POINT('Ctrl Pts',(373.971842047904,-1.48214638609823,0.7364521997205));
#32494=CARTESIAN_POINT('Ctrl Pts',(373.967822935575,-1.4832050357469,0.75336962714913));
#32495=CARTESIAN_POINT('Ctrl Pts',(373.960328439762,-1.48512214342538,0.783817910720799));
#32496=CARTESIAN_POINT('Ctrl Pts',(373.956901585872,-1.48597901921,0.797360349651279));
#32497=CARTESIAN_POINT('Ctrl Pts',(373.949378666447,-1.48781917211601,0.826297439133791));
#32498=CARTESIAN_POINT('Ctrl Pts',(373.945256296769,-1.48880328103639,0.8416848067446));
#32499=CARTESIAN_POINT('Ctrl Pts',(373.93371348638,-1.49149489473921,0.883526544361791));
#32500=CARTESIAN_POINT('Ctrl Pts',(373.92606868449,-1.49320963475085,0.909917121305269));
#32501=CARTESIAN_POINT('Ctrl Pts',(373.881561341171,-1.50283314718759,1.0565198829922));
#32502=CARTESIAN_POINT('Ctrl Pts',(373.838029912122,-1.51095849043888,1.17457833811883));
#32503=CARTESIAN_POINT('Ctrl Pts',(373.728443780192,-1.52904514437713,1.42551381175018));
#32504=CARTESIAN_POINT('Ctrl Pts',(373.659885128132,-1.53905743583866,1.55699020692286));
#32505=CARTESIAN_POINT('Ctrl Pts',(373.494568059308,-1.56047030815258,1.8268966065613));
#32506=CARTESIAN_POINT('Ctrl Pts',(373.395469777809,-1.57184192595846,1.96341383995172));
#32507=CARTESIAN_POINT('Ctrl Pts',(373.26866089881,-1.58439566804518,2.11206469754357));
#32508=CARTESIAN_POINT('Ctrl Pts',(373.250919526167,-1.58611173562044,2.13234139263423));
#32509=CARTESIAN_POINT('Ctrl Pts',(373.226029450301,-1.58846147549171,2.16007865739174));
#32510=CARTESIAN_POINT('Ctrl Pts',(373.219096588898,-1.58910991885919,2.16773027805698));
#32511=CARTESIAN_POINT('Ctrl Pts',(373.207128557573,-1.59021876940817,2.18081217873651));
#32512=CARTESIAN_POINT('Ctrl Pts',(373.202111275254,-1.59068048500793,2.18625861023046));
#32513=CARTESIAN_POINT('Ctrl Pts',(373.191566995393,-1.59164417799432,2.19762591134269));
#32514=CARTESIAN_POINT('Ctrl Pts',(373.186036385439,-1.59214585565961,2.20354330830963));
#32515=CARTESIAN_POINT('Ctrl Pts',(373.172429702683,-1.59337103548449,2.21799200737855));
#32516=CARTESIAN_POINT('Ctrl Pts',(373.164329079463,-1.59409268028318,2.22650022701476));
#32517=CARTESIAN_POINT('Ctrl Pts',(373.134705556481,-1.59670450296204,2.25727557349824));
#32518=CARTESIAN_POINT('Ctrl Pts',(373.112907758761,-1.59857468575869,2.27927725458802));
#32519=CARTESIAN_POINT('Ctrl Pts',(373.057342318869,-1.60322478800862,2.33376844138187));
#32520=CARTESIAN_POINT('Ctrl Pts',(373.023176196394,-1.60597880729982,2.36584287316793));
#32521=CARTESIAN_POINT('Ctrl Pts',(372.782942132503,-1.62473310043034,2.58170850428326));
#32522=CARTESIAN_POINT('Ctrl Pts',(372.554880914872,-1.63962221807123,2.73893445371739));
#32523=CARTESIAN_POINT('Ctrl Pts',(372.309820561358,-1.65539601866278,2.86513687644936));
#32524=CARTESIAN_POINT('Origin',(370.834317853224,2.31077344927308,0.));
#32525=CARTESIAN_POINT('',(372.309820619203,-3.1506689542051,2.86513684665969));
#32526=CARTESIAN_POINT('',(372.309820062099,-2.90499717006881,2.86513713356015));
#32527=CARTESIAN_POINT('',(372.309820613641,2.31077344927308,2.86513684952399));
#32528=CARTESIAN_POINT('Ctrl Pts',(372.309820619203,-3.15066895420512,2.86513684665975));
#32529=CARTESIAN_POINT('Ctrl Pts',(372.494256646546,-3.13828665471397,2.77015504193128));
#32530=CARTESIAN_POINT('Ctrl Pts',(372.669133387482,-3.12679078588963,2.65756409005948));
#32531=CARTESIAN_POINT('Ctrl Pts',(373.005201576513,-3.1028362123736,2.39209106534282));
#32532=CARTESIAN_POINT('Ctrl Pts',(373.1638668757,-3.09040604357014,2.23786073095912));
#32533=CARTESIAN_POINT('Ctrl Pts',(373.326034567183,-3.07530311480665,2.04413469922012));
#32534=CARTESIAN_POINT('Ctrl Pts',(373.346181511151,-3.07337874193438,2.01932654733445));
#32535=CARTESIAN_POINT('Ctrl Pts',(373.376401816767,-3.07041521406648,1.9809623083413));
#32536=CARTESIAN_POINT('Ctrl Pts',(373.386743446553,-3.069386754737,1.96761940384665));
#32537=CARTESIAN_POINT('Ctrl Pts',(373.40535132021,-3.06750962299772,1.94321771389924));
#32538=CARTESIAN_POINT('Ctrl Pts',(373.41365228426,-3.06666234481606,1.93218582322144));
#32539=CARTESIAN_POINT('Ctrl Pts',(373.43157897608,-3.06481066079082,1.90804005292954));
#32540=CARTESIAN_POINT('Ctrl Pts',(373.441176771508,-3.06380519967878,1.8949059999212));
#32541=CARTESIAN_POINT('Ctrl Pts',(373.467179785695,-3.06104185673471,1.858750842449));
#32542=CARTESIAN_POINT('Ctrl Pts',(373.483381889237,-3.05927626475275,1.83558609197985));
#32543=CARTESIAN_POINT('Ctrl Pts',(373.570646789636,-3.04951937512063,1.70725816895095));
#32544=CARTESIAN_POINT('Ctrl Pts',(373.635745837506,-3.04130827180882,1.59819299975049));
#32545=CARTESIAN_POINT('Ctrl Pts',(373.796919155135,-3.01819094818559,1.28791587900172));
#32546=CARTESIAN_POINT('Ctrl Pts',(373.878824763584,-3.00293452645181,1.08013824551366));
#32547=CARTESIAN_POINT('Ctrl Pts',(373.957898925665,-2.98323913304865,0.796553532431933));
#32548=CARTESIAN_POINT('Ctrl Pts',(373.974844834627,-2.97849086489083,0.726875368911395));
#32549=CARTESIAN_POINT('Ctrl Pts',(373.995204596727,-2.97199930026233,0.629054171290673));
#32550=CARTESIAN_POINT('Ctrl Pts',(374.00059264999,-2.9701799321999,0.601346972410001));
#32551=CARTESIAN_POINT('Ctrl Pts',(374.009366290876,-2.96703232330613,0.552837191185859));
#32552=CARTESIAN_POINT('Ctrl Pts',(374.012913064436,-2.96569656854798,0.532065859823218));
#32553=CARTESIAN_POINT('Ctrl Pts',(374.017852846103,-2.96373871675195,0.501322087933816));
#32554=CARTESIAN_POINT('Ctrl Pts',(374.019403179898,-2.96310828157868,0.491375981256995));
#32555=CARTESIAN_POINT('Ctrl Pts',(374.022078153826,-2.96199145007601,0.473670035722993));
#32556=CARTESIAN_POINT('Ctrl Pts',(374.023221103251,-2.96150404702677,0.465913192734428));
#32557=CARTESIAN_POINT('Ctrl Pts',(374.025643722601,-2.96044822465561,0.449044993440785));
#32558=CARTESIAN_POINT('Ctrl Pts',(374.026912688976,-2.95988040700818,0.439932301985312));
#32559=CARTESIAN_POINT('Ctrl Pts',(374.030330976285,-2.9583081940656,0.414590956494544));
#32560=CARTESIAN_POINT('Ctrl Pts',(374.032395731984,-2.95730840532546,0.398350914632495));
#32561=CARTESIAN_POINT('Ctrl Pts',(374.043099625045,-2.95182893089433,0.308706667371768));
#32562=CARTESIAN_POINT('Ctrl Pts',(374.049336058315,-2.94747060153796,0.235031937306053));
#32563=CARTESIAN_POINT('Ctrl Pts',(374.054526682938,-2.94146206873297,0.131390984773724));
#32564=CARTESIAN_POINT('Ctrl Pts',(374.055605511493,-2.93974684074643,0.101559832493373));
#32565=CARTESIAN_POINT('Ctrl Pts',(374.062344523622,-2.92244630848787,-0.201194939506387));
#32566=CARTESIAN_POINT('Ctrl Pts',(374.033722096033,-2.90765131912007,-0.473770361912933));
#32567=CARTESIAN_POINT('Ctrl Pts',(373.957751897544,-2.88848200898075,-0.796022256421406));
#32568=CARTESIAN_POINT('Ctrl Pts',(373.942897890869,-2.88508167084649,-0.852186159728038));
#32569=CARTESIAN_POINT('Ctrl Pts',(373.914552920897,-2.87911194319827,-0.948724627983305));
#32570=CARTESIAN_POINT('Ctrl Pts',(373.901764686171,-2.87656450191462,-0.989290738187691));
#32571=CARTESIAN_POINT('Ctrl Pts',(373.882137339628,-2.87284679953868,-1.04750724937452));
#32572=CARTESIAN_POINT('Ctrl Pts',(373.875939370931,-2.87169756811669,-1.06537016037872));
#32573=CARTESIAN_POINT('Ctrl Pts',(373.864826997929,-2.86967883432334,-1.09650912530368));
#32574=CARTESIAN_POINT('Ctrl Pts',(373.85998159342,-2.86881163910406,-1.10980937966301));
#32575=CARTESIAN_POINT('Ctrl Pts',(373.850414306301,-2.86712401918505,-1.13554243015719));
#32576=CARTESIAN_POINT('Ctrl Pts',(373.845702770833,-2.86630395457971,-1.14797878660509));
#32577=CARTESIAN_POINT('Ctrl Pts',(373.832932760268,-2.86411001695393,-1.18106630023375));
#32578=CARTESIAN_POINT('Ctrl Pts',(373.824738067992,-2.86273159804163,-1.2016637907445));
#32579=CARTESIAN_POINT('Ctrl Pts',(373.793888374753,-2.85764678191228,-1.27693470944716));
#32580=CARTESIAN_POINT('Ctrl Pts',(373.769942231703,-2.85389718068263,-1.33106299320422));
#32581=CARTESIAN_POINT('Ctrl Pts',(373.597518565078,-2.82813818248433,-1.69349588898913));
#32582=CARTESIAN_POINT('Ctrl Pts',(373.402293377525,-2.80440328879243,-1.97702303023724));
#32583=CARTESIAN_POINT('Ctrl Pts',(373.133702723644,-2.7787142723145,-2.2585751675315));
#32584=CARTESIAN_POINT('Ctrl Pts',(373.100472854419,-2.77563780842132,-2.29191503580343));
#32585=CARTESIAN_POINT('Ctrl Pts',(373.04411582136,-2.77060271084828,-2.34603401099087));
#32586=CARTESIAN_POINT('Ctrl Pts',(373.021397700749,-2.76861990629522,-2.36722718545441));
#32587=CARTESIAN_POINT('Ctrl Pts',(372.989664091348,-2.76591839539917,-2.39598380002527));
#32588=CARTESIAN_POINT('Ctrl Pts',(372.980909168495,-2.76518006843733,-2.40383059125255));
#32589=CARTESIAN_POINT('Ctrl Pts',(372.966052119984,-2.76393917270545,-2.41700065008793));
#32590=CARTESIAN_POINT('Ctrl Pts',(372.959972564941,-2.76343476037647,-2.42234910329179));
#32591=CARTESIAN_POINT('Ctrl Pts',(372.948298110935,-2.76247267481678,-2.4325418390364));
#32592=CARTESIAN_POINT('Ctrl Pts',(372.942706615918,-2.76201471386794,-2.43738982450511));
#32593=CARTESIAN_POINT('Ctrl Pts',(372.929286083695,-2.76092214591439,-2.44894506962848));
#32594=CARTESIAN_POINT('Ctrl Pts',(372.92144140854,-2.7602888581184,-2.45563415685052));
#32595=CARTESIAN_POINT('Ctrl Pts',(372.893062655972,-2.75801651238711,-2.47959824554528));
#32596=CARTESIAN_POINT('Ctrl Pts',(372.872344475811,-2.75639244273793,-2.49665480476884));
#32597=CARTESIAN_POINT('Ctrl Pts',(372.711363198381,-2.74401752239893,-2.62584563976042));
#32598=CARTESIAN_POINT('Ctrl Pts',(372.562143796891,-2.7339431749126,-2.72635256110259));
#32599=CARTESIAN_POINT('Ctrl Pts',(372.386727736572,-2.72270331291392,-2.82428647269521));
#32600=CARTESIAN_POINT('Ctrl Pts',(372.368042424455,-2.72151342772971,-2.83447693005543));
#32601=CARTESIAN_POINT('Ctrl Pts',(372.20761748265,-2.71135068793101,-2.91991749425213));
#32602=CARTESIAN_POINT('Ctrl Pts',(372.060547142384,-2.70237177119169,-2.98466531683603));
#32603=CARTESIAN_POINT('Ctrl Pts',(371.855266364946,-2.68975724797139,-3.05729681943449));
#32604=CARTESIAN_POINT('Ctrl Pts',(371.800759775434,-2.6864019789633,-3.07496165449587));
#32605=CARTESIAN_POINT('Ctrl Pts',(371.70544912243,-2.68050441865521,-3.10306603542138));
#32606=CARTESIAN_POINT('Ctrl Pts',(371.664857005002,-2.67798333924915,-3.11417613169469));
#32607=CARTESIAN_POINT('Ctrl Pts',(371.605806234928,-2.67429723771714,-3.1291017464783));
#32608=CARTESIAN_POINT('Ctrl Pts',(371.587512353206,-2.67315273965911,-3.13355550211132));
#32609=CARTESIAN_POINT('Ctrl Pts',(371.555410334917,-2.6711394837,-3.14107357779126));
#32610=CARTESIAN_POINT('Ctrl Pts',(371.541618975692,-2.67027299448701,-3.14420780171195));
#32611=CARTESIAN_POINT('Ctrl Pts',(371.514797943536,-2.66858463925068,-3.15011775623333));
#32612=CARTESIAN_POINT('Ctrl Pts',(371.501770792257,-2.66776311942222,-3.15290367710876));
#32613=CARTESIAN_POINT('Ctrl Pts',(371.466903465057,-2.66556019443596,-3.16013445135567));
#32614=CARTESIAN_POINT('Ctrl Pts',(371.445034127,-2.66417417490402,-3.1644335827799));
#32615=CARTESIAN_POINT('Ctrl Pts',(371.364125280448,-2.65902957096483,-3.17946890355102));
#32616=CARTESIAN_POINT('Ctrl Pts',(371.304836904047,-2.65522645119721,-3.18878181593822));
#32617=CARTESIAN_POINT('Ctrl Pts',(370.90696214042,-2.62946894115874,-3.23994190048388));
#32618=CARTESIAN_POINT('Ctrl Pts',(370.563934734911,-2.60580626478598,-3.22944375383793));
#32619=CARTESIAN_POINT('Ctrl Pts',(370.182792393523,-2.58018844944854,-3.15655565993993));
#32620=CARTESIAN_POINT('Ctrl Pts',(370.136799312273,-2.57711449721953,-3.14671215622166));
#32621=CARTESIAN_POINT('Ctrl Pts',(370.060825443393,-2.57208305160301,-3.12870436499419));
#32622=CARTESIAN_POINT('Ctrl Pts',(370.030718683315,-2.57010142920158,-3.12110718363619));
#32623=CARTESIAN_POINT('Ctrl Pts',(369.989371396378,-2.56740124674508,-3.11003556223163));
#32624=CARTESIAN_POINT('Ctrl Pts',(369.978034144666,-2.56666309066174,-3.10693320394771));
#32625=CARTESIAN_POINT('Ctrl Pts',(369.958916186123,-2.5654223979759,-3.10158911519372));
#32626=CARTESIAN_POINT('Ctrl Pts',(369.951126557931,-2.56491801917305,-3.09937997980737));
#32627=CARTESIAN_POINT('Ctrl Pts',(369.936232613975,-2.56395593034292,-3.09509535243999));
#32628=CARTESIAN_POINT('Ctrl Pts',(369.929127034355,-2.5634979330401,-3.09302472051063));
#32629=CARTESIAN_POINT('Ctrl Pts',(369.912138967854,-2.56240519314657,-3.08801068491246));
#32630=CARTESIAN_POINT('Ctrl Pts',(369.90226327888,-2.56177177068374,-3.08504427260112));
#32631=CARTESIAN_POINT('Ctrl Pts',(369.866724478313,-2.55949833130275,-3.07418306741917));
#32632=CARTESIAN_POINT('Ctrl Pts',(369.841145233227,-2.55787332181643,-3.06601479524194));
#32633=CARTESIAN_POINT('Ctrl Pts',(369.644643597079,-2.54545603494258,-3.00054819028005));
#32634=CARTESIAN_POINT('Ctrl Pts',(369.478676720308,-2.5353454816319,-2.92931182610317));
#32635=CARTESIAN_POINT('Ctrl Pts',(369.164500095966,-2.51543223185407,-2.76200530275248));
#32636=CARTESIAN_POINT('Ctrl Pts',(369.016490281316,-2.50565576365396,-2.66692011534032));
#32637=CARTESIAN_POINT('Ctrl Pts',(368.829083047009,-2.49201826760763,-2.5236451214449));
#32638=CARTESIAN_POINT('Ctrl Pts',(368.78223298039,-2.48849404448916,-2.48569877140857));
#32639=CARTESIAN_POINT('Ctrl Pts',(368.70325998499,-2.48232644594049,-2.41797943402869));
#32640=CARTESIAN_POINT('Ctrl Pts',(368.670628353227,-2.47970711428,-2.38882390574285));
#32641=CARTESIAN_POINT('Ctrl Pts',(368.624604875637,-2.47590336312598,-2.34598630615332));
#32642=CARTESIAN_POINT('Ctrl Pts',(368.610724675512,-2.4747413830775,-2.33283444496604));
#32643=CARTESIAN_POINT('Ctrl Pts',(368.586749548561,-2.47270782752138,-2.30970899196102));
#32644=CARTESIAN_POINT('Ctrl Pts',(368.576601838802,-2.47183866319166,-2.29979070781147));
#32645=CARTESIAN_POINT('Ctrl Pts',(368.555825838663,-2.47004146990439,-2.27921439274485));
#32646=CARTESIAN_POINT('Ctrl Pts',(368.545206068762,-2.46911309533973,-2.26854828789052));
#32647=CARTESIAN_POINT('Ctrl Pts',(368.518227578436,-2.46672933682199,-2.24106975716668));
#32648=CARTESIAN_POINT('Ctrl Pts',(368.501977214269,-2.4652692830166,-2.22415262844367));
#32649=CARTESIAN_POINT('Ctrl Pts',(368.438934229154,-2.45950783033517,-2.15707224315787));
#32650=CARTESIAN_POINT('Ctrl Pts',(368.39356628741,-2.45514687447327,-2.10560063082864));
#32651=CARTESIAN_POINT('Ctrl Pts',(368.139251992464,-2.42939235941282,-1.79780049246657));
#32652=CARTESIAN_POINT('Ctrl Pts',(367.969165400526,-2.40646284702157,-1.51204992548336));
#32653=CARTESIAN_POINT('Ctrl Pts',(367.828074730364,-2.38156851011381,-1.16223655203076));
#32654=CARTESIAN_POINT('Ctrl Pts',(367.811573820574,-2.3785215340526,-1.11861989520291));
#32655=CARTESIAN_POINT('Ctrl Pts',(367.785736607136,-2.37352934473963,-1.04557246561894));
#32656=CARTESIAN_POINT('Ctrl Pts',(367.775866518286,-2.37156044957382,-1.0163390131899));
#32657=CARTESIAN_POINT('Ctrl Pts',(367.762826646044,-2.3688745825874,-0.975805716625654));
#32658=CARTESIAN_POINT('Ctrl Pts',(367.759296811055,-2.3681382782774,-0.964624607078675));
#32659=CARTESIAN_POINT('Ctrl Pts',(367.753434371918,-2.36689979286245,-0.945695511522337));
#32660=CARTESIAN_POINT('Ctrl Pts',(367.751069802247,-2.36639578417202,-0.937957614790712));
#32661=CARTESIAN_POINT('Ctrl Pts',(367.746596362837,-2.36543369587093,-0.923118858001552));
#32662=CARTESIAN_POINT('Ctrl Pts',(367.744482806035,-2.36497533366303,-0.916019547807302));
#32663=CARTESIAN_POINT('Ctrl Pts',(367.739478989244,-2.36388080439427,-0.898997651218655));
#32664=CARTESIAN_POINT('Ctrl Pts',(367.736611924758,-2.36324596731442,-0.889068252945829));
#32665=CARTESIAN_POINT('Ctrl Pts',(367.726421249971,-2.3609606395984,-0.853127469308557));
#32666=CARTESIAN_POINT('Ctrl Pts',(367.71937686776,-2.35932536777931,-0.827037206556625));
#32667=CARTESIAN_POINT('Ctrl Pts',(367.671653771437,-2.34781390570902,-0.641018385861111));
#32668=CARTESIAN_POINT('Ctrl Pts',(367.642978621136,-2.3385060377231,-0.478242329656994));
#32669=CARTESIAN_POINT('Ctrl Pts',(367.623318008137,-2.32720143846736,-0.277395091620869));
#32670=CARTESIAN_POINT('Ctrl Pts',(367.620363661911,-2.32514723497933,-0.240762360852559));
#32671=CARTESIAN_POINT('Ctrl Pts',(367.613782807552,-2.3193367437615,-0.137052294487127));
#32672=CARTESIAN_POINT('Ctrl Pts',(367.611625986118,-2.31558027910065,-0.0699016882072931));
#32673=CARTESIAN_POINT('Ctrl Pts',(367.611426460719,-2.30232962703521,0.165325704249052));
#32674=CARTESIAN_POINT('Ctrl Pts',(367.624429434822,-2.29269715389302,0.333117854404309));
#32675=CARTESIAN_POINT('Ctrl Pts',(367.654675637949,-2.28100704750822,0.526057466281077));
#32676=CARTESIAN_POINT('Ctrl Pts',(367.659240257185,-2.27936465206984,0.552940562310314));
#32677=CARTESIAN_POINT('Ctrl Pts',(367.667288723925,-2.2766521683846,0.59695005685734));
#32678=CARTESIAN_POINT('Ctrl Pts',(367.670571784686,-2.27558844298291,0.614112099960196));
#32679=CARTESIAN_POINT('Ctrl Pts',(367.676731317483,-2.27366599201807,0.644949692272733));
#32680=CARTESIAN_POINT('Ctrl Pts',(367.679557503801,-2.27280888906427,0.658634924855483));
#32681=CARTESIAN_POINT('Ctrl Pts',(367.685782580613,-2.27097246476489,0.687818986536376));
#32682=CARTESIAN_POINT('Ctrl Pts',(367.689207098644,-2.26999234311787,0.703311913845366));
#32683=CARTESIAN_POINT('Ctrl Pts',(367.698810888621,-2.26732238908112,0.745287278058035));
#32684=CARTESIAN_POINT('Ctrl Pts',(367.705211061347,-2.26562551852846,0.771717347298704));
#32685=CARTESIAN_POINT('Ctrl Pts',(367.741910819588,-2.25631883178027,0.915302992611616));
#32686=CARTESIAN_POINT('Ctrl Pts',(367.778452717587,-2.24850926187905,1.03074879460554));
#32687=CARTESIAN_POINT('Ctrl Pts',(367.878772725009,-2.22987169017638,1.29499227150133));
#32688=CARTESIAN_POINT('Ctrl Pts',(367.947438512769,-2.21893049770601,1.44158675921385));
#32689=CARTESIAN_POINT('Ctrl Pts',(368.067193597863,-2.20243627285231,1.65405777584262));
#32690=CARTESIAN_POINT('Ctrl Pts',(368.110312478033,-2.19688499021178,1.72414596709367));
#32691=CARTESIAN_POINT('Ctrl Pts',(368.207602897065,-2.18522727202252,1.86951097632006));
#32692=CARTESIAN_POINT('Ctrl Pts',(368.262440819754,-2.1791443702264,1.9442619630939));
#32693=CARTESIAN_POINT('Ctrl Pts',(368.330365858588,-2.17223979953017,2.0289391690068));
#32694=CARTESIAN_POINT('Ctrl Pts',(368.340394132298,-2.17123539107492,2.04125310554076));
#32695=CARTESIAN_POINT('Ctrl Pts',(368.356844370827,-2.16961258071302,2.06115051165966));
#32696=CARTESIAN_POINT('Ctrl Pts',(368.363210971184,-2.16899043771208,2.06877912581562));
#32697=CARTESIAN_POINT('Ctrl Pts',(368.374658490684,-2.16788250678358,2.08236757388315));
#32698=CARTESIAN_POINT('Ctrl Pts',(368.37972593866,-2.16739577664318,2.08833843749012));
#32699=CARTESIAN_POINT('Ctrl Pts',(368.390857813417,-2.16633466372496,2.10135838373816));
#32700=CARTESIAN_POINT('Ctrl Pts',(368.396930998223,-2.16576093384717,2.10839971238249));
#32701=CARTESIAN_POINT('Ctrl Pts',(368.414382127844,-2.1641267384332,2.12845660094871));
#32702=CARTESIAN_POINT('Ctrl Pts',(368.425834635548,-2.16307160143824,2.1414072563427));
#32703=CARTESIAN_POINT('Ctrl Pts',(368.507648908458,-2.15565019748023,2.23243727316014));
#32704=CARTESIAN_POINT('Ctrl Pts',(368.581696551776,-2.14953410541245,2.30713382454027));
#32705=CARTESIAN_POINT('Ctrl Pts',(368.821603144342,-2.13097894252752,2.52655760934273));
#32706=CARTESIAN_POINT('Ctrl Pts',(368.998713745804,-2.11894688404738,2.65802146027684));
#32707=CARTESIAN_POINT('Ctrl Pts',(369.299829473686,-2.0990136181496,2.8369761854604));
#32708=CARTESIAN_POINT('Ctrl Pts',(369.415738243686,-2.09145740983911,2.89667303631612));
#32709=CARTESIAN_POINT('Ctrl Pts',(369.560961845954,-2.0819466673311,2.96065720434556));
#32710=CARTESIAN_POINT('Ctrl Pts',(369.587141089391,-2.08023084974059,2.97178004641657));
#32711=CARTESIAN_POINT('Ctrl Pts',(369.628555050189,-2.07751288666328,2.98873209583485));
#32712=CARTESIAN_POINT('Ctrl Pts',(369.64369303525,-2.0765186399789,2.99479481858454));
#32713=CARTESIAN_POINT('Ctrl Pts',(369.671729545066,-2.07467555498135,3.00577719528103));
#32714=CARTESIAN_POINT('Ctrl Pts',(369.684614979387,-2.0738278341478,3.01072938246388));
#32715=CARTESIAN_POINT('Ctrl Pts',(369.713285015953,-2.07194003946472,3.0215370879688));
#32716=CARTESIAN_POINT('Ctrl Pts',(369.729084403441,-2.07089863658552,3.02735197829491));
#32717=CARTESIAN_POINT('Ctrl Pts',(369.774796307102,-2.06788209406325,3.0437704961702));
#32718=CARTESIAN_POINT('Ctrl Pts',(369.804820159089,-2.06589651441403,3.05405617533953));
#32719=CARTESIAN_POINT('Ctrl Pts',(369.87293830879,-2.06138062060792,3.07627375102281));
#32720=CARTESIAN_POINT('Ctrl Pts',(369.911111694824,-2.05884221388878,3.08794445917764));
#32721=CARTESIAN_POINT('Ctrl Pts',(370.03685612037,-2.05045400100331,3.12384816199758));
#32722=CARTESIAN_POINT('Ctrl Pts',(370.125230485309,-2.04451535904278,3.14508589738989));
#32723=CARTESIAN_POINT('Ctrl Pts',(370.350851779475,-2.02927120626128,3.18931323785587));
#32724=CARTESIAN_POINT('Ctrl Pts',(370.488907247141,-2.0198624217125,3.20720216957262));
#32725=CARTESIAN_POINT('Ctrl Pts',(370.79195465275,-1.99932174985938,3.22667341307807));
#32726=CARTESIAN_POINT('Ctrl Pts',(370.956815300839,-1.98821820321541,3.2246272095518));
#32727=CARTESIAN_POINT('Ctrl Pts',(371.147753243404,-1.97590094640662,3.20758593100874));
#32728=CARTESIAN_POINT('Ctrl Pts',(371.174665544676,-1.97417783571976,3.20484208799174));
#32729=CARTESIAN_POINT('Ctrl Pts',(371.211812331567,-1.97182031607334,3.20058156702063));
#32730=CARTESIAN_POINT('Ctrl Pts',(371.22207799187,-1.97117101573503,3.19935408013054));
#32731=CARTESIAN_POINT('Ctrl Pts',(371.239689214252,-1.97006111120245,3.19716225793784));
#32732=CARTESIAN_POINT('Ctrl Pts',(371.247037609574,-1.96959919377444,3.19622196495526));
#32733=CARTESIAN_POINT('Ctrl Pts',(371.262404231841,-1.96863585265251,3.1942017892765));
#32734=CARTESIAN_POINT('Ctrl Pts',(371.270421722098,-1.96813472476631,3.19311704067928));
#32735=CARTESIAN_POINT('Ctrl Pts',(371.290044130519,-1.96691171723678,3.19038688892539));
#32736=CARTESIAN_POINT('Ctrl Pts',(371.301644464318,-1.96619168256136,3.188708326151));
#32737=CARTESIAN_POINT('Ctrl Pts',(371.343717274083,-1.96359020216431,3.18238588287451));
#32738=CARTESIAN_POINT('Ctrl Pts',(371.374132952802,-1.9617285541274,3.17736801370667));
#32739=CARTESIAN_POINT('Ctrl Pts',(371.450307084205,-1.95710353647795,3.16367562343212));
#32740=CARTESIAN_POINT('Ctrl Pts',(371.495959301325,-1.95436572106415,3.15444404045581));
#32741=CARTESIAN_POINT('Ctrl Pts',(371.808552996556,-1.93575593317946,3.08414735308054));
#32742=CARTESIAN_POINT('Ctrl Pts',(372.066748857434,-1.92098113377829,2.99031518462765));
#32743=CARTESIAN_POINT('Ctrl Pts',(372.309820657226,-1.90534924053903,2.86513682707866));
#32744=CARTESIAN_POINT('',(367.61156894943,-2.06176984286323,0.0015491427833167));
#32745=CARTESIAN_POINT('Ctrl Pts',(372.309820561358,-1.65539601866277,2.86513687644937));
#32746=CARTESIAN_POINT('Ctrl Pts',(372.256427656497,-1.65883275994792,2.89263342517085));
#32747=CARTESIAN_POINT('Ctrl Pts',(372.202227534331,-1.66230651349411,2.91865739099724));
#32748=CARTESIAN_POINT('Ctrl Pts',(372.088942520497,-1.6695691048338,2.96919430498641));
#32749=CARTESIAN_POINT('Ctrl Pts',(372.029849064809,-1.67335869469997,2.99347660446399));
#32750=CARTESIAN_POINT('Ctrl Pts',(371.948695006037,-1.67858363058956,3.02403754878361));
#32751=CARTESIAN_POINT('Ctrl Pts',(371.927229498561,-1.67996751717465,3.03186141330077));
#32752=CARTESIAN_POINT('Ctrl Pts',(371.891602832077,-1.68226826229659,3.04441930754466));
#32753=CARTESIAN_POINT('Ctrl Pts',(371.877488503411,-1.68318075362313,3.04928441268975));
#32754=CARTESIAN_POINT('Ctrl Pts',(371.849817280911,-1.68497186995512,3.0586078746352));
#32755=CARTESIAN_POINT('Ctrl Pts',(371.836263556777,-1.68585019417586,3.06307460162666));
#32756=CARTESIAN_POINT('Ctrl Pts',(371.804081815276,-1.68793827176251,3.0734438754171));
#32757=CARTESIAN_POINT('Ctrl Pts',(371.785429064989,-1.68915058944043,3.07926725591095));
#32758=CARTESIAN_POINT('Ctrl Pts',(371.722534160148,-1.69324588665021,3.09827703182328));
#32759=CARTESIAN_POINT('Ctrl Pts',(371.6780635561,-1.69615403627469,3.11068185585343));
#32760=CARTESIAN_POINT('Ctrl Pts',(371.570697304627,-1.70320842622309,3.1381594087761));
#32761=CARTESIAN_POINT('Ctrl Pts',(371.507586334424,-1.70738227212509,3.15230198587124));
#32762=CARTESIAN_POINT('Ctrl Pts',(371.25598829793,-1.72412475413989,3.20078270499804));
#32763=CARTESIAN_POINT('Ctrl Pts',(371.065040122354,-1.73708826581574,3.22018150893149));
#32764=CARTESIAN_POINT('Ctrl Pts',(370.794216674312,-1.75540057084861,3.22347637137753));
#32765=CARTESIAN_POINT('Ctrl Pts',(370.714899010365,-1.76074997606981,3.22151329963644));
#32766=CARTESIAN_POINT('Ctrl Pts',(370.543968104798,-1.77216053525531,3.21096050591037));
#32767=CARTESIAN_POINT('Ctrl Pts',(370.452479012519,-1.77819469180759,3.2013704385472));
#32768=CARTESIAN_POINT('Ctrl Pts',(370.345828073707,-1.78505214873581,3.18555283518526));
#32769=CARTESIAN_POINT('Ctrl Pts',(370.330155815924,-1.78605530746706,3.18311008201246));
#32770=CARTESIAN_POINT('Ctrl Pts',(370.304696405869,-1.78767684059574,3.17894910313233));
#32771=CARTESIAN_POINT('Ctrl Pts',(370.294898252696,-1.78829894048797,3.17730117844474));
#32772=CARTESIAN_POINT('Ctrl Pts',(370.277384095224,-1.78940725311997,3.1742721670413));
#32773=CARTESIAN_POINT('Ctrl Pts',(370.26966537397,-1.78989440474434,3.17290822164588));
#32774=CARTESIAN_POINT('Ctrl Pts',(370.252783819291,-1.79095699538033,3.16986159201016));
#32775=CARTESIAN_POINT('Ctrl Pts',(370.243623279859,-1.7915317760844,3.16816733636552));
#32776=CARTESIAN_POINT('Ctrl Pts',(370.21742640976,-1.7931706279896,3.16320461257788));
#32777=CARTESIAN_POINT('Ctrl Pts',(370.200408651208,-1.79422932871363,3.15983822816909));
#32778=CARTESIAN_POINT('Ctrl Pts',(370.079095348345,-1.80173947406436,3.13482099598137));
#32779=CARTESIAN_POINT('Ctrl Pts',(369.975891443623,-1.80793396323129,3.10814617211976));
#32780=CARTESIAN_POINT('Ctrl Pts',(369.656186870956,-1.82703720164101,3.00836811791855));
#32781=CARTESIAN_POINT('Ctrl Pts',(369.446032725797,-1.83951095116339,2.91735196177768));
#32782=CARTESIAN_POINT('Ctrl Pts',(369.141829889757,-1.8594617631227,2.74522785258736));
#32783=CARTESIAN_POINT('Ctrl Pts',(369.039858199459,-1.86650800055447,2.67968306097314));
#32784=CARTESIAN_POINT('Ctrl Pts',(368.91914078599,-1.87544936356169,2.59210333776315));
#32785=CARTESIAN_POINT('Ctrl Pts',(368.896673689478,-1.87714032265486,2.57535200160633));
#32786=CARTESIAN_POINT('Ctrl Pts',(368.861552889903,-1.87982794179045,2.54844639651482));
#32787=CARTESIAN_POINT('Ctrl Pts',(368.848752184977,-1.88081700477486,2.53848569002763));
#32788=CARTESIAN_POINT('Ctrl Pts',(368.825535570872,-1.88262856022891,2.52013692884033));
#32789=CARTESIAN_POINT('Ctrl Pts',(368.815095588292,-1.88344980725576,2.51177981404762));
#32790=CARTESIAN_POINT('Ctrl Pts',(368.804498644258,-1.88429027674603,2.50318828977826));
#32791=CARTESIAN_POINT('Ctrl Pts',(368.804289264825,-1.88430688589198,2.5030184908338));
#32792=CARTESIAN_POINT('Ctrl Pts',(368.80389752159,-1.8843379663048,2.50270072013022));
#32793=CARTESIAN_POINT('Ctrl Pts',(368.803715152861,-1.8843524372987,2.50255275487497));
#32794=CARTESIAN_POINT('Ctrl Pts',(368.803373368314,-1.88437956188626,2.50227538529875));
#32795=CARTESIAN_POINT('Ctrl Pts',(368.803213948856,-1.88439221527622,2.50214598581336));
#32796=CARTESIAN_POINT('Ctrl Pts',(368.802914734581,-1.88441596741558,2.50190306856553));
#32797=CARTESIAN_POINT('Ctrl Pts',(368.802774936996,-1.8844270660158,2.50178955438925));
#32798=CARTESIAN_POINT('Ctrl Pts',(368.802512214525,-1.88444792599529,2.50157618995164));
#32799=CARTESIAN_POINT('Ctrl Pts',(368.802389287178,-1.88445768729145,2.50147634209593));
#32800=CARTESIAN_POINT('Ctrl Pts',(368.802017404867,-1.88448722024115,2.50117423483383));
#32801=CARTESIAN_POINT('Ctrl Pts',(368.801768473088,-1.88450699300504,2.50097194760267));
#32802=CARTESIAN_POINT('Ctrl Pts',(368.801276676802,-1.88454606432086,2.50057218161234));
#32803=CARTESIAN_POINT('Ctrl Pts',(368.801033810647,-1.88456536281757,2.50037470445559));
#32804=CARTESIAN_POINT('Ctrl Pts',(368.800553708391,-1.88460351979304,2.49998421179604));
#32805=CARTESIAN_POINT('Ctrl Pts',(368.800316471404,-1.88462237817355,2.49979119823808));
#32806=CARTESIAN_POINT('Ctrl Pts',(368.7998472235,-1.8846596865331,2.49940931197583));
#32807=CARTESIAN_POINT('Ctrl Pts',(368.79961521128,-1.88467813646258,2.49922044063089));
#32808=CARTESIAN_POINT('Ctrl Pts',(368.799156037245,-1.88471465734252,2.49884654012972));
#32809=CARTESIAN_POINT('Ctrl Pts',(368.798928873944,-1.8847327282719,2.49866151196304));
#32810=CARTESIAN_POINT('Ctrl Pts',(368.786018800195,-1.88575991516695,2.48814312017868));
#32811=CARTESIAN_POINT('Ctrl Pts',(368.773414922018,-1.88677291736464,2.47771352046107));
#32812=CARTESIAN_POINT('Ctrl Pts',(368.746534915753,-1.88895554737861,2.45512354789626));
#32813=CARTESIAN_POINT('Ctrl Pts',(368.73228448108,-1.89012636229239,2.4429336683449));
#32814=CARTESIAN_POINT('Ctrl Pts',(368.695217002445,-1.89320832797246,2.41066152700094));
#32815=CARTESIAN_POINT('Ctrl Pts',(368.672576686812,-1.89512763637953,2.39037998569962));
#32816=CARTESIAN_POINT('Ctrl Pts',(368.605235293649,-1.9009500001155,2.32831532375715));
#32817=CARTESIAN_POINT('Ctrl Pts',(368.561435915633,-1.90489193131936,2.2855783122875));
#32818=CARTESIAN_POINT('Ctrl Pts',(368.393364739012,-1.92064500992626,2.11197278671562));
#32819=CARTESIAN_POINT('Ctrl Pts',(368.278971183362,-1.93281174592096,1.97202224398151));
#32820=CARTESIAN_POINT('Ctrl Pts',(368.07864342318,-1.95676751090956,1.68004163338432));
#32821=CARTESIAN_POINT('Ctrl Pts',(367.992114455196,-1.96850972103909,1.52910839604845));
#32822=CARTESIAN_POINT('Ctrl Pts',(367.906684779315,-1.98140340992467,1.34751978341968));
#32823=CARTESIAN_POINT('Ctrl Pts',(367.895509715891,-1.98312141594579,1.32297083285518));
#32824=CARTESIAN_POINT('Ctrl Pts',(367.880481183239,-1.98547355709268,1.28882630959208));
#32825=CARTESIAN_POINT('Ctrl Pts',(367.876364059119,-1.98612248703803,1.27934893129843));
#32826=CARTESIAN_POINT('Ctrl Pts',(367.869372724665,-1.98723214000185,1.26304111465651));
#32827=CARTESIAN_POINT('Ctrl Pts',(367.866476389915,-1.98769417265049,1.25622033257258));
#32828=CARTESIAN_POINT('Ctrl Pts',(367.860463652257,-1.98865816994591,1.24192365003193));
#32829=CARTESIAN_POINT('Ctrl Pts',(367.857351870958,-1.98915983585674,1.23444590943358));
#32830=CARTESIAN_POINT('Ctrl Pts',(367.849796326701,-1.99038492395569,1.21609489440479));
#32831=CARTESIAN_POINT('Ctrl Pts',(367.845383700749,-1.99110648961312,1.20520876887073));
#32832=CARTESIAN_POINT('Ctrl Pts',(367.829556095328,-1.99371793443876,1.16553981950728));
#32833=CARTESIAN_POINT('Ctrl Pts',(367.818496149464,-1.99558782319623,1.13661598815687));
#32834=CARTESIAN_POINT('Ctrl Pts',(367.791755328348,-2.00023710176736,1.0635437667978));
#32835=CARTESIAN_POINT('Ctrl Pts',(367.776616630551,-2.00299059945996,1.01920347747206));
#32836=CARTESIAN_POINT('Ctrl Pts',(367.662615351118,-2.02488194521479,0.659860088865763));
#32837=CARTESIAN_POINT('Ctrl Pts',(367.611727293097,-2.04248769501544,0.331713486549737));
#32838=CARTESIAN_POINT('Ctrl Pts',(367.611568227248,-2.06176838145633,0.00155266577040972));
#32839=CARTESIAN_POINT('Ctrl Pts',(367.611568225518,-2.06176859143958,0.00154907003543143));
#32840=CARTESIAN_POINT('Ctrl Pts',(367.611546633093,-2.06439192849467,-0.0433727063854235));
#32841=CARTESIAN_POINT('Ctrl Pts',(367.612464284761,-2.0670394314014,-0.0882888458202929));
#32842=CARTESIAN_POINT('Ctrl Pts',(367.615628263428,-2.07159962404561,-0.164792515275044));
#32843=CARTESIAN_POINT('Ctrl Pts',(367.617401797135,-2.07349803938567,-0.196393052452183));
#32844=CARTESIAN_POINT('Ctrl Pts',(367.620729361154,-2.07634126754824,-0.243317832966538));
#32845=CARTESIAN_POINT('Ctrl Pts',(367.621928323142,-2.07727507846268,-0.258665920748005));
#32846=CARTESIAN_POINT('Ctrl Pts',(367.624351168571,-2.0790100022435,-0.287059427078281));
#32847=CARTESIAN_POINT('Ctrl Pts',(367.62554473616,-2.07981015341681,-0.300107158391464));
#32848=CARTESIAN_POINT('Ctrl Pts',(367.62809848877,-2.08142023748647,-0.326264710521572));
#32849=CARTESIAN_POINT('Ctrl Pts',(367.629459599074,-2.08223018463649,-0.339374184267279));
#32850=CARTESIAN_POINT('Ctrl Pts',(367.632802323081,-2.08411431600601,-0.369754054174064));
#32851=CARTESIAN_POINT('Ctrl Pts',(367.63484332118,-2.08519034836884,-0.3870173770874));
#32852=CARTESIAN_POINT('Ctrl Pts',(367.640404633975,-2.08794597749298,-0.431001488096569));
#32853=CARTESIAN_POINT('Ctrl Pts',(367.644120609317,-2.08963167681436,-0.457695760212168));
#32854=CARTESIAN_POINT('Ctrl Pts',(367.661353683028,-2.09684869458605,-0.571060639319669));
#32855=CARTESIAN_POINT('Ctrl Pts',(367.678070430414,-2.10247912570915,-0.657199931490127));
#32856=CARTESIAN_POINT('Ctrl Pts',(367.738432555735,-2.11958476397544,-0.912131615638865));
#32857=CARTESIAN_POINT('Ctrl Pts',(367.792273324021,-2.13133289366246,-1.07816676233011));
#32858=CARTESIAN_POINT('Ctrl Pts',(367.931791879193,-2.15588417851675,-1.41317009708529));
#32859=CARTESIAN_POINT('Ctrl Pts',(368.0194799626,-2.16864660013255,-1.58063575687867));
#32860=CARTESIAN_POINT('Ctrl Pts',(368.131533699801,-2.18187099570145,-1.75540110910275));
#32861=CARTESIAN_POINT('Ctrl Pts',(368.141881798728,-2.18306780038168,-1.77123216044541));
#32862=CARTESIAN_POINT('Ctrl Pts',(368.157714737254,-2.18486142011126,-1.79499478286253));
#32863=CARTESIAN_POINT('Ctrl Pts',(368.16309658641,-2.18546472374789,-1.80299402669822));
#32864=CARTESIAN_POINT('Ctrl Pts',(368.172480589219,-2.18650553100239,-1.81680757406896));
#32865=CARTESIAN_POINT('Ctrl Pts',(368.176466002879,-2.18694413230798,-1.82263296515406));
#32866=CARTESIAN_POINT('Ctrl Pts',(368.185706266837,-2.18795314990762,-1.83604449427088));
#32867=CARTESIAN_POINT('Ctrl Pts',(368.190974577409,-2.18852264380473,-1.84362117899666));
#32868=CARTESIAN_POINT('Ctrl Pts',(368.205738330371,-2.19010285076731,-1.86466046566565));
#32869=CARTESIAN_POINT('Ctrl Pts',(368.215304715869,-2.1911088859725,-1.87807326077123));
#32870=CARTESIAN_POINT('Ctrl Pts',(368.269333861316,-2.19669551929634,-1.95261048438364));
#32871=CARTESIAN_POINT('Ctrl Pts',(368.315837006173,-2.20114909003744,-2.01223426153285));
#32872=CARTESIAN_POINT('Ctrl Pts',(368.381480855756,-2.20706066195212,-2.09055386817888));
#32873=CARTESIAN_POINT('Ctrl Pts',(368.398815907494,-2.20858886995154,-2.11072384266777));
#32874=CARTESIAN_POINT('Ctrl Pts',(368.597656367092,-2.22578045549424,-2.33637044740378));
#32875=CARTESIAN_POINT('Ctrl Pts',(368.804416905435,-2.24063341297452,-2.51809342576822));
#32876=CARTESIAN_POINT('Ctrl Pts',(369.079939811531,-2.25987609302753,-2.70400861958595));
#32877=CARTESIAN_POINT('Ctrl Pts',(369.129055609753,-2.26328285912067,-2.7352486258766));
#32878=CARTESIAN_POINT('Ctrl Pts',(369.204172117929,-2.26847708825232,-2.78021652995913));
#32879=CARTESIAN_POINT('Ctrl Pts',(369.22956003075,-2.27022992155853,-2.7949474629069));
#32880=CARTESIAN_POINT('Ctrl Pts',(369.276592838333,-2.27347453210016,-2.82138542232974));
#32881=CARTESIAN_POINT('Ctrl Pts',(369.29817755057,-2.27496257576627,-2.83319534143244));
#32882=CARTESIAN_POINT('Ctrl Pts',(369.329969612686,-2.27715375935871,-2.85012003224718));
#32883=CARTESIAN_POINT('Ctrl Pts',(369.340072617701,-2.27784999996492,-2.8554297396209));
#32884=CARTESIAN_POINT('Ctrl Pts',(369.362342841243,-2.27938467181118,-2.86698345874105));
#32885=CARTESIAN_POINT('Ctrl Pts',(369.37452198169,-2.2802239124323,-2.87320388989754));
#32886=CARTESIAN_POINT('Ctrl Pts',(369.401230291938,-2.2820644191832,-2.88663136470035));
#32887=CARTESIAN_POINT('Ctrl Pts',(369.415774952658,-2.28306676995659,-2.89380659648641));
#32888=CARTESIAN_POINT('Ctrl Pts',(369.455593469559,-2.28581135181107,-2.91307770225725));
#32889=CARTESIAN_POINT('Ctrl Pts',(369.480971438898,-2.2875611135408,-2.92495402163588));
#32890=CARTESIAN_POINT('Ctrl Pts',(369.617033355851,-2.29694747097019,-2.98647812592677));
#32891=CARTESIAN_POINT('Ctrl Pts',(369.730287102389,-2.30478386760349,-3.03017214018948));
#32892=CARTESIAN_POINT('Ctrl Pts',(370.061681290645,-2.32776056841907,-3.13697829753263));
#32893=CARTESIAN_POINT('Ctrl Pts',(370.284380038398,-2.34330083795763,-3.18357561894358));
#32894=CARTESIAN_POINT('Ctrl Pts',(370.582674517578,-2.3633685698636,-3.21373847321718));
#32895=CARTESIAN_POINT('Ctrl Pts',(370.655487941078,-2.3682035039931,-3.21861158485213));
#32896=CARTESIAN_POINT('Ctrl Pts',(370.770878612462,-2.37570704911475,-3.22240573385288));
#32897=CARTESIAN_POINT('Ctrl Pts',(370.813374951208,-2.37843641072064,-3.22296215457504));
#32898=CARTESIAN_POINT('Ctrl Pts',(370.869107368796,-2.38196067640316,-3.22258939845419));
#32899=CARTESIAN_POINT('Ctrl Pts',(370.882342189019,-2.38279350117328,-3.22241934247874));
#32900=CARTESIAN_POINT('Ctrl Pts',(370.903989983376,-2.38414863332975,-3.22200778707792));
#32901=CARTESIAN_POINT('Ctrl Pts',(370.912403571084,-2.3846735628551,-3.22181486280806));
#32902=CARTESIAN_POINT('Ctrl Pts',(370.928827448387,-2.3856947092498,-3.22137388729834));
#32903=CARTESIAN_POINT('Ctrl Pts',(370.936837692888,-2.38619108357238,-3.22112891229201));
#32904=CARTESIAN_POINT('Ctrl Pts',(370.956558825057,-2.38740924266884,-3.22045214769007));
#32905=CARTESIAN_POINT('Ctrl Pts',(370.968268575687,-2.38812915185582,-3.2199863516109));
#32906=CARTESIAN_POINT('Ctrl Pts',(371.008580204285,-2.39059659983677,-3.21816253257003));
#32907=CARTESIAN_POINT('Ctrl Pts',(371.037167278517,-2.39232751339454,-3.21648716642913));
#32908=CARTESIAN_POINT('Ctrl Pts',(371.389293736767,-2.41345692753949,-3.19113707990928));
#32909=CARTESIAN_POINT('Ctrl Pts',(371.707529922617,-2.43072098806815,-3.11912207645665));
#32910=CARTESIAN_POINT('Ctrl Pts',(372.118449290802,-2.45596755326888,-2.95816981991702));
#32911=CARTESIAN_POINT('Ctrl Pts',(372.224806962655,-2.46277778123383,-2.90969035176546));
#32912=CARTESIAN_POINT('Ctrl Pts',(372.352167340394,-2.47140557027467,-2.84305761203099));
#32913=CARTESIAN_POINT('Ctrl Pts',(372.375884956472,-2.47303305553731,-2.83026755807345));
#32914=CARTESIAN_POINT('Ctrl Pts',(372.413268377565,-2.47563279096866,-2.809498725831));
#32915=CARTESIAN_POINT('Ctrl Pts',(372.427040927419,-2.47659811348342,-2.80171394752034));
#32916=CARTESIAN_POINT('Ctrl Pts',(372.452885742144,-2.47842412816016,-2.78685330531481));
#32917=CARTESIAN_POINT('Ctrl Pts',(372.464970363672,-2.47928400609428,-2.77979958571805));
#32918=CARTESIAN_POINT('Ctrl Pts',(372.492129672036,-2.48123043958634,-2.76370882018954));
#32919=CARTESIAN_POINT('Ctrl Pts',(372.507177042042,-2.48231861714963,-2.75462675950499));
#32920=CARTESIAN_POINT('Ctrl Pts',(372.545647251175,-2.48512625548045,-2.73097603571204));
#32921=CARTESIAN_POINT('Ctrl Pts',(372.568958320109,-2.4868522174586,-2.71622914913098));
#32922=CARTESIAN_POINT('Ctrl Pts',(372.752800690613,-2.50066485059672,-2.59659627707509));
#32923=CARTESIAN_POINT('Ctrl Pts',(372.903842121649,-2.51327904557552,-2.47788936103686));
#32924=CARTESIAN_POINT('Ctrl Pts',(373.179072185367,-2.53869480083802,-2.21877367999824));
#32925=CARTESIAN_POINT('Ctrl Pts',(373.303395187075,-2.55142849190428,-2.07954034199217));
#32926=CARTESIAN_POINT('Ctrl Pts',(373.460739176643,-2.56881759540263,-1.8691874027074));
#32927=CARTESIAN_POINT('Ctrl Pts',(373.504300779354,-2.57379713306532,-1.80641736822578));
#32928=CARTESIAN_POINT('Ctrl Pts',(373.554235222029,-2.57966059369886,-1.72870546663604));
#32929=CARTESIAN_POINT('Ctrl Pts',(373.562776437828,-2.58066944973846,-1.71519295128393));
#32930=CARTESIAN_POINT('Ctrl Pts',(373.575980673352,-2.58223776543875,-1.69395511820842));
#32931=CARTESIAN_POINT('Ctrl Pts',(373.58071225831,-2.58280154183277,-1.68627303191747));
#32932=CARTESIAN_POINT('Ctrl Pts',(373.589512585921,-2.58385333842673,-1.67184973663547));
#32933=CARTESIAN_POINT('Ctrl Pts',(373.593588854309,-2.58434182656368,-1.66511353996758));
#32934=CARTESIAN_POINT('Ctrl Pts',(373.602878870233,-2.58545820722565,-1.64963362200546));
#32935=CARTESIAN_POINT('Ctrl Pts',(373.608075909937,-2.58608501793485,-1.64088008127678));
#32936=CARTESIAN_POINT('Ctrl Pts',(373.624485834297,-2.58807201306248,-1.61293957000483));
#32937=CARTESIAN_POINT('Ctrl Pts',(373.635542051682,-2.58942253808624,-1.5936607140069));
#32938=CARTESIAN_POINT('Ctrl Pts',(373.648990927178,-2.59108214438442,-1.56963728881009));
#32939=CARTESIAN_POINT('Ctrl Pts',(373.651572122507,-2.59140145520163,-1.56499971714145));
#32940=CARTESIAN_POINT('Ctrl Pts',(373.759866287628,-2.60483243227363,-1.3692940353964));
#32941=CARTESIAN_POINT('Ctrl Pts',(373.845913690395,-2.61691322161687,-1.1679541444941));
#32942=CARTESIAN_POINT('Ctrl Pts',(373.955451091337,-2.63749536761685,-0.816700205933311));
#32943=CARTESIAN_POINT('Ctrl Pts',(373.989973260656,-2.64589345959054,-0.67104871204428));
#32944=CARTESIAN_POINT('Ctrl Pts',(374.023189153743,-2.65775822384725,-0.469296341066459));
#32945=CARTESIAN_POINT('Ctrl Pts',(374.030729409801,-2.6609820745336,-0.414839613979763));
#32946=CARTESIAN_POINT('Ctrl Pts',(374.041430004338,-2.6666689564829,-0.319705078219756));
#32947=CARTESIAN_POINT('Ctrl Pts',(374.045217580092,-2.66911285026489,-0.2791100250101));
#32948=CARTESIAN_POINT('Ctrl Pts',(374.049610226146,-2.6727067626466,-0.219905671871226));
#32949=CARTESIAN_POINT('Ctrl Pts',(374.050825871232,-2.67383770653679,-0.201344718078478));
#32950=CARTESIAN_POINT('Ctrl Pts',(374.052681399325,-2.67583587484425,-0.168680009214052));
#32951=CARTESIAN_POINT('Ctrl Pts',(374.053389414298,-2.67670094369416,-0.154580513190758));
#32952=CARTESIAN_POINT('Ctrl Pts',(374.054589081127,-2.67839314300787,-0.127084540769422));
#32953=CARTESIAN_POINT('Ctrl Pts',(374.055089829709,-2.67921997022517,-0.113688735568026));
#32954=CARTESIAN_POINT('Ctrl Pts',(374.05621307486,-2.68145340217471,-0.0776116366943328));
#32955=CARTESIAN_POINT('Ctrl Pts',(374.056679629077,-2.6828648505158,-0.0549265746182278));
#32956=CARTESIAN_POINT('Ctrl Pts',(374.05753450255,-2.68820931738686,0.0305261789265668));
#32957=CARTESIAN_POINT('Ctrl Pts',(374.056328570001,-2.69219145687869,0.0932924190315749));
#32958=CARTESIAN_POINT('Ctrl Pts',(374.036946291238,-2.71794374131263,0.493285979181566));
#32959=CARTESIAN_POINT('Ctrl Pts',(373.967699108441,-2.74136510917914,0.825832790318517));
#32960=CARTESIAN_POINT('Ctrl Pts',(373.8315113794,-2.76674557473438,1.18538961381349));
#32961=CARTESIAN_POINT('Ctrl Pts',(373.813941009317,-2.76981131404731,1.22888724651558));
#32962=CARTESIAN_POINT('Ctrl Pts',(373.783194111084,-2.7748311099694,1.30046411082045));
#32963=CARTESIAN_POINT('Ctrl Pts',(373.770551066057,-2.7768091516012,1.32876362560782));
#32964=CARTESIAN_POINT('Ctrl Pts',(373.752553770127,-2.77950563687249,1.36753602381804));
#32965=CARTESIAN_POINT('Ctrl Pts',(373.747547983375,-2.78024359871316,1.37816757398072));
#32966=CARTESIAN_POINT('Ctrl Pts',(373.738993407933,-2.78148432513536,1.39608133713833));
#32967=CARTESIAN_POINT('Ctrl Pts',(373.735475138047,-2.78198892871152,1.40337792195803));
#32968=CARTESIAN_POINT('Ctrl Pts',(373.728686130343,-2.78295174815612,1.41732308822957));
#32969=CARTESIAN_POINT('Ctrl Pts',(373.725419936904,-2.78341024972644,1.42397373724846));
#32970=CARTESIAN_POINT('Ctrl Pts',(373.717545398587,-2.78450460115969,1.43986915510599));
#32971=CARTESIAN_POINT('Ctrl Pts',(373.712915452721,-2.7851391245458,1.44910321546769));
#32972=CARTESIAN_POINT('Ctrl Pts',(373.696047624343,-2.78741952614218,1.48234489805956));
#32973=CARTESIAN_POINT('Ctrl Pts',(373.683552774476,-2.78905028160114,1.50622181331525));
#32974=CARTESIAN_POINT('Ctrl Pts',(373.591263161743,-2.80070406741627,1.67732269595656));
#32975=CARTESIAN_POINT('Ctrl Pts',(373.500390394921,-2.81014106916837,1.81830407623108));
#32976=CARTESIAN_POINT('Ctrl Pts',(373.304333824479,-2.82827230167331,2.07594697970285));
#32977=CARTESIAN_POINT('Ctrl Pts',(373.200790340985,-2.83695256375842,2.19324887137075));
#32978=CARTESIAN_POINT('Ctrl Pts',(373.004070942733,-2.85269064435811,2.38588964324588));
#32979=CARTESIAN_POINT('Ctrl Pts',(372.914446505848,-2.85962817517038,2.46441840999463));
#32980=CARTESIAN_POINT('Ctrl Pts',(372.79935786551,-2.86839971160625,2.55449977818439));
#32981=CARTESIAN_POINT('Ctrl Pts',(372.77781721384,-2.87003566975625,2.57092620157335));
#32982=CARTESIAN_POINT('Ctrl Pts',(372.743347608119,-2.87264582586219,2.59653119174095));
#32983=CARTESIAN_POINT('Ctrl Pts',(372.730553296375,-2.87361299875585,2.60588947671575));
#32984=CARTESIAN_POINT('Ctrl Pts',(372.706339610666,-2.87544057515436,2.62332761481063));
#32985=CARTESIAN_POINT('Ctrl Pts',(372.694935621003,-2.87630014830955,2.63142827137717));
#32986=CARTESIAN_POINT('Ctrl Pts',(372.669123861875,-2.87824328090601,2.64951159709431));
#32987=CARTESIAN_POINT('Ctrl Pts',(372.654686749923,-2.87932843979613,2.65945141956297));
#32988=CARTESIAN_POINT('Ctrl Pts',(372.617454031289,-2.88212309541942,2.68464058928198));
#32989=CARTESIAN_POINT('Ctrl Pts',(372.594543908417,-2.8838389925197,2.69971737096328));
#32990=CARTESIAN_POINT('Ctrl Pts',(372.486580169867,-2.89190973654399,2.76880808397516));
#32991=CARTESIAN_POINT('Ctrl Pts',(372.399273068547,-2.89839472972295,2.81907019070487));
#32992=CARTESIAN_POINT('Ctrl Pts',(372.309820062099,-2.90499717006879,2.86513713356016));
#32993=CARTESIAN_POINT('Origin',(370.834317853224,2.31077344927308,0.));
#32994=CARTESIAN_POINT('',(372.30982074573,-4.40407334669084,2.86513678150015));
#32995=CARTESIAN_POINT('',(372.309820591895,-4.15988901539236,2.86513686072291));
#32996=CARTESIAN_POINT('',(372.309820613641,2.31077344927308,2.86513684952399));
#32997=CARTESIAN_POINT('',(367.611567856376,-3.55765537866733,-0.00014252679442044));
#32998=CARTESIAN_POINT('Ctrl Pts',(372.30982074573,-4.40407334669084,2.86513678150013));
#32999=CARTESIAN_POINT('Ctrl Pts',(372.356820336721,-4.40050650002824,2.84093269012777));
#33000=CARTESIAN_POINT('Ctrl Pts',(372.403229895877,-4.39692788281758,2.8155692833783));
#33001=CARTESIAN_POINT('Ctrl Pts',(372.594590100041,-4.38196998916824,2.70478418667755));
#33002=CARTESIAN_POINT('Ctrl Pts',(372.733365395875,-4.37061300566367,2.60922306379554));
#33003=CARTESIAN_POINT('Ctrl Pts',(372.88497741809,-4.35807259069125,2.48629010110657));
#33004=CARTESIAN_POINT('Ctrl Pts',(372.905687217492,-4.35635683435112,2.46906301756107));
#33005=CARTESIAN_POINT('Ctrl Pts',(372.934032335231,-4.35400751349806,2.44487693464788));
#33006=CARTESIAN_POINT('Ctrl Pts',(372.941853200669,-4.353359192509,2.43813840821318));
#33007=CARTESIAN_POINT('Ctrl Pts',(372.955227619482,-4.35225052391116,2.42650245145076));
#33008=CARTESIAN_POINT('Ctrl Pts',(372.960796865606,-4.35178886936453,2.42162329771172));
#33009=CARTESIAN_POINT('Ctrl Pts',(372.972418853882,-4.35082558807084,2.41137039542081));
#33010=CARTESIAN_POINT('Ctrl Pts',(372.978468234431,-4.35032425993365,2.4059929795146));
#33011=CARTESIAN_POINT('Ctrl Pts',(372.993241635538,-4.34909994440325,2.39276063782111));
#33012=CARTESIAN_POINT('Ctrl Pts',(373.001943227888,-4.34837881145916,2.38488062861831));
#33013=CARTESIAN_POINT('Ctrl Pts',(373.033427699975,-4.34576870835481,2.35605416646881));
#33014=CARTESIAN_POINT('Ctrl Pts',(373.055952412938,-4.34389970945168,2.33482663105801));
#33015=CARTESIAN_POINT('Ctrl Pts',(373.111778109745,-4.33925259613662,2.28067637627111));
#33016=CARTESIAN_POINT('Ctrl Pts',(373.144674672588,-4.3365003512048,2.24734549056114));
#33017=CARTESIAN_POINT('Ctrl Pts',(373.407319713652,-4.31429258103204,1.96936770421954));
#33018=CARTESIAN_POINT('Ctrl Pts',(373.598296227912,-4.2964143340372,1.69092014962956));
#33019=CARTESIAN_POINT('Ctrl Pts',(373.770608954436,-4.27299697573036,1.32983577508168));
#33020=CARTESIAN_POINT('Ctrl Pts',(373.79660581065,-4.26917547823155,1.27087286522773));
#33021=CARTESIAN_POINT('Ctrl Pts',(373.829427365802,-4.26391382785677,1.18994179907895));
#33022=CARTESIAN_POINT('Ctrl Pts',(373.837810954837,-4.26252612439066,1.16861953798211));
#33023=CARTESIAN_POINT('Ctrl Pts',(373.851282340918,-4.26022128232695,1.133254543545));
#33024=CARTESIAN_POINT('Ctrl Pts',(373.856501218672,-4.25930855223057,1.1192623795593));
#33025=CARTESIAN_POINT('Ctrl Pts',(373.866508753866,-4.25751865360689,1.09185113324143));
#33026=CARTESIAN_POINT('Ctrl Pts',(373.871306048396,-4.25664179745701,1.0784355553817));
#33027=CARTESIAN_POINT('Ctrl Pts',(373.882446480422,-4.25455993733679,1.04661755714939));
#33028=CARTESIAN_POINT('Ctrl Pts',(373.888712107683,-4.25335240176869,1.02818877184621));
#33029=CARTESIAN_POINT('Ctrl Pts',(373.90915164639,-4.24928650769127,0.966234959734304));
#33030=CARTESIAN_POINT('Ctrl Pts',(373.922564602881,-4.24640344643216,0.922466541764184));
#33031=CARTESIAN_POINT('Ctrl Pts',(373.952473300675,-4.23942067017441,0.816893334582244));
#33032=CARTESIAN_POINT('Ctrl Pts',(373.968069561371,-4.23529406305667,0.754855920454128));
#33033=CARTESIAN_POINT('Ctrl Pts',(374.022127095938,-4.21886069056194,0.509122368967236));
#33034=CARTESIAN_POINT('Ctrl Pts',(374.046356150456,-4.20617490837765,0.322691357908466));
#33035=CARTESIAN_POINT('Ctrl Pts',(374.057161237622,-4.18875979158576,0.0654234177713689));
#33036=CARTESIAN_POINT('Ctrl Pts',(374.057822188569,-4.18404169576746,-0.00446586208591672));
#33037=CARTESIAN_POINT('Ctrl Pts',(374.055220281539,-4.17649153413159,-0.117258592036203));
#33038=CARTESIAN_POINT('Ctrl Pts',(374.053371637904,-4.17363416235853,-0.160171786559151));
#33039=CARTESIAN_POINT('Ctrl Pts',(374.046481593723,-4.16642384790428,-0.269318549531825));
#33040=CARTESIAN_POINT('Ctrl Pts',(374.040249203542,-4.16210810448749,-0.33546077485909));
#33041=CARTESIAN_POINT('Ctrl Pts',(374.030001833576,-4.15688482982029,-0.417100557186794));
#33042=CARTESIAN_POINT('Ctrl Pts',(374.027910959258,-4.15588398668096,-0.432818754315248));
#33043=CARTESIAN_POINT('Ctrl Pts',(374.024439936618,-4.15431962361985,-0.457516299855573));
#33044=CARTESIAN_POINT('Ctrl Pts',(374.023137719238,-4.15375192185907,-0.466506096929454));
#33045=CARTESIAN_POINT('Ctrl Pts',(374.020754585345,-4.15274628160205,-0.482481584146566));
#33046=CARTESIAN_POINT('Ctrl Pts',(374.019688698739,-4.15230752304586,-0.489469207220433));
#33047=CARTESIAN_POINT('Ctrl Pts',(374.017088619077,-4.15126294634592,-0.506146271740775));
#33048=CARTESIAN_POINT('Ctrl Pts',(374.015533168222,-4.15065833349952,-0.515832261393103));
#33049=CARTESIAN_POINT('Ctrl Pts',(374.010710197986,-4.14884263443907,-0.545013738709289));
#33050=CARTESIAN_POINT('Ctrl Pts',(374.007307449573,-4.14763888316993,-0.564486819332759));
#33051=CARTESIAN_POINT('Ctrl Pts',(373.969765559872,-4.13511386628366,-0.768254366939748));
#33052=CARTESIAN_POINT('Ctrl Pts',(373.91978493487,-4.12458483459276,-0.949294351220609));
#33053=CARTESIAN_POINT('Ctrl Pts',(373.819833751023,-4.10856162533082,-1.21761392715217));
#33054=CARTESIAN_POINT('Ctrl Pts',(373.781084386549,-4.1030515975203,-1.30860822257572));
#33055=CARTESIAN_POINT('Ctrl Pts',(373.667695485865,-4.08830598020329,-1.544191875326));
#33056=CARTESIAN_POINT('Ctrl Pts',(373.586197573693,-4.07897021820306,-1.68514264495063));
#33057=CARTESIAN_POINT('Ctrl Pts',(373.479103553636,-4.06761338849572,-1.84172807314838));
#33058=CARTESIAN_POINT('Ctrl Pts',(373.463505062924,-4.065979013034,-1.86392817597613));
#33059=CARTESIAN_POINT('Ctrl Pts',(373.437427317206,-4.06327708255522,-1.90006383082037));
#33060=CARTESIAN_POINT('Ctrl Pts',(373.427111790021,-4.06221580468078,-1.91411625179955));
#33061=CARTESIAN_POINT('Ctrl Pts',(373.408324669152,-4.06029599635024,-1.93927864233283));
#33062=CARTESIAN_POINT('Ctrl Pts',(373.399893820278,-4.05943906902534,-1.95041859317688));
#33063=CARTESIAN_POINT('Ctrl Pts',(373.381716654477,-4.05760106768792,-1.97411487876878));
#33064=CARTESIAN_POINT('Ctrl Pts',(373.371949371963,-4.05661917912857,-1.9866545919824));
#33065=CARTESIAN_POINT('Ctrl Pts',(373.34514195245,-4.05393942922595,-2.0205510056913));
#33066=CARTESIAN_POINT('Ctrl Pts',(373.327922651327,-4.05223444196566,-2.04176371328451));
#33067=CARTESIAN_POINT('Ctrl Pts',(373.231612482809,-4.04278425163842,-2.15737387419143));
#33068=CARTESIAN_POINT('Ctrl Pts',(373.147439633739,-4.03483182100616,-2.24738622962639));
#33069=CARTESIAN_POINT('Ctrl Pts',(372.949899411766,-4.01681960922254,-2.43575054674697));
#33070=CARTESIAN_POINT('Ctrl Pts',(372.834394890547,-4.00669466629736,-2.5314525460864));
#33071=CARTESIAN_POINT('Ctrl Pts',(372.57499181843,-3.98509897833282,-2.71751277023943));
#33072=CARTESIAN_POINT('Ctrl Pts',(372.429735509719,-3.97365730965254,-2.80525842180363));
#33073=CARTESIAN_POINT('Ctrl Pts',(372.254162065999,-3.96103988422441,-2.89324824363864));
#33074=CARTESIAN_POINT('Ctrl Pts',(372.22993170662,-3.95932428414451,-2.90501378140044));
#33075=CARTESIAN_POINT('Ctrl Pts',(372.196213935869,-3.95697513767979,-2.92086685503076));
#33076=CARTESIAN_POINT('Ctrl Pts',(372.186850878523,-3.95632683767809,-2.9252142736942));
#33077=CARTESIAN_POINT('Ctrl Pts',(372.17073659314,-3.95521819550737,-2.9326024847951));
#33078=CARTESIAN_POINT('Ctrl Pts',(372.163995546321,-3.95475654653658,-2.93566510646598));
#33079=CARTESIAN_POINT('Ctrl Pts',(372.149863373954,-3.95379326605578,-2.94202703201353));
#33080=CARTESIAN_POINT('Ctrl Pts',(372.142470292408,-3.95329193321712,-2.94532176032525));
#33081=CARTESIAN_POINT('Ctrl Pts',(372.124324048026,-3.95206758840162,-2.95332683504522));
#33082=CARTESIAN_POINT('Ctrl Pts',(372.113557276421,-3.95134643108233,-2.95800640385837));
#33083=CARTESIAN_POINT('Ctrl Pts',(372.074312249028,-3.94873613852915,-2.97480914018418));
#33084=CARTESIAN_POINT('Ctrl Pts',(372.045684301878,-3.94686697834984,-2.986581157422));
#33085=CARTESIAN_POINT('Ctrl Pts',(371.973328101669,-3.94221938030647,-3.01512290463813));
#33086=CARTESIAN_POINT('Ctrl Pts',(371.929394637014,-3.93946681882986,-3.03135576059474));
#33087=CARTESIAN_POINT('Ctrl Pts',(371.567720028278,-3.91725038484891,-3.15609990962591));
#33088=CARTESIAN_POINT('Ctrl Pts',(371.23515525825,-3.89936487727849,-3.21530939151872));
#33089=CARTESIAN_POINT('Ctrl Pts',(370.835118414114,-3.87594445282317,-3.22339148369575));
#33090=CARTESIAN_POINT('Ctrl Pts',(370.770800946733,-3.87212983958409,-3.22276559302365));
#33091=CARTESIAN_POINT('Ctrl Pts',(370.683671783539,-3.86687626716856,-3.2193085411111));
#33092=CARTESIAN_POINT('Ctrl Pts',(370.660806061208,-3.86548954623362,-3.21815713379013));
#33093=CARTESIAN_POINT('Ctrl Pts',(370.623052479826,-3.8631859050584,-3.21585251789856));
#33094=CARTESIAN_POINT('Ctrl Pts',(370.608156672431,-3.86227338388473,-3.2148392780038));
#33095=CARTESIAN_POINT('Ctrl Pts',(370.579059110299,-3.86048357332093,-3.2126567795609));
#33096=CARTESIAN_POINT('Ctrl Pts',(370.564856993383,-3.85960659398358,-3.21149676066196));
#33097=CARTESIAN_POINT('Ctrl Pts',(370.531263101636,-3.85752392407555,-3.20852842949336));
#33098=CARTESIAN_POINT('Ctrl Pts',(370.511879276313,-3.85631569651385,-3.2066384583778));
#33099=CARTESIAN_POINT('Ctrl Pts',(370.446932874968,-3.85224498910158,-3.19971119422618));
#33100=CARTESIAN_POINT('Ctrl Pts',(370.401462566226,-3.84935772663629,-3.19387770606642));
#33101=CARTESIAN_POINT('Ctrl Pts',(370.292765285308,-3.84236283082331,-3.17756893902443));
#33102=CARTESIAN_POINT('Ctrl Pts',(370.229698011863,-3.83822818160346,-3.16617395339352));
#33103=CARTESIAN_POINT('Ctrl Pts',(369.982775837391,-3.82174239440779,-3.1139137007705));
#33104=CARTESIAN_POINT('Ctrl Pts',(369.802325379488,-3.80900954444348,-3.05884948296285));
#33105=CARTESIAN_POINT('Ctrl Pts',(369.478699228753,-3.78540588260638,-2.9281817511395));
#33106=CARTESIAN_POINT('Ctrl Pts',(369.334358961332,-3.77457644246989,-2.85693603057764));
#33107=CARTESIAN_POINT('Ctrl Pts',(369.172764043659,-3.76252036520117,-2.76153580439345));
#33108=CARTESIAN_POINT('Ctrl Pts',(369.14977261488,-3.7608070608928,-2.74757138408088));
#33109=CARTESIAN_POINT('Ctrl Pts',(369.117428846552,-3.75840263417235,-2.72736794971393));
#33110=CARTESIAN_POINT('Ctrl Pts',(369.107930848259,-3.7576972765344,-2.72136578067754));
#33111=CARTESIAN_POINT('Ctrl Pts',(369.091791514999,-3.75650020344815,-2.71104818208775));
#33112=CARTESIAN_POINT('Ctrl Pts',(369.085134389634,-3.75600687491644,-2.70675774690817));
#33113=CARTESIAN_POINT('Ctrl Pts',(369.072364509496,-3.75506150243121,-2.6984609299233));
#33114=CARTESIAN_POINT('Ctrl Pts',(369.066249494605,-3.75460921029972,-2.69445824936202));
#33115=CARTESIAN_POINT('Ctrl Pts',(369.053182277428,-3.75364346645604,-2.68584125475485));
#33116=CARTESIAN_POINT('Ctrl Pts',(369.046234253935,-3.7531304318148,-2.68122066056447));
#33117=CARTESIAN_POINT('Ctrl Pts',(369.019388682129,-3.75114966551596,-2.66321697917447));
#33118=CARTESIAN_POINT('Ctrl Pts',(368.99962221371,-3.74969438922306,-2.64963857197487));
#33119=CARTESIAN_POINT('Ctrl Pts',(368.892919872959,-3.74184517466493,-2.5745736500928));
#33120=CARTESIAN_POINT('Ctrl Pts',(368.808912229926,-3.73568853385702,-2.50902214528503));
#33121=CARTESIAN_POINT('Ctrl Pts',(368.540094203558,-3.71550721996651,-2.2769444046196));
#33122=CARTESIAN_POINT('Ctrl Pts',(368.371328920377,-3.70195302775649,-2.09323389094672));
#33123=CARTESIAN_POINT('Ctrl Pts',(368.170026241403,-3.68217321679005,-1.81564081844182));
#33124=CARTESIAN_POINT('Ctrl Pts',(368.118071956698,-3.67664234250873,-1.73695342040547));
#33125=CARTESIAN_POINT('Ctrl Pts',(368.056097606065,-3.66939965566806,-1.63349461299386));
#33126=CARTESIAN_POINT('Ctrl Pts',(368.042830177055,-3.66780697896265,-1.61071688494918));
#33127=CARTESIAN_POINT('Ctrl Pts',(368.022116281324,-3.66525050605913,-1.57413020451759));
#33128=CARTESIAN_POINT('Ctrl Pts',(368.014488477137,-3.66429324674535,-1.56042489659651));
#33129=CARTESIAN_POINT('Ctrl Pts',(368.000913391225,-3.662560425152,-1.53560916766059));
#33130=CARTESIAN_POINT('Ctrl Pts',(367.994930619681,-3.6617861497307,-1.52451844590893));
#33131=CARTESIAN_POINT('Ctrl Pts',(367.980995440456,-3.65995733597459,-1.49831915047281));
#33132=CARTESIAN_POINT('Ctrl Pts',(367.973097807401,-3.65890088624625,-1.48318201826607));
#33133=CARTESIAN_POINT('Ctrl Pts',(367.950338710095,-3.65579669096998,-1.4387020914458));
#33134=CARTESIAN_POINT('Ctrl Pts',(367.935806080932,-3.65373754648814,-1.4091943737659));
#33135=CARTESIAN_POINT('Ctrl Pts',(367.903851192017,-3.64902821329003,-1.34172536976308));
#33136=CARTESIAN_POINT('Ctrl Pts',(367.886710442178,-3.64636889319304,-1.30363802979962));
#33137=CARTESIAN_POINT('Ctrl Pts',(367.83216280498,-3.63744234058219,-1.17585148246727));
#33138=CARTESIAN_POINT('Ctrl Pts',(367.798075726298,-3.63107312681071,-1.0848007015654));
#33139=CARTESIAN_POINT('Ctrl Pts',(367.710264086302,-3.6121106062235,-0.813481981640369));
#33140=CARTESIAN_POINT('Ctrl Pts',(367.668137518932,-3.59927912810973,-0.629889307343783));
#33141=CARTESIAN_POINT('Ctrl Pts',(367.626128087694,-3.57878885385889,-0.327657132336179));
#33142=CARTESIAN_POINT('Ctrl Pts',(367.616336929242,-3.57102517716654,-0.210820564885843));
#33143=CARTESIAN_POINT('Ctrl Pts',(367.612365008877,-3.56231404483283,-0.0742658328475275));
#33144=CARTESIAN_POINT('Ctrl Pts',(367.61197560134,-3.56108262042694,-0.0548270000785654));
#33145=CARTESIAN_POINT('Ctrl Pts',(367.611671746325,-3.5593430140859,-0.0271547736545808));
#33146=CARTESIAN_POINT('Ctrl Pts',(367.611612901793,-3.5588272649062,-0.0189238359192423));
#33147=CARTESIAN_POINT('Ctrl Pts',(367.611573923759,-3.55809363972904,-0.00717598306127299));
#33148=CARTESIAN_POINT('Ctrl Pts',(367.611568011904,-3.55787434821804,-0.00365926833753844));
#33149=CARTESIAN_POINT('Ctrl Pts',(367.611567856376,-3.55765537866733,-0.00014252679442044));
#33150=CARTESIAN_POINT('Ctrl Pts',(367.611567856366,-3.55765536469338,-0.00014230236719019));
#33151=CARTESIAN_POINT('Ctrl Pts',(367.611567829866,-3.55761799647536,0.000457846706114776));
#33152=CARTESIAN_POINT('Ctrl Pts',(367.611567971008,-3.55758063764161,0.00105799643576072));
#33153=CARTESIAN_POINT('Ctrl Pts',(367.61157075936,-3.55724336969791,0.00647739667062727));
#33154=CARTESIAN_POINT('Ctrl Pts',(367.61158404864,-3.55694406733888,0.0112965967864436));
#33155=CARTESIAN_POINT('Ctrl Pts',(367.611652082637,-3.55610084187474,0.024901450644145));
#33156=CARTESIAN_POINT('Ctrl Pts',(367.611731943653,-3.55555833350072,0.0336869542414703));
#33157=CARTESIAN_POINT('Ctrl Pts',(367.612046172872,-3.55409132298816,0.0575283286255893));
#33158=CARTESIAN_POINT('Ctrl Pts',(367.61235013472,-3.5531705924886,0.0725832746862368));
#33159=CARTESIAN_POINT('Ctrl Pts',(367.614346293638,-3.54870787142136,0.145963525277752));
#33160=CARTESIAN_POINT('Ctrl Pts',(367.617516869005,-3.54524079870716,0.204241448695378));
#33161=CARTESIAN_POINT('Ctrl Pts',(367.625786436883,-3.53930385541055,0.305467638002747));
#33162=CARTESIAN_POINT('Ctrl Pts',(367.630170149061,-3.53680942521572,0.348456714715536));
#33163=CARTESIAN_POINT('Ctrl Pts',(367.660584617158,-3.52247539848918,0.597067511163521));
#33164=CARTESIAN_POINT('Ctrl Pts',(367.70553853136,-3.51111512367214,0.799887186822757));
#33165=CARTESIAN_POINT('Ctrl Pts',(367.800494870066,-3.49374226226303,1.09177377903907));
#33166=CARTESIAN_POINT('Ctrl Pts',(367.835707505049,-3.48803061199899,1.18506778974916));
#33167=CARTESIAN_POINT('Ctrl Pts',(367.892009772254,-3.47970109678367,1.31557781088509));
#33168=CARTESIAN_POINT('Ctrl Pts',(367.909604168867,-3.47718971066936,1.35424201974225));
#33169=CARTESIAN_POINT('Ctrl Pts',(367.942360117787,-3.47266274249192,1.42260644571472));
#33170=CARTESIAN_POINT('Ctrl Pts',(367.957228287441,-3.47065707821311,1.45244075559862));
#33171=CARTESIAN_POINT('Ctrl Pts',(367.98044907226,-3.46759429225963,1.49727924227374));
#33172=CARTESIAN_POINT('Ctrl Pts',(367.988463516651,-3.46654902539147,1.5124566855182));
#33173=CARTESIAN_POINT('Ctrl Pts',(368.003211429787,-3.46464633343383,1.53985343893699));
#33174=CARTESIAN_POINT('Ctrl Pts',(368.009903777199,-3.46379038421298,1.55209449187227));
#33175=CARTESIAN_POINT('Ctrl Pts',(368.024484543626,-3.46194119084425,1.57835774671204));
#33176=CARTESIAN_POINT('Ctrl Pts',(368.03239888159,-3.46094703421216,1.59236505416481));
#33177=CARTESIAN_POINT('Ctrl Pts',(368.054115324162,-3.45824440146888,1.63013701956501));
#33178=CARTESIAN_POINT('Ctrl Pts',(368.0681168208,-3.45652876402522,1.65378492501516));
#33179=CARTESIAN_POINT('Ctrl Pts',(368.141916134403,-3.44761936118916,1.7748689807496));
#33180=CARTESIAN_POINT('Ctrl Pts',(368.206559006927,-3.44024910185309,1.86924189523738));
#33181=CARTESIAN_POINT('Ctrl Pts',(368.416262833981,-3.41755386877325,2.14295681260095));
#33182=CARTESIAN_POINT('Ctrl Pts',(368.575676492069,-3.40177312332332,2.31036272296844));
#33183=CARTESIAN_POINT('Ctrl Pts',(368.829767106105,-3.37946119270624,2.52554911837101));
#33184=CARTESIAN_POINT('Ctrl Pts',(368.911102326798,-3.37268277922018,2.58802396646093));
#33185=CARTESIAN_POINT('Ctrl Pts',(369.01460666062,-3.364615032296,2.6599478160917));
#33186=CARTESIAN_POINT('Ctrl Pts',(369.034076362535,-3.36312064213182,2.67316326830018));
#33187=CARTESIAN_POINT('Ctrl Pts',(369.06060672089,-3.3611173396641,2.6907499420766));
#33188=CARTESIAN_POINT('Ctrl Pts',(369.067541510324,-3.36059670975951,2.69530847761069));
#33189=CARTESIAN_POINT('Ctrl Pts',(369.080617009859,-3.35962083802367,2.70383141787077));
#33190=CARTESIAN_POINT('Ctrl Pts',(369.086753732208,-3.35916520699288,2.70780180769196));
#33191=CARTESIAN_POINT('Ctrl Pts',(369.09943459671,-3.35822866912669,2.71594511828762));
#33192=CARTESIAN_POINT('Ctrl Pts',(369.105980385522,-3.3577479546418,2.72011532822708));
#33193=CARTESIAN_POINT('Ctrl Pts',(369.122043307154,-3.35657479965343,2.730267348895));
#33194=CARTESIAN_POINT('Ctrl Pts',(369.131576903321,-3.35588405656928,2.73622316045245));
#33195=CARTESIAN_POINT('Ctrl Pts',(369.164054935429,-3.35354897406428,2.75627729733774));
#33196=CARTESIAN_POINT('Ctrl Pts',(369.187145527261,-3.35191925768542,2.77013829806946));
#33197=CARTESIAN_POINT('Ctrl Pts',(369.354447708721,-3.34030827535417,2.86773603079442));
#33198=CARTESIAN_POINT('Ctrl Pts',(369.50481053641,-3.33090809950149,2.94046754668799));
#33199=CARTESIAN_POINT('Ctrl Pts',(369.806155769874,-3.31278502378425,3.0583627921969));
#33200=CARTESIAN_POINT('Ctrl Pts',(369.956139636517,-3.30407663110238,3.10475460573256));
#33201=CARTESIAN_POINT('Ctrl Pts',(370.225097507132,-3.28829901733509,3.16688980919041));
#33202=CARTESIAN_POINT('Ctrl Pts',(370.342686052497,-3.28135139917287,3.18726122239711));
#33203=CARTESIAN_POINT('Ctrl Pts',(370.488029244925,-3.27256924428055,3.20420590125974));
#33204=CARTESIAN_POINT('Ctrl Pts',(370.514971660014,-3.27093340694136,3.20700314917601));
#33205=CARTESIAN_POINT('Ctrl Pts',(370.557723914031,-3.26832385039949,3.2108977527887));
#33206=CARTESIAN_POINT('Ctrl Pts',(370.573512462089,-3.2673571582495,3.2122187223159));
#33207=CARTESIAN_POINT('Ctrl Pts',(370.603246645412,-3.26553074901222,3.21448580984111));
#33208=CARTESIAN_POINT('Ctrl Pts',(370.617189986974,-3.26467186312405,3.21545772864211));
#33209=CARTESIAN_POINT('Ctrl Pts',(370.648612609444,-3.26273063926348,3.21744272195414));
#33210=CARTESIAN_POINT('Ctrl Pts',(370.666094602899,-3.26164670724076,3.21840411155972));
#33211=CARTESIAN_POINT('Ctrl Pts',(370.710936715245,-3.25885594024044,3.22050376610953));
#33212=CARTESIAN_POINT('Ctrl Pts',(370.738304647765,-3.25714272815167,3.22143582937388));
#33213=CARTESIAN_POINT('Ctrl Pts',(370.978412778047,-3.24202146271751,3.22655075669993));
#33214=CARTESIAN_POINT('Ctrl Pts',(371.191032416868,-3.22795410939271,3.21000280670159));
#33215=CARTESIAN_POINT('Ctrl Pts',(371.613777981251,-3.19899209760355,3.13456915176621));
#33216=CARTESIAN_POINT('Ctrl Pts',(371.822747055675,-3.18416695670709,3.07507728358897));
#33217=CARTESIAN_POINT('Ctrl Pts',(372.054998044556,-3.16803520284136,2.98281036824715));
#33218=CARTESIAN_POINT('Ctrl Pts',(372.085635200027,-3.16591543623544,2.97008803244851));
#33219=CARTESIAN_POINT('Ctrl Pts',(372.127136193383,-3.16306057174462,2.95209819037317));
#33220=CARTESIAN_POINT('Ctrl Pts',(372.138173767819,-3.16230291152344,2.94723985299111));
#33221=CARTESIAN_POINT('Ctrl Pts',(372.15663233412,-3.16103888397526,2.9389910739153));
#33222=CARTESIAN_POINT('Ctrl Pts',(372.164068111902,-3.16053051946372,2.93563423692895));
#33223=CARTESIAN_POINT('Ctrl Pts',(372.178170663718,-3.15956805875611,2.92920314755624));
#33224=CARTESIAN_POINT('Ctrl Pts',(372.184839787428,-3.15911362747474,2.92613430377092));
#33225=CARTESIAN_POINT('Ctrl Pts',(372.200640510535,-3.15803854488296,2.9187979637927));
#33226=CARTESIAN_POINT('Ctrl Pts',(372.209762753533,-3.15741911740308,2.91451033448505));
#33227=CARTESIAN_POINT('Ctrl Pts',(372.241804253353,-3.15524729819495,2.89926627247825));
#33228=CARTESIAN_POINT('Ctrl Pts',(372.264614605347,-3.15370822051652,2.88808140070798));
#33229=CARTESIAN_POINT('Ctrl Pts',(372.294816617636,-3.1516767028354,2.87282648332488));
#33230=CARTESIAN_POINT('Ctrl Pts',(372.302326508682,-3.15117207890497,2.86899620186515));
#33231=CARTESIAN_POINT('Ctrl Pts',(372.309820619203,-3.15066895420511,2.86513684665975));
#33232=CARTESIAN_POINT('Ctrl Pts',(372.309820062099,-2.9049971700688,2.86513713356014));
#33233=CARTESIAN_POINT('Ctrl Pts',(372.212990497692,-2.9121440670608,2.91500289198845));
#33234=CARTESIAN_POINT('Ctrl Pts',(372.113646582387,-2.91942904114421,2.95995312199687));
#33235=CARTESIAN_POINT('Ctrl Pts',(371.807974008103,-2.9415687748639,3.07997266155052));
#33236=CARTESIAN_POINT('Ctrl Pts',(371.596125083592,-2.95658437889865,3.13909193096567));
#33237=CARTESIAN_POINT('Ctrl Pts',(371.347045112705,-2.97290044565745,3.18187678968539));
#33238=CARTESIAN_POINT('Ctrl Pts',(371.314098772515,-2.97503131292557,3.18701107940408));
#33239=CARTESIAN_POINT('Ctrl Pts',(371.269105515018,-2.97789890008957,3.19330915849462));
#33240=CARTESIAN_POINT('Ctrl Pts',(371.257124246555,-2.97865842483268,3.19491759787925));
#33241=CARTESIAN_POINT('Ctrl Pts',(371.23703213408,-2.979924954863,3.1974998819085));
#33242=CARTESIAN_POINT('Ctrl Pts',(371.228926214098,-2.98043397059477,3.19851036153577));
#33243=CARTESIAN_POINT('Ctrl Pts',(371.213526068135,-2.98139721724477,3.20037069989908));
#33244=CARTESIAN_POINT('Ctrl Pts',(371.206232661043,-2.98185178672203,3.20122646267032));
#33245=CARTESIAN_POINT('Ctrl Pts',(371.18892736776,-2.98292665733528,3.20319701743692));
#33246=CARTESIAN_POINT('Ctrl Pts',(371.178912985396,-2.983545738333,3.20428981858283));
#33247=CARTESIAN_POINT('Ctrl Pts',(371.143687146139,-2.98571357513805,3.20796672135347));
#33248=CARTESIAN_POINT('Ctrl Pts',(371.118449754988,-2.98724908709812,3.21030045283448));
#33249=CARTESIAN_POINT('Ctrl Pts',(370.876717096777,-3.00181066886283,3.22978067537564));
#33250=CARTESIAN_POINT('Ctrl Pts',(370.659007524435,-3.01383060881662,3.22530206277619));
#33251=CARTESIAN_POINT('Ctrl Pts',(370.294203025646,-3.03438817927249,3.18071999993724));
#33252=CARTESIAN_POINT('Ctrl Pts',(370.146491447725,-3.04282735445192,3.15207773805954));
#33253=CARTESIAN_POINT('Ctrl Pts',(369.948060920604,-3.05474533432585,3.09898475081882));
#33254=CARTESIAN_POINT('Ctrl Pts',(369.895172777709,-3.05797876640334,3.08336891676003));
#33255=CARTESIAN_POINT('Ctrl Pts',(369.803829858491,-3.0636810643626,3.05383072187969));
#33256=CARTESIAN_POINT('Ctrl Pts',(369.765190559135,-3.06613064613561,3.04051873664162));
#33257=CARTESIAN_POINT('Ctrl Pts',(369.709331707476,-3.06973140073274,3.02007787563735));
#33258=CARTESIAN_POINT('Ctrl Pts',(369.691903390251,-3.07086339430153,3.01352839297769));
#33259=CARTESIAN_POINT('Ctrl Pts',(369.661359169208,-3.07286277121287,3.00174696812662));
#33260=CARTESIAN_POINT('Ctrl Pts',(369.648218964491,-3.07372799056319,2.99657910811594));
#33261=CARTESIAN_POINT('Ctrl Pts',(369.622675797214,-3.0754199956706,2.98633900348051));
#33262=CARTESIAN_POINT('Ctrl Pts',(369.610269657893,-3.07624647497355,2.98127541875283));
#33263=CARTESIAN_POINT('Ctrl Pts',(369.576968726971,-3.0784777571452,2.96744069136204));
#33264=CARTESIAN_POINT('Ctrl Pts',(369.556134572482,-3.07988738685624,2.95852641373332));
#33265=CARTESIAN_POINT('Ctrl Pts',(369.4781407185,-3.08521703500485,2.92417769704913));
#33266=CARTESIAN_POINT('Ctrl Pts',(369.421634725397,-3.08918582422223,2.89730169846489));
#33267=CARTESIAN_POINT('Ctrl Pts',(369.065112621371,-3.11493823966977,2.71481920817199));
#33268=CARTESIAN_POINT('Ctrl Pts',(368.790448867474,-3.13837725266613,2.51452731906935));
#33269=CARTESIAN_POINT('Ctrl Pts',(368.51881711562,-3.16377513663097,2.24204700986508));
#33270=CARTESIAN_POINT('Ctrl Pts',(368.486423571826,-3.16684151399197,2.20810129998184));
#33271=CARTESIAN_POINT('Ctrl Pts',(368.433876482635,-3.17186224090437,2.15057192472469));
#33272=CARTESIAN_POINT('Ctrl Pts',(368.413302120969,-3.17384058586332,2.12738369046839));
#33273=CARTESIAN_POINT('Ctrl Pts',(368.385392955192,-3.17653741522548,2.09499940434961));
#33274=CARTESIAN_POINT('Ctrl Pts',(368.377769849716,-3.17727542397237,2.08605550667594));
#33275=CARTESIAN_POINT('Ctrl Pts',(368.364974898184,-3.17851620822447,2.07087627618417));
#33276=CARTESIAN_POINT('Ctrl Pts',(368.359777372325,-3.17902082307195,2.06466282824706));
#33277=CARTESIAN_POINT('Ctrl Pts',(368.349870873617,-3.17998364447989,2.05272883334959));
#33278=CARTESIAN_POINT('Ctrl Pts',(368.345158141807,-3.18044213686891,2.04701157578841));
#33279=CARTESIAN_POINT('Ctrl Pts',(368.333922761546,-3.18153644559037,2.03328518321275));
#33280=CARTESIAN_POINT('Ctrl Pts',(368.32741877071,-3.1821709356715,2.02526078508258));
#33281=CARTESIAN_POINT('Ctrl Pts',(368.304089310004,-3.18445106059485,1.99619312254939));
#33282=CARTESIAN_POINT('Ctrl Pts',(368.287488780277,-3.18608157755797,1.97496968185856));
#33283=CARTESIAN_POINT('Ctrl Pts',(368.169292390578,-3.19777043982276,1.81988888447335));
#33284=CARTESIAN_POINT('Ctrl Pts',(368.078025428772,-3.20723851439143,1.67845825364984));
#33285=CARTESIAN_POINT('Ctrl Pts',(367.928125676097,-3.22491379972707,1.40069099692061));
#33286=CARTESIAN_POINT('Ctrl Pts',(367.867053271532,-3.23311396081248,1.26618618897768));
#33287=CARTESIAN_POINT('Ctrl Pts',(367.771169655093,-3.24873262785019,1.00956395124081));
#33288=CARTESIAN_POINT('Ctrl Pts',(367.733936138239,-3.25607965892257,0.888664263684783));
#33289=CARTESIAN_POINT('Ctrl Pts',(367.697359130642,-3.26531336639497,0.739165096227663));
#33290=CARTESIAN_POINT('Ctrl Pts',(367.691161129629,-3.26697507139554,0.712348795432458));
#33291=CARTESIAN_POINT('Ctrl Pts',(367.681915896509,-3.26961688578751,0.669875913463045));
#33292=CARTESIAN_POINT('Ctrl Pts',(367.678640036096,-3.27058967052463,0.654270079049063));
#33293=CARTESIAN_POINT('Ctrl Pts',(367.672710501913,-3.27242206845296,0.624941485819358));
#33294=CARTESIAN_POINT('Ctrl Pts',(367.670030014276,-3.2732808027859,0.611224481747655));
#33295=CARTESIAN_POINT('Ctrl Pts',(367.664215093501,-3.27521434445588,0.580403663803702));
#33296=CARTESIAN_POINT('Ctrl Pts',(367.6611297111,-3.27629068538196,0.563291146628433));
#33297=CARTESIAN_POINT('Ctrl Pts',(367.653613197444,-3.27904752273958,0.519579249319347));
#33298=CARTESIAN_POINT('Ctrl Pts',(367.649377225552,-3.28073412997337,0.492948101564355));
#33299=CARTESIAN_POINT('Ctrl Pts',(367.622762044809,-3.2923124245762,0.310924716107186));
#33300=CARTESIAN_POINT('Ctrl Pts',(367.611432623364,-3.30254997493467,0.154152664312409));
#33301=CARTESIAN_POINT('Ctrl Pts',(367.611779203676,-3.32915016553059,-0.244515246666114));
#33302=CARTESIAN_POINT('Ctrl Pts',(367.639180874197,-3.34579243102028,-0.485426413940841));
#33303=CARTESIAN_POINT('Ctrl Pts',(367.706259561983,-3.36547561738465,-0.777654906549834));
#33304=CARTESIAN_POINT('Ctrl Pts',(367.72079412074,-3.36923911200978,-0.833946492865908));
#33305=CARTESIAN_POINT('Ctrl Pts',(367.741085105635,-3.37390019904172,-0.90457980847519));
#33306=CARTESIAN_POINT('Ctrl Pts',(367.745431371501,-3.37486893053905,-0.919311582398069));
#33307=CARTESIAN_POINT('Ctrl Pts',(367.752457942647,-3.376388769133,-0.942515781451098));
#33308=CARTESIAN_POINT('Ctrl Pts',(367.755068187148,-3.37694377818999,-0.951008940629364));
#33309=CARTESIAN_POINT('Ctrl Pts',(367.760066683813,-3.37798858435168,-0.967036596165972));
#33310=CARTESIAN_POINT('Ctrl Pts',(367.762447505092,-3.3784787736131,-0.97457303286626));
#33311=CARTESIAN_POINT('Ctrl Pts',(367.768084933984,-3.37962232265652,-0.992192274379373));
#33312=CARTESIAN_POINT('Ctrl Pts',(367.771363566489,-3.3802743905606,-1.00226786295412));
#33313=CARTESIAN_POINT('Ctrl Pts',(367.782197697417,-3.38238800377416,-1.03501259831202));
#33314=CARTESIAN_POINT('Ctrl Pts',(367.789955829606,-3.38383823618245,-1.05761451862846));
#33315=CARTESIAN_POINT('Ctrl Pts',(367.83337690453,-3.39163356579976,-1.17967561754491));
#33316=CARTESIAN_POINT('Ctrl Pts',(367.873666605061,-3.39774498281753,-1.27743090109817));
#33317=CARTESIAN_POINT('Ctrl Pts',(368.022759711864,-3.41763768935576,-1.59402795990486));
#33318=CARTESIAN_POINT('Ctrl Pts',(368.151613355638,-3.43095997806631,-1.80246656955757));
#33319=CARTESIAN_POINT('Ctrl Pts',(368.363998610368,-3.4507187537325,-2.07205847557383));
#33320=CARTESIAN_POINT('Ctrl Pts',(368.428756474573,-3.45651493851356,-2.14689896862242));
#33321=CARTESIAN_POINT('Ctrl Pts',(368.515228055924,-3.46405605097678,-2.2380019670637));
#33322=CARTESIAN_POINT('Ctrl Pts',(368.533846541543,-3.46566875661021,-2.25713578934491));
#33323=CARTESIAN_POINT('Ctrl Pts',(368.563834822089,-3.46825031338518,-2.28719761658069));
#33324=CARTESIAN_POINT('Ctrl Pts',(368.575051066068,-3.46921240536457,-2.29827755125347));
#33325=CARTESIAN_POINT('Ctrl Pts',(368.595376984848,-3.47094995899639,-2.3180638741087));
#33326=CARTESIAN_POINT('Ctrl Pts',(368.604457331219,-3.47172409630808,-2.32680003046726));
#33327=CARTESIAN_POINT('Ctrl Pts',(368.625898177617,-3.47354727828909,-2.34718738640369));
#33328=CARTESIAN_POINT('Ctrl Pts',(368.638299932047,-3.47459819147874,-2.35879447232996));
#33329=CARTESIAN_POINT('Ctrl Pts',(368.674643196603,-3.47766773458439,-2.39227392190985));
#33330=CARTESIAN_POINT('Ctrl Pts',(368.698823241024,-3.47969737047273,-2.41388313258036));
#33331=CARTESIAN_POINT('Ctrl Pts',(368.883444555114,-3.49510530886284,-2.57393021356425));
#33332=CARTESIAN_POINT('Ctrl Pts',(369.056836071296,-3.50913069089222,-2.69658166691028));
#33333=CARTESIAN_POINT('Ctrl Pts',(369.436485797651,-3.53859704341476,-2.91252017197192));
#33334=CARTESIAN_POINT('Ctrl Pts',(369.643112447912,-3.55398798522191,-3.00295713774306));
#33335=CARTESIAN_POINT('Ctrl Pts',(369.881074744475,-3.56999902556909,-3.0786454756534));
#33336=CARTESIAN_POINT('Ctrl Pts',(369.90475202913,-3.5715735346865,-3.0858771612309));
#33337=CARTESIAN_POINT('Ctrl Pts',(369.938082484053,-3.57376170804045,-3.09563873774642));
#33338=CARTESIAN_POINT('Ctrl Pts',(369.947666967893,-3.57438767929088,-3.09839752860961));
#33339=CARTESIAN_POINT('Ctrl Pts',(369.964306346375,-3.57546858327716,-3.10310346237015));
#33340=CARTESIAN_POINT('Ctrl Pts',(369.971355288168,-3.57592467907679,-3.10507113188542));
#33341=CARTESIAN_POINT('Ctrl Pts',(369.986315308536,-3.57688873431455,-3.10919225311614));
#33342=CARTESIAN_POINT('Ctrl Pts',(369.994228027728,-3.57739632476171,-3.11133956209253));
#33343=CARTESIAN_POINT('Ctrl Pts',(370.013967964446,-3.57865703174619,-3.11661567907993));
#33344=CARTESIAN_POINT('Ctrl Pts',(370.025805099449,-3.57940803680223,-3.11970741724982));
#33345=CARTESIAN_POINT('Ctrl Pts',(370.070989022946,-3.58225676144758,-3.13123454825162));
#33346=CARTESIAN_POINT('Ctrl Pts',(370.104453800288,-3.58432943358858,-3.13920362199423));
#33347=CARTESIAN_POINT('Ctrl Pts',(370.190849493394,-3.58960014192736,-3.15832096003903));
#33348=CARTESIAN_POINT('Ctrl Pts',(370.243946429728,-3.5927625748746,-3.16867559553745));
#33349=CARTESIAN_POINT('Ctrl Pts',(370.457813844205,-3.60528317841956,-3.20481964511786));
#33350=CARTESIAN_POINT('Ctrl Pts',(370.620180687067,-3.61430985243349,-3.21974779953513));
#33351=CARTESIAN_POINT('Ctrl Pts',(370.993741959887,-3.63522415055653,-3.22569835500643));
#33352=CARTESIAN_POINT('Ctrl Pts',(371.204287589343,-3.64714496323274,-3.20837224024529));
#33353=CARTESIAN_POINT('Ctrl Pts',(371.438607084134,-3.66139951906262,-3.16570757580315));
#33354=CARTESIAN_POINT('Ctrl Pts',(371.465528244942,-3.66305148646487,-3.16044985747343));
#33355=CARTESIAN_POINT('Ctrl Pts',(371.509538178868,-3.66577698185465,-3.15126995727593));
#33356=CARTESIAN_POINT('Ctrl Pts',(371.526668194596,-3.66684404759612,-3.14755076491498));
#33357=CARTESIAN_POINT('Ctrl Pts',(371.557411967435,-3.6687707054668,-3.14061270116702));
#33358=CARTESIAN_POINT('Ctrl Pts',(371.571036809727,-3.6696286523253,-3.13744456622157));
#33359=CARTESIAN_POINT('Ctrl Pts',(371.60005559418,-3.67146489637807,-3.13049748775872));
#33360=CARTESIAN_POINT('Ctrl Pts',(371.615443100201,-3.67244398056333,-3.12669348401505));
#33361=CARTESIAN_POINT('Ctrl Pts',(371.657046692551,-3.67510609735314,-3.11608222419833));
#33362=CARTESIAN_POINT('Ctrl Pts',(371.683205583709,-3.67679609056244,-3.10905785087844));
#33363=CARTESIAN_POINT('Ctrl Pts',(371.823827128,-3.68597053619749,-3.06939017089466));
#33364=CARTESIAN_POINT('Ctrl Pts',(371.936490663738,-3.6936479276592,-3.03075798727444));
#33365=CARTESIAN_POINT('Ctrl Pts',(372.191391209001,-3.7117757586918,-2.92725809461126));
#33366=CARTESIAN_POINT('Ctrl Pts',(372.331564547322,-3.7223267048198,-2.85809963701444));
#33367=CARTESIAN_POINT('Ctrl Pts',(372.610762336887,-3.74422881938056,-2.69415673114183));
#33368=CARTESIAN_POINT('Ctrl Pts',(372.748527627384,-3.75554801241723,-2.59808526955013));
#33369=CARTESIAN_POINT('Ctrl Pts',(372.899032600674,-3.76805463356073,-2.47463060025924));
#33370=CARTESIAN_POINT('Ctrl Pts',(372.919651222622,-3.76977097162885,-2.45728070124938));
#33371=CARTESIAN_POINT('Ctrl Pts',(372.947870054799,-3.77212125364152,-2.4329244437565));
#33372=CARTESIAN_POINT('Ctrl Pts',(372.955657165518,-3.77276996167892,-2.42613762733044));
#33373=CARTESIAN_POINT('Ctrl Pts',(372.968973728147,-3.77387933443189,-2.41441851276293));
#33374=CARTESIAN_POINT('Ctrl Pts',(372.974518991729,-3.7743413073408,-2.40950441968526));
#33375=CARTESIAN_POINT('Ctrl Pts',(372.986091333157,-3.77530531981232,-2.39917779089605));
#33376=CARTESIAN_POINT('Ctrl Pts',(372.992115018516,-3.77580705990702,-2.39376159558856));
#33377=CARTESIAN_POINT('Ctrl Pts',(373.006826800607,-3.7770325234044,-2.38043284392909));
#33378=CARTESIAN_POINT('Ctrl Pts',(373.015492272111,-3.77775438793283,-2.37249527191035));
#33379=CARTESIAN_POINT('Ctrl Pts',(373.04685457927,-3.78036800144486,-2.34345032872171));
#33380=CARTESIAN_POINT('Ctrl Pts',(373.069290834093,-3.78223971845508,-2.32206247619523));
#33381=CARTESIAN_POINT('Ctrl Pts',(373.124898309436,-3.78689445588478,-2.26750062999015));
#33382=CARTESIAN_POINT('Ctrl Pts',(373.157661076496,-3.78965150877388,-2.23391912022644));
#33383=CARTESIAN_POINT('Ctrl Pts',(373.420178234749,-3.81198467921825,-1.95281622241874));
#33384=CARTESIAN_POINT('Ctrl Pts',(373.610458269654,-3.82996805825992,-1.67130180618511));
#33385=CARTESIAN_POINT('Ctrl Pts',(373.780113394984,-3.8534287674637,-1.30856238574083));
#33386=CARTESIAN_POINT('Ctrl Pts',(373.805006399867,-3.85714928361983,-1.25102185254051));
#33387=CARTESIAN_POINT('Ctrl Pts',(373.836598209323,-3.86229303504222,-1.17172715313238));
#33388=CARTESIAN_POINT('Ctrl Pts',(373.844768976411,-3.86366688147504,-1.15057196758881));
#33389=CARTESIAN_POINT('Ctrl Pts',(373.857412394046,-3.86586458791856,-1.11677956681121));
#33390=CARTESIAN_POINT('Ctrl Pts',(373.862030738563,-3.86668357060054,-1.10419739133355));
#33391=CARTESIAN_POINT('Ctrl Pts',(373.871352498341,-3.86837064607648,-1.07830304487691));
#33392=CARTESIAN_POINT('Ctrl Pts',(373.876047182889,-3.86923900727129,-1.0649880596574));
#33393=CARTESIAN_POINT('Ctrl Pts',(373.886726272867,-3.87125864715333,-1.03405350763706));
#33394=CARTESIAN_POINT('Ctrl Pts',(373.892645821064,-3.87241203792564,-1.0164122366533));
#33395=CARTESIAN_POINT('Ctrl Pts',(373.911058673749,-3.87611115906772,-0.959921266544794));
#33396=CARTESIAN_POINT('Ctrl Pts',(373.922966585009,-3.87867589013796,-0.920886356140307));
#33397=CARTESIAN_POINT('Ctrl Pts',(373.949186490513,-3.88475572296247,-0.828697904603664));
#33398=CARTESIAN_POINT('Ctrl Pts',(373.9628839076,-3.88828937970205,-0.775384235249085));
#33399=CARTESIAN_POINT('Ctrl Pts',(374.008765095857,-3.90158860469663,-0.575719352182483));
#33400=CARTESIAN_POINT('Ctrl Pts',(374.0320931526,-3.9115989174222,-0.427542673436495));
#33401=CARTESIAN_POINT('Ctrl Pts',(374.063845229113,-3.9364230442883,-0.0612172094050287));
#33402=CARTESIAN_POINT('Ctrl Pts',(374.060598827227,-3.95130997040103,0.15722391718154));
#33403=CARTESIAN_POINT('Ctrl Pts',(374.032396816226,-3.9669133748851,0.398809107101842));
#33404=CARTESIAN_POINT('Ctrl Pts',(374.029167073468,-3.96852327796972,0.423906014817121));
#33405=CARTESIAN_POINT('Ctrl Pts',(374.024239582691,-3.97075220844494,0.458931650489408));
#33406=CARTESIAN_POINT('Ctrl Pts',(374.022790470839,-3.97138413487997,0.468893669184143));
#33407=CARTESIAN_POINT('Ctrl Pts',(374.020203842003,-3.97247246227818,0.486108966869099));
#33408=CARTESIAN_POINT('Ctrl Pts',(374.019088184484,-3.97293006401439,0.493365382703262));
#33409=CARTESIAN_POINT('Ctrl Pts',(374.01667852328,-3.97389392191113,0.508689380776045));
#33410=CARTESIAN_POINT('Ctrl Pts',(374.015378617927,-3.97439982786514,0.516755971664285));
#33411=CARTESIAN_POINT('Ctrl Pts',(374.012077868809,-3.97565058972185,0.536754331800457));
#33412=CARTESIAN_POINT('Ctrl Pts',(374.010040464796,-3.97639340598691,0.548680083936111));
#33413=CARTESIAN_POINT('Ctrl Pts',(374.002124123033,-3.97917427346625,0.593495818295456));
#33414=CARTESIAN_POINT('Ctrl Pts',(373.995800777476,-3.9811887861083,0.626306449499276));
#33415=CARTESIAN_POINT('Ctrl Pts',(373.943875778393,-3.99632733087697,0.874867399492619));
#33416=CARTESIAN_POINT('Ctrl Pts',(373.876742610989,-4.00848282831185,1.08555047116196));
#33417=CARTESIAN_POINT('Ctrl Pts',(373.705280189953,-4.03250861791472,1.47891205875771));
#33418=CARTESIAN_POINT('Ctrl Pts',(373.603607089236,-4.04431114045585,1.66151350072321));
#33419=CARTESIAN_POINT('Ctrl Pts',(373.469416803599,-4.05843153649002,1.85556554642088));
#33420=CARTESIAN_POINT('Ctrl Pts',(373.453528325431,-4.06008355264648,1.87792609219064));
#33421=CARTESIAN_POINT('Ctrl Pts',(373.427021695981,-4.06280911222559,1.91423917636079));
#33422=CARTESIAN_POINT('Ctrl Pts',(373.41657149612,-4.06387619287794,1.92831297911782));
#33423=CARTESIAN_POINT('Ctrl Pts',(373.397576580063,-4.06580286700543,1.95346306253045));
#33424=CARTESIAN_POINT('Ctrl Pts',(373.389073522046,-4.06666081509207,1.96457036022048));
#33425=CARTESIAN_POINT('Ctrl Pts',(373.370781741681,-4.06849705016439,1.98814480010711));
#33426=CARTESIAN_POINT('Ctrl Pts',(373.360972842844,-4.06947612405606,2.00059574945215));
#33427=CARTESIAN_POINT('Ctrl Pts',(373.334155308242,-4.07213818354391,2.03412483121249));
#33428=CARTESIAN_POINT('Ctrl Pts',(373.316972452335,-4.07382812923219,2.05506136162226));
#33429=CARTESIAN_POINT('Ctrl Pts',(373.222871453893,-4.08300176313569,2.16681643109897));
#33430=CARTESIAN_POINT('Ctrl Pts',(373.141239622164,-4.09067834932071,2.25352789169221));
#33431=CARTESIAN_POINT('Ctrl Pts',(372.941899247381,-4.10880314254793,2.44306743086542));
#33432=CARTESIAN_POINT('Ctrl Pts',(372.821134419252,-4.11935178358883,2.54224917994442));
#33433=CARTESIAN_POINT('Ctrl Pts',(372.571281966395,-4.14004479943622,2.71873611795599));
#33434=CARTESIAN_POINT('Ctrl Pts',(372.443019729746,-4.15015981842891,2.79654129191001));
#33435=CARTESIAN_POINT('Ctrl Pts',(372.309820591895,-4.15988901539235,2.86513686072284));
#33436=CARTESIAN_POINT('Origin',(370.834317853224,2.31077344927308,0.));
#33437=CARTESIAN_POINT('',(372.30982061461,-5.65649214416028,2.86513684902517));
#33438=CARTESIAN_POINT('',(372.309820461314,-5.4072724248197,2.86513692797037));
#33439=CARTESIAN_POINT('',(372.309820613641,2.31077344927308,2.86513684952399));
#33440=CARTESIAN_POINT('Ctrl Pts',(372.30982061461,-5.65649214416028,2.86513684902516));
#33441=CARTESIAN_POINT('Ctrl Pts',(372.324646905427,-5.65549151767139,2.85750153029707));
#33442=CARTESIAN_POINT('Ctrl Pts',(372.339413897489,-5.65448700712985,2.849751145584));
#33443=CARTESIAN_POINT('Ctrl Pts',(372.371287420897,-5.65230123425484,2.83270561624129));
#33444=CARTESIAN_POINT('Ctrl Pts',(372.388370738551,-5.65111860453467,2.82336964709382));
#33445=CARTESIAN_POINT('Ctrl Pts',(372.417808569281,-5.64906086813046,2.80693386502652));
#33446=CARTESIAN_POINT('Ctrl Pts',(372.430202641378,-5.64818834276088,2.79990576683099));
#33447=CARTESIAN_POINT('Ctrl Pts',(372.455490109454,-5.6463952677621,2.78534397623984));
#33448=CARTESIAN_POINT('Ctrl Pts',(372.46837854585,-5.64547444838736,2.77780240319494));
#33449=CARTESIAN_POINT('Ctrl Pts',(372.500903467046,-5.64313281882727,2.7584659965061));
#33450=CARTESIAN_POINT('Ctrl Pts',(372.520467218694,-5.64170765669649,2.7465510255415));
#33451=CARTESIAN_POINT('Ctrl Pts',(372.594539642962,-5.63624671857717,2.70034878146331));
#33452=CARTESIAN_POINT('Ctrl Pts',(372.648140259158,-5.632159007086,2.66464099260271));
#33453=CARTESIAN_POINT('Ctrl Pts',(372.974343310244,-5.6064060655082,2.43292589040928));
#33454=CARTESIAN_POINT('Ctrl Pts',(373.215920612553,-5.58312211048917,2.19698114644329));
#33455=CARTESIAN_POINT('Ctrl Pts',(373.444722237587,-5.55787786934681,1.89052877422227));
#33456=CARTESIAN_POINT('Ctrl Pts',(373.471915974453,-5.55481751501434,1.85240025159212));
#33457=CARTESIAN_POINT('Ctrl Pts',(373.515687780797,-5.54980585174876,1.78810813736598));
#33458=CARTESIAN_POINT('Ctrl Pts',(373.532736485199,-5.54783063961079,1.76227479427757));
#33459=CARTESIAN_POINT('Ctrl Pts',(373.555735366145,-5.54513766641326,1.72630880515592));
#33460=CARTESIAN_POINT('Ctrl Pts',(373.562005659106,-5.54440044224962,1.71638416855106));
#33461=CARTESIAN_POINT('Ctrl Pts',(373.572507294621,-5.54316086084008,1.6995592530596));
#33462=CARTESIAN_POINT('Ctrl Pts',(373.576767091321,-5.54265666874517,1.69267694885435));
#33463=CARTESIAN_POINT('Ctrl Pts',(373.584873988485,-5.54169458086278,1.67946816877427));
#33464=CARTESIAN_POINT('Ctrl Pts',(373.588725262863,-5.54123640015409,1.67314440723975));
#33465=CARTESIAN_POINT('Ctrl Pts',(373.597893884134,-5.54014276182353,1.65797215025059));
#33466=CARTESIAN_POINT('Ctrl Pts',(373.603190615228,-5.53950862927065,1.64911120431293));
#33467=CARTESIAN_POINT('Ctrl Pts',(373.622153620668,-5.53722928122978,1.61703890362909));
#33468=CARTESIAN_POINT('Ctrl Pts',(373.635571772745,-5.53559917782147,1.59368116887163));
#33469=CARTESIAN_POINT('Ctrl Pts',(373.730812085376,-5.52388065936735,1.42297070013873));
#33470=CARTESIAN_POINT('Ctrl Pts',(373.801265837483,-5.51438616685968,1.26955030696506));
#33471=CARTESIAN_POINT('Ctrl Pts',(373.91303122637,-5.49623676717866,0.965314205608621));
#33472=CARTESIAN_POINT('Ctrl Pts',(373.956023607588,-5.48759516155223,0.815633857660002));
#33473=CARTESIAN_POINT('Ctrl Pts',(374.012495896879,-5.47191324494361,0.547187947629447));
#33474=CARTESIAN_POINT('Ctrl Pts',(374.03050277524,-5.46499155525484,0.429683314757538));
#33475=CARTESIAN_POINT('Ctrl Pts',(374.044597052922,-5.4562386729318,0.284529725317868));
#33476=CARTESIAN_POINT('Ctrl Pts',(374.046872732845,-5.45460453789132,0.257567044231749));
#33477=CARTESIAN_POINT('Ctrl Pts',(374.049941713462,-5.45199707482328,0.214782628524611));
#33478=CARTESIAN_POINT('Ctrl Pts',(374.050958367269,-5.45103075423221,0.198977831542825));
#33479=CARTESIAN_POINT('Ctrl Pts',(374.052652920555,-5.44920466006201,0.169210941900602));
#33480=CARTESIAN_POINT('Ctrl Pts',(374.053356557146,-5.44834571445371,0.155250640445523));
#33481=CARTESIAN_POINT('Ctrl Pts',(374.054737334368,-5.44640383512622,0.12378531742598));
#33482=CARTESIAN_POINT('Ctrl Pts',(374.05536260377,-5.44531930287454,0.10627857225238));
#33483=CARTESIAN_POINT('Ctrl Pts',(374.056600220576,-5.44252595655696,0.061363489917607));
#33484=CARTESIAN_POINT('Ctrl Pts',(374.057005608462,-5.44081074544034,0.0339512958255219));
#33485=CARTESIAN_POINT('Ctrl Pts',(374.057489157858,-5.42580277844255,-0.204404840944728));
#33486=CARTESIAN_POINT('Ctrl Pts',(374.03720586316,-5.41186293169812,-0.414841996855587));
#33487=CARTESIAN_POINT('Ctrl Pts',(373.965074170965,-5.38665259642414,-0.781699283207342));
#33488=CARTESIAN_POINT('Ctrl Pts',(373.921535743419,-5.37554454534307,-0.93902970781249));
#33489=CARTESIAN_POINT('Ctrl Pts',(373.839017853861,-5.35940211354028,-1.16806000342722));
#33490=CARTESIAN_POINT('Ctrl Pts',(373.808930079924,-5.35414993751283,-1.24268687981371));
#33491=CARTESIAN_POINT('Ctrl Pts',(373.769461387083,-5.34801344151446,-1.33090666728788));
#33492=CARTESIAN_POINT('Ctrl Pts',(373.762732468218,-5.34699056539046,-1.34564779551968));
#33493=CARTESIAN_POINT('Ctrl Pts',(373.752065852021,-5.34540559487515,-1.36855630626528));
#33494=CARTESIAN_POINT('Ctrl Pts',(373.748204496745,-5.34483903301053,-1.37675865036442));
#33495=CARTESIAN_POINT('Ctrl Pts',(373.740931212906,-5.34378533172292,-1.39204098473887));
#33496=CARTESIAN_POINT('Ctrl Pts',(373.737528022902,-5.34329769776267,-1.39912474001386));
#33497=CARTESIAN_POINT('Ctrl Pts',(373.729694571067,-5.34218741273633,-1.41527845638848));
#33498=CARTESIAN_POINT('Ctrl Pts',(373.725247585582,-5.34156580450749,-1.42434010556204));
#33499=CARTESIAN_POINT('Ctrl Pts',(373.713297930534,-5.33991797806365,-1.44840346899508));
#33500=CARTESIAN_POINT('Ctrl Pts',(373.7057204856,-5.33889620727996,-1.46336797989245));
#33501=CARTESIAN_POINT('Ctrl Pts',(373.639414499747,-5.33014576237488,-1.5918158479939));
#33502=CARTESIAN_POINT('Ctrl Pts',(373.574094472916,-5.32278681951285,-1.70178630154783));
#33503=CARTESIAN_POINT('Ctrl Pts',(373.396857078838,-5.30490381028631,-1.96339615710775));
#33504=CARTESIAN_POINT('Ctrl Pts',(373.277862871147,-5.29454528626369,-2.10964958834086));
#33505=CARTESIAN_POINT('Ctrl Pts',(373.050446434535,-5.2760017292912,-2.343933216325));
#33506=CARTESIAN_POINT('Ctrl Pts',(372.947829120339,-5.26799294342707,-2.43686525887041));
#33507=CARTESIAN_POINT('Ctrl Pts',(372.817542964072,-5.25801339699229,-2.54041872357883));
#33508=CARTESIAN_POINT('Ctrl Pts',(372.795290011404,-5.25631539458875,-2.55763508934913));
#33509=CARTESIAN_POINT('Ctrl Pts',(372.759976195503,-5.25362941032637,-2.58422440899075));
#33510=CARTESIAN_POINT('Ctrl Pts',(372.747065424199,-5.25264918796207,-2.59379501162311));
#33511=CARTESIAN_POINT('Ctrl Pts',(372.722813275474,-5.25081091728813,-2.61149330351116));
#33512=CARTESIAN_POINT('Ctrl Pts',(372.711489612163,-5.24995381594216,-2.61964471100201));
#33513=CARTESIAN_POINT('Ctrl Pts',(372.686100387786,-5.24803457993975,-2.63767215093226));
#33514=CARTESIAN_POINT('Ctrl Pts',(372.672008117829,-5.2469710032909,-2.64750966082783));
#33515=CARTESIAN_POINT('Ctrl Pts',(372.6361326769,-5.24426732579149,-2.67212909414519));
#33516=CARTESIAN_POINT('Ctrl Pts',(372.614246148032,-5.24262150458826,-2.68675747954303));
#33517=CARTESIAN_POINT('Ctrl Pts',(372.474954430997,-5.23216743712715,-2.77740746607341));
#33518=CARTESIAN_POINT('Ctrl Pts',(372.352898979344,-5.22308754895868,-2.84597661227349));
#33519=CARTESIAN_POINT('Ctrl Pts',(372.035785492412,-5.19974105518724,-2.99790763950144));
#33520=CARTESIAN_POINT('Ctrl Pts',(371.836240520109,-5.18524077418099,-3.07036104077704));
#33521=CARTESIAN_POINT('Ctrl Pts',(371.56359393141,-5.16643288900253,-3.13992340680465));
#33522=CARTESIAN_POINT('Ctrl Pts',(371.495604097281,-5.1618267467785,-3.15494283536281));
#33523=CARTESIAN_POINT('Ctrl Pts',(371.399975495633,-5.15550962580159,-3.17284018677567));
#33524=CARTESIAN_POINT('Ctrl Pts',(371.372708253527,-5.1537265760859,-3.1775807313505));
#33525=CARTESIAN_POINT('Ctrl Pts',(371.324893927462,-5.15063554013575,-3.18526031649999));
#33526=CARTESIAN_POINT('Ctrl Pts',(371.304373529068,-5.14932038718332,-3.18835316147302));
#33527=CARTESIAN_POINT('Ctrl Pts',(371.273917867183,-5.14738680647311,-3.19264302267347));
#33528=CARTESIAN_POINT('Ctrl Pts',(371.264005056932,-5.14676032759744,-3.19399225981672));
#33529=CARTESIAN_POINT('Ctrl Pts',(371.246316843103,-5.14564775979524,-3.19631597246973));
#33530=CARTESIAN_POINT('Ctrl Pts',(371.238544017884,-5.14516069489457,-3.19730827033428));
#33531=CARTESIAN_POINT('Ctrl Pts',(371.221591426488,-5.1441024264937,-3.19940966959952));
#33532=CARTESIAN_POINT('Ctrl Pts',(371.212410480767,-5.1435318486785,-3.20050761980941));
#33533=CARTESIAN_POINT('Ctrl Pts',(371.186761338326,-5.14194458820511,-3.20346309433044));
#33534=CARTESIAN_POINT('Ctrl Pts',(371.170283084457,-5.14093265493638,-3.20523315798925));
#33535=CARTESIAN_POINT('Ctrl Pts',(371.076900694595,-5.13523844693912,-3.21453604746284));
#33536=CARTESIAN_POINT('Ctrl Pts',(370.999752534408,-5.13068904940357,-3.21942880606091));
#33537=CARTESIAN_POINT('Ctrl Pts',(370.900340452009,-5.12494139558371,-3.22214988071866));
#33538=CARTESIAN_POINT('Ctrl Pts',(370.878177992615,-5.12366737439745,-3.22252775905837));
#33539=CARTESIAN_POINT('Ctrl Pts',(370.778335001081,-5.11795415573871,-3.22319990607404));
#33540=CARTESIAN_POINT('Ctrl Pts',(370.700660688103,-5.11358073492079,-3.22091420292741));
#33541=CARTESIAN_POINT('Ctrl Pts',(370.435261082579,-5.09867398897162,-3.20348605622059));
#33542=CARTESIAN_POINT('Ctrl Pts',(370.248832148169,-5.08824278153732,-3.17470815883318));
#33543=CARTESIAN_POINT('Ctrl Pts',(370.003759684228,-5.07369140125921,-3.11454588050704));
#33544=CARTESIAN_POINT('Ctrl Pts',(369.94200666875,-5.06995358368212,-3.09741875352984));
#33545=CARTESIAN_POINT('Ctrl Pts',(369.837022645712,-5.06344652433765,-3.06490144816775));
#33546=CARTESIAN_POINT('Ctrl Pts',(369.793533650584,-5.06070518925956,-3.05040760317297));
#33547=CARTESIAN_POINT('Ctrl Pts',(369.732029457587,-5.05675584460028,-3.0284413718049));
#33548=CARTESIAN_POINT('Ctrl Pts',(369.713748871939,-5.05557277196612,-3.02172500106408));
#33549=CARTESIAN_POINT('Ctrl Pts',(369.682200473244,-5.05351451464985,-3.00980832444101));
#33550=CARTESIAN_POINT('Ctrl Pts',(369.668904071322,-5.05264191495387,-3.00468489426048));
#33551=CARTESIAN_POINT('Ctrl Pts',(369.641746267532,-5.05084891683763,-2.99401294114284));
#33552=CARTESIAN_POINT('Ctrl Pts',(369.627888589966,-5.04992825024649,-2.9884559390301));
#33553=CARTESIAN_POINT('Ctrl Pts',(369.592879723652,-5.04758747589247,-2.97413401170751));
#33554=CARTESIAN_POINT('Ctrl Pts',(369.571782671624,-5.04616302256331,-2.96523972402519));
#33555=CARTESIAN_POINT('Ctrl Pts',(369.491789167395,-5.04070789426281,-2.93050688937293));
#33556=CARTESIAN_POINT('Ctrl Pts',(369.433579388903,-5.03662542487482,-2.90313360149514));
#33557=CARTESIAN_POINT('Ctrl Pts',(369.07673267804,-5.01087243452327,-2.72209441703721));
#33558=CARTESIAN_POINT('Ctrl Pts',(368.802904312656,-4.98758156421748,-2.52431833925148));
#33559=CARTESIAN_POINT('Ctrl Pts',(368.531329336638,-4.96233049908931,-2.2548956390582));
#33560=CARTESIAN_POINT('Ctrl Pts',(368.498806320119,-4.95926989002745,-2.22119264687658));
#33561=CARTESIAN_POINT('Ctrl Pts',(368.446026246626,-4.95425785607234,-2.16405607960657));
#33562=CARTESIAN_POINT('Ctrl Pts',(368.425352334165,-4.95228252375283,-2.14101863755636));
#33563=CARTESIAN_POINT('Ctrl Pts',(368.3972986173,-4.94958941537574,-2.10883679324896));
#33564=CARTESIAN_POINT('Ctrl Pts',(368.389632841798,-4.94885217372389,-2.09994537589614));
#33565=CARTESIAN_POINT('Ctrl Pts',(368.376764180204,-4.94761257147218,-2.08485323625828));
#33566=CARTESIAN_POINT('Ctrl Pts',(368.371535800518,-4.94710837588572,-2.07867449074258));
#33567=CARTESIAN_POINT('Ctrl Pts',(368.361569281017,-4.94614628805035,-2.06680596112113));
#33568=CARTESIAN_POINT('Ctrl Pts',(368.356827412674,-4.94568811083578,-2.06111947782452));
#33569=CARTESIAN_POINT('Ctrl Pts',(368.345521344389,-4.94459448952684,-2.04746576592711));
#33570=CARTESIAN_POINT('Ctrl Pts',(368.338975696935,-4.94396037040533,-2.03948318326187));
#33571=CARTESIAN_POINT('Ctrl Pts',(368.315490599295,-4.94168113495278,-2.01056018534058));
#33572=CARTESIAN_POINT('Ctrl Pts',(368.298774936091,-4.94005112870489,-1.98943841747473));
#33573=CARTESIAN_POINT('Ctrl Pts',(368.178843752613,-4.92827835760766,-1.83392695778037));
#33574=CARTESIAN_POINT('Ctrl Pts',(368.086092707703,-4.91873606956641,-1.6917752193104));
#33575=CARTESIAN_POINT('Ctrl Pts',(367.933190535076,-4.9008545141536,-1.4113960598316));
#33576=CARTESIAN_POINT('Ctrl Pts',(367.870703303659,-4.89252431986466,-1.27497665699189));
#33577=CARTESIAN_POINT('Ctrl Pts',(367.774603510989,-4.87694528387461,-1.01951608987162));
#33578=CARTESIAN_POINT('Ctrl Pts',(367.737908231019,-4.86978422037394,-0.901946457321207));
#33579=CARTESIAN_POINT('Ctrl Pts',(367.701393753535,-4.86076114382184,-0.756075639030048));
#33580=CARTESIAN_POINT('Ctrl Pts',(367.695097743755,-4.8591116428621,-0.729493537308239));
#33581=CARTESIAN_POINT('Ctrl Pts',(367.685674336434,-4.85648528368446,-0.687323927583807));
#33582=CARTESIAN_POINT('Ctrl Pts',(367.682322959629,-4.85551561081848,-0.671787432043597));
#33583=CARTESIAN_POINT('Ctrl Pts',(367.676241920511,-4.85368665205122,-0.642548945607366));
#33584=CARTESIAN_POINT('Ctrl Pts',(367.673486159424,-4.85282822314324,-0.628852715667466));
#33585=CARTESIAN_POINT('Ctrl Pts',(367.667491963347,-4.85089215113474,-0.598026148405397));
#33586=CARTESIAN_POINT('Ctrl Pts',(367.664303321402,-4.84981294929722,-0.580886684207893));
#33587=CARTESIAN_POINT('Ctrl Pts',(367.656507260779,-4.84704248606099,-0.537004454162611));
#33588=CARTESIAN_POINT('Ctrl Pts',(367.652098343247,-4.84534500352673,-0.510228246203521));
#33589=CARTESIAN_POINT('Ctrl Pts',(367.623610513318,-4.83338949410468,-0.322453233494839));
#33590=CARTESIAN_POINT('Ctrl Pts',(367.611426003885,-4.82275828032377,-0.159911944217903));
#33591=CARTESIAN_POINT('Ctrl Pts',(367.611724882292,-4.80004385520079,0.180009964118632));
#33592=CARTESIAN_POINT('Ctrl Pts',(367.626490871899,-4.78795182583808,0.356863727043824));
#33593=CARTESIAN_POINT('Ctrl Pts',(367.674066768005,-4.76862171279464,0.641332939805374));
#33594=CARTESIAN_POINT('Ctrl Pts',(367.698090140048,-4.76126992786214,0.750050526311881));
#33595=CARTESIAN_POINT('Ctrl Pts',(367.732087468951,-4.75313447488548,0.873245219936679));
#33596=CARTESIAN_POINT('Ctrl Pts',(367.736605453394,-4.75208872822624,0.889139182453399));
#33597=CARTESIAN_POINT('Ctrl Pts',(367.744089750632,-4.75041271698354,0.914718764157189));
#33598=CARTESIAN_POINT('Ctrl Pts',(367.746979768377,-4.74977831020298,0.924426146285701));
#33599=CARTESIAN_POINT('Ctrl Pts',(367.752189658175,-4.7486571670899,0.941628858885629));
#33600=CARTESIAN_POINT('Ctrl Pts',(367.754491188119,-4.74816939323319,0.949129514875481));
#33601=CARTESIAN_POINT('Ctrl Pts',(367.759538076874,-4.74711588470862,0.965365592880919));
#33602=CARTESIAN_POINT('Ctrl Pts',(367.762293278958,-4.74655072837297,0.9740977471101));
#33603=CARTESIAN_POINT('Ctrl Pts',(367.770155145203,-4.74496547387296,0.998649483639158));
#33604=CARTESIAN_POINT('Ctrl Pts',(367.775347127892,-4.74395021555722,1.01444172872425));
#33605=CARTESIAN_POINT('Ctrl Pts',(367.809042829425,-4.73755300007197,1.11432112568646));
#33606=CARTESIAN_POINT('Ctrl Pts',(367.840891668857,-4.73234889711195,1.19724817837271));
#33607=CARTESIAN_POINT('Ctrl Pts',(367.992824178923,-4.71033604001266,1.54871742555803));
#33608=CARTESIAN_POINT('Ctrl Pts',(368.145921593542,-4.69448974080339,1.80143171329925));
#33609=CARTESIAN_POINT('Ctrl Pts',(368.382236139445,-4.67271488014358,2.09284079008715));
#33610=CARTESIAN_POINT('Ctrl Pts',(368.435642198235,-4.66793638707432,2.15384326446947));
#33611=CARTESIAN_POINT('Ctrl Pts',(368.508395871514,-4.6615646349442,2.23087995053426));
#33612=CARTESIAN_POINT('Ctrl Pts',(368.525713198257,-4.66005764673338,2.24879588059757));
#33613=CARTESIAN_POINT('Ctrl Pts',(368.55404512125,-4.65760653609023,2.27743497038722));
#33614=CARTESIAN_POINT('Ctrl Pts',(368.564931946076,-4.65666802129122,2.28828349820155));
#33615=CARTESIAN_POINT('Ctrl Pts',(368.585936113334,-4.65486345078466,2.30891645540075));
#33616=CARTESIAN_POINT('Ctrl Pts',(368.596040791321,-4.65399797103665,2.31871331355835));
#33617=CARTESIAN_POINT('Ctrl Pts',(368.619471309767,-4.65199701372289,2.34113418829121));
#33618=CARTESIAN_POINT('Ctrl Pts',(368.63284138339,-4.65085954099763,2.35371107595666));
#33619=CARTESIAN_POINT('Ctrl Pts',(368.675301905866,-4.64726019371105,2.39297431863524));
#33620=CARTESIAN_POINT('Ctrl Pts',(368.704774769939,-4.64478072081449,2.41923996015343));
#33621=CARTESIAN_POINT('Ctrl Pts',(368.856871465799,-4.63207466577503,2.5498523535447));
#33622=CARTESIAN_POINT('Ctrl Pts',(368.986692802258,-4.62150107512343,2.64543188349788));
#33623=CARTESIAN_POINT('Ctrl Pts',(369.277044173948,-4.59853658134947,2.82737030229153));
#33624=CARTESIAN_POINT('Ctrl Pts',(369.438871391191,-4.58612404896,2.91064457028469));
#33625=CARTESIAN_POINT('Ctrl Pts',(369.69429547435,-4.56770124604273,3.015859834663));
#33626=CARTESIAN_POINT('Ctrl Pts',(369.783292055932,-4.56148820231008,3.04801735906208));
#33627=CARTESIAN_POINT('Ctrl Pts',(369.888814923402,-4.55445601495591,3.08097329393238));
#33628=CARTESIAN_POINT('Ctrl Pts',(369.904083061098,-4.55344658837929,3.08561752065752));
#33629=CARTESIAN_POINT('Ctrl Pts',(369.928935184991,-4.55181730817089,3.09297574825196));
#33630=CARTESIAN_POINT('Ctrl Pts',(369.938498153885,-4.55119366570206,3.09575900672334));
#33631=CARTESIAN_POINT('Ctrl Pts',(369.955604887496,-4.55008413455439,3.10065193790939));
#33632=CARTESIAN_POINT('Ctrl Pts',(369.963143576507,-4.54959729198648,3.10277848063583));
#33633=CARTESIAN_POINT('Ctrl Pts',(369.979630917529,-4.54853717935907,3.10736446613637));
#33634=CARTESIAN_POINT('Ctrl Pts',(369.988582463895,-4.54796455268825,3.10981274994618));
#33635=CARTESIAN_POINT('Ctrl Pts',(370.01415602629,-4.54633668878438,3.11668863177166));
#33636=CARTESIAN_POINT('Ctrl Pts',(370.030803371767,-4.5452867156206,3.1210219412368));
#33637=CARTESIAN_POINT('Ctrl Pts',(370.147091868934,-4.53801460299677,3.15029973668505));
#33638=CARTESIAN_POINT('Ctrl Pts',(370.247851427951,-4.53203128649899,3.17060396442827));
#33639=CARTESIAN_POINT('Ctrl Pts',(370.49347607998,-4.51783754306373,3.20798655603339));
#33640=CARTESIAN_POINT('Ctrl Pts',(370.638860227859,-4.50975440810934,3.22011654137405));
#33641=CARTESIAN_POINT('Ctrl Pts',(370.988721150358,-4.49015482597942,3.22551770126043));
#33642=CARTESIAN_POINT('Ctrl Pts',(371.192681092834,-4.47858288576605,3.20926245224846));
#33643=CARTESIAN_POINT('Ctrl Pts',(371.420712669612,-4.46472461313978,3.16907083084951));
#33644=CARTESIAN_POINT('Ctrl Pts',(371.447643079774,-4.46307385105367,3.16396916994804));
#33645=CARTESIAN_POINT('Ctrl Pts',(371.49167159215,-4.46035035335377,3.15504523570459));
#33646=CARTESIAN_POINT('Ctrl Pts',(371.508809728201,-4.4592840703786,3.15142587873747));
#33647=CARTESIAN_POINT('Ctrl Pts',(371.539569490001,-4.45735883915971,3.14466740258357));
#33648=CARTESIAN_POINT('Ctrl Pts',(371.553201897568,-4.45650153378486,3.14157900825419));
#33649=CARTESIAN_POINT('Ctrl Pts',(371.582237709249,-4.45466668314576,3.13480211716403));
#33650=CARTESIAN_POINT('Ctrl Pts',(371.597634830338,-4.45368835217053,3.13108856517249));
#33651=CARTESIAN_POINT('Ctrl Pts',(371.639265326823,-4.45102835527231,3.12072260197273));
#33652=CARTESIAN_POINT('Ctrl Pts',(371.665442837501,-4.44933974013695,3.11385310868284));
#33653=CARTESIAN_POINT('Ctrl Pts',(371.806132368478,-4.44017564550926,3.07503296523369));
#33654=CARTESIAN_POINT('Ctrl Pts',(371.918883867167,-4.43250769055062,3.0370976318991));
#33655=CARTESIAN_POINT('Ctrl Pts',(372.12480754239,-4.41789825027614,2.95488337808739));
#33656=CARTESIAN_POINT('Ctrl Pts',(372.218429702573,-4.41100910571352,2.91220181148356));
#33657=CARTESIAN_POINT('Ctrl Pts',(372.30982074573,-4.40407334669083,2.86513678150012));
#33658=CARTESIAN_POINT('',(367.611567853362,-4.5673390469264,2.97967533004691E-5));
#33659=CARTESIAN_POINT('Ctrl Pts',(372.309820591896,-4.15988901539235,2.86513686072284));
#33660=CARTESIAN_POINT('Ctrl Pts',(372.293919473726,-4.16105047268937,2.87332569935363));
#33661=CARTESIAN_POINT('Ctrl Pts',(372.27794799162,-4.16220630468556,2.88138329414723));
#33662=CARTESIAN_POINT('Ctrl Pts',(372.23775092834,-4.16508694134537,2.90124441904508));
#33663=CARTESIAN_POINT('Ctrl Pts',(372.213444456082,-4.16680325451408,2.91287718567665));
#33664=CARTESIAN_POINT('Ctrl Pts',(372.179621627552,-4.16915350879268,2.92854605760678));
#33665=CARTESIAN_POINT('Ctrl Pts',(372.170228240372,-4.16980221353723,2.93284293835819));
#33666=CARTESIAN_POINT('Ctrl Pts',(372.154061726601,-4.17091158218854,2.94014431067768));
#33667=CARTESIAN_POINT('Ctrl Pts',(372.147298667945,-4.17137355426733,2.94317071229736));
#33668=CARTESIAN_POINT('Ctrl Pts',(372.133119786015,-4.17233756672996,2.94945702136365));
#33669=CARTESIAN_POINT('Ctrl Pts',(372.125702026984,-4.17283930763598,2.95271232920548));
#33670=CARTESIAN_POINT('Ctrl Pts',(372.107493718593,-4.17406477600753,2.96062136524162));
#33671=CARTESIAN_POINT('Ctrl Pts',(372.096689704679,-4.17478664456424,2.96524416719236));
#33672=CARTESIAN_POINT('Ctrl Pts',(372.057298401016,-4.17740028914764,2.98184453228169));
#33673=CARTESIAN_POINT('Ctrl Pts',(372.028562986718,-4.17927203258121,2.99346905068147));
#33674=CARTESIAN_POINT('Ctrl Pts',(371.955928295334,-4.18392684939651,3.02163995791922));
#33675=CARTESIAN_POINT('Ctrl Pts',(371.911826108893,-4.18668395411857,3.03764619624868));
#33676=CARTESIAN_POINT('Ctrl Pts',(371.547476813413,-4.20901857090006,3.16094698166854));
#33677=CARTESIAN_POINT('Ctrl Pts',(371.212530176513,-4.22700316287315,3.21825685678827));
#33678=CARTESIAN_POINT('Ctrl Pts',(370.812104007818,-4.25046439235811,3.22328263691059));
#33679=CARTESIAN_POINT('Ctrl Pts',(370.749438150346,-4.25418376327138,3.22224131227551));
#33680=CARTESIAN_POINT('Ctrl Pts',(370.664193817272,-4.25932617057299,3.21833645612469));
#33681=CARTESIAN_POINT('Ctrl Pts',(370.641554295781,-4.26069985223141,3.21705982273558));
#33682=CARTESIAN_POINT('Ctrl Pts',(370.605558036364,-4.26289736099131,3.21464867995924));
#33683=CARTESIAN_POINT('Ctrl Pts',(370.592191386704,-4.26371631237675,3.21366954665046));
#33684=CARTESIAN_POINT('Ctrl Pts',(370.564757161574,-4.26540337247315,3.21148780671581));
#33685=CARTESIAN_POINT('Ctrl Pts',(370.550690622039,-4.26627174989232,3.21027607579472));
#33686=CARTESIAN_POINT('Ctrl Pts',(370.518102643931,-4.268291511133,3.20725300230315));
#33687=CARTESIAN_POINT('Ctrl Pts',(370.499588170261,-4.26944500784393,3.20537359685805));
#33688=CARTESIAN_POINT('Ctrl Pts',(370.440519256952,-4.27314481708523,3.19886016187596));
#33689=CARTESIAN_POINT('Ctrl Pts',(370.400037435893,-4.27571014026193,3.19361612333886));
#33690=CARTESIAN_POINT('Ctrl Pts',(370.305212883206,-4.28179162241,3.17949627377124));
#33691=CARTESIAN_POINT('Ctrl Pts',(370.250977701844,-4.28532634999213,3.16999405610348));
#33692=CARTESIAN_POINT('Ctrl Pts',(370.050066431028,-4.29863158101186,3.1294632045557));
#33693=CARTESIAN_POINT('Ctrl Pts',(369.905380234927,-4.30864707151545,3.08960461346886));
#33694=CARTESIAN_POINT('Ctrl Pts',(369.558292334868,-4.33349003476182,2.9673963601132));
#33695=CARTESIAN_POINT('Ctrl Pts',(369.360448027307,-4.34839063702113,2.87426577960914));
#33696=CARTESIAN_POINT('Ctrl Pts',(369.152012984451,-4.36399048017446,2.74892662005306));
#33697=CARTESIAN_POINT('Ctrl Pts',(369.130659354596,-4.36558686294989,2.73574396532394));
#33698=CARTESIAN_POINT('Ctrl Pts',(369.10024050926,-4.36785596639115,2.7164705922847));
#33699=CARTESIAN_POINT('Ctrl Pts',(369.091049466776,-4.36854091191462,2.71058149748293));
#33700=CARTESIAN_POINT('Ctrl Pts',(369.075290139734,-4.36971395926281,2.70037050786144));
#33701=CARTESIAN_POINT('Ctrl Pts',(369.0687074606,-4.37020351985001,2.69607109014549));
#33702=CARTESIAN_POINT('Ctrl Pts',(369.056028713149,-4.37114554483955,2.68772372850348));
#33703=CARTESIAN_POINT('Ctrl Pts',(369.049930650029,-4.37159823151033,2.68367908253868));
#33704=CARTESIAN_POINT('Ctrl Pts',(369.033354950083,-4.3728277910272,2.67260348645659));
#33705=CARTESIAN_POINT('Ctrl Pts',(369.02290461539,-4.37360196400808,2.66553162958238));
#33706=CARTESIAN_POINT('Ctrl Pts',(368.981709227445,-4.3766508711397,2.63730009682714));
#33707=CARTESIAN_POINT('Ctrl Pts',(368.951289879049,-4.3788958135154,2.61566749467324));
#33708=CARTESIAN_POINT('Ctrl Pts',(368.872484131582,-4.38471416435397,2.55753755169612));
#33709=CARTESIAN_POINT('Ctrl Pts',(368.824737986983,-4.3882419632125,2.52019433461088));
#33710=CARTESIAN_POINT('Ctrl Pts',(368.538200455607,-4.40962103051671,2.28276291406079));
#33711=CARTESIAN_POINT('Ctrl Pts',(368.328415428144,-4.42636054749662,2.0502768366703));
#33712=CARTESIAN_POINT('Ctrl Pts',(368.118629672299,-4.44843421413053,1.73651818524964));
#33713=CARTESIAN_POINT('Ctrl Pts',(368.083702052769,-4.45233959453823,1.68064556938772));
#33714=CARTESIAN_POINT('Ctrl Pts',(368.038865894922,-4.45769994605102,1.60377687690108));
#33715=CARTESIAN_POINT('Ctrl Pts',(368.027434475627,-4.45909986279602,1.58368481207129));
#33716=CARTESIAN_POINT('Ctrl Pts',(368.008950513878,-4.46142009575002,1.5503681882121));
#33717=CARTESIAN_POINT('Ctrl Pts',(368.001772195655,-4.46233588881326,1.53721410582272));
#33718=CARTESIAN_POINT('Ctrl Pts',(367.987953259396,-4.46412817661317,1.51146579954769));
#33719=CARTESIAN_POINT('Ctrl Pts',(367.981303838433,-4.46500433226035,1.49887667446756));
#33720=CARTESIAN_POINT('Ctrl Pts',(367.965810983394,-4.46707876434762,1.46906794037193));
#33721=CARTESIAN_POINT('Ctrl Pts',(367.957038924547,-4.4682795162656,1.45181204570901));
#33722=CARTESIAN_POINT('Ctrl Pts',(367.928354426482,-4.47229533909766,1.39410435122466));
#33723=CARTESIAN_POINT('Ctrl Pts',(367.90913618507,-4.47513427619917,1.35331528389806));
#33724=CARTESIAN_POINT('Ctrl Pts',(367.865258708932,-4.48198937111957,1.25488434570314));
#33725=CARTESIAN_POINT('Ctrl Pts',(367.841414085328,-4.4860311237511,1.19690146764548));
#33726=CARTESIAN_POINT('Ctrl Pts',(367.758603451583,-4.50133180203989,0.97755193973707));
#33727=CARTESIAN_POINT('Ctrl Pts',(367.710882855977,-4.51290203098739,0.812262034469767));
#33728=CARTESIAN_POINT('Ctrl Pts',(367.639129133981,-4.53719522700026,0.460415284340354));
#33729=CARTESIAN_POINT('Ctrl Pts',(367.617767905853,-4.54988161519056,0.273922287603608));
#33730=CARTESIAN_POINT('Ctrl Pts',(367.612195881093,-4.56313526092677,0.0666743665876585));
#33731=CARTESIAN_POINT('Ctrl Pts',(367.61184489797,-4.5644019459049,0.0467287152035062));
#33732=CARTESIAN_POINT('Ctrl Pts',(367.61162440377,-4.56607408325113,0.0201955132305951));
#33733=CARTESIAN_POINT('Ctrl Pts',(367.611589864399,-4.56648803135677,0.0136102795926603));
#33734=CARTESIAN_POINT('Ctrl Pts',(367.611570427038,-4.56704708473222,0.00469322337694372));
#33735=CARTESIAN_POINT('Ctrl Pts',(367.61156787492,-4.56719313445545,0.00236151425848598));
#33736=CARTESIAN_POINT('Ctrl Pts',(367.611567853362,-4.5673390469264,2.97967533004691E-5));
#33737=CARTESIAN_POINT('Ctrl Pts',(367.611567853355,-4.5673390901344,2.9106277886545E-5));
#33738=CARTESIAN_POINT('Ctrl Pts',(367.61156783133,-4.56749169558373,-0.00240956713773506));
#33739=CARTESIAN_POINT('Ctrl Pts',(367.611570577343,-4.56764415094795,-0.00484825048755294));
#33740=CARTESIAN_POINT('Ctrl Pts',(367.611590360164,-4.56819056498431,-0.013597455458878));
#33741=CARTESIAN_POINT('Ctrl Pts',(367.611623164111,-4.56858365646499,-0.0199079810364738));
#33742=CARTESIAN_POINT('Ctrl Pts',(367.611739809861,-4.5694743820323,-0.0342455138049178));
#33743=CARTESIAN_POINT('Ctrl Pts',(367.611835107448,-4.56997135991083,-0.042272412898108));
#33744=CARTESIAN_POINT('Ctrl Pts',(367.612143532491,-4.57119072346036,-0.0620313833186715));
#33745=CARTESIAN_POINT('Ctrl Pts',(367.612390745664,-4.57191123222472,-0.0737629251980433));
#33746=CARTESIAN_POINT('Ctrl Pts',(367.613502174776,-4.57447190567572,-0.115644657201449));
#33747=CARTESIAN_POINT('Ctrl Pts',(367.614725600891,-4.57629331399327,-0.145784767931852));
#33748=CARTESIAN_POINT('Ctrl Pts',(367.61788208994,-4.5797494032511,-0.203528670621334));
#33749=CARTESIAN_POINT('Ctrl Pts',(367.619747819506,-4.5813869001697,-0.23113314977507));
#33750=CARTESIAN_POINT('Ctrl Pts',(367.635394725314,-4.59282944384832,-0.425416800950013));
#33751=CARTESIAN_POINT('Ctrl Pts',(367.661778371179,-4.6021543633138,-0.590840015721989));
#33752=CARTESIAN_POINT('Ctrl Pts',(367.736884862957,-4.62011598369071,-0.903178918229882));
#33753=CARTESIAN_POINT('Ctrl Pts',(367.783562354811,-4.62872678280989,-1.0501000850242));
#33754=CARTESIAN_POINT('Ctrl Pts',(367.863380652703,-4.64117900050485,-1.25037988907046));
#33755=CARTESIAN_POINT('Ctrl Pts',(367.887840056502,-4.64478014190965,-1.3069757656596));
#33756=CARTESIAN_POINT('Ctrl Pts',(367.93273146274,-4.65107058671465,-1.40317344158835));
#33757=CARTESIAN_POINT('Ctrl Pts',(367.952389672441,-4.65373449939021,-1.44311779116309));
#33758=CARTESIAN_POINT('Ctrl Pts',(367.981729119955,-4.65759202267539,-1.49974199418895));
#33759=CARTESIAN_POINT('Ctrl Pts',(367.99074298682,-4.65876230109209,-1.51676316033512));
#33760=CARTESIAN_POINT('Ctrl Pts',(368.006676485508,-4.66080605425554,-1.54620958950122));
#33761=CARTESIAN_POINT('Ctrl Pts',(368.013526860387,-4.66167705309079,-1.55867185885553));
#33762=CARTESIAN_POINT('Ctrl Pts',(368.026903593353,-4.6633633927571,-1.58262992335582));
#33763=CARTESIAN_POINT('Ctrl Pts',(368.033418651477,-4.66417831552572,-1.59413172422668));
#33764=CARTESIAN_POINT('Ctrl Pts',(368.049050274562,-4.66611870116859,-1.62133641315909));
#33765=CARTESIAN_POINT('Ctrl Pts',(368.058229074867,-4.66724639672523,-1.63700284740387));
#33766=CARTESIAN_POINT('Ctrl Pts',(368.091396324818,-4.67128076144585,-1.69253167803771));
#33767=CARTESIAN_POINT('Ctrl Pts',(368.116114040863,-4.674213831618,-1.73194967137018));
#33768=CARTESIAN_POINT('Ctrl Pts',(368.288398268864,-4.69418858768308,-1.9939190200968));
#33769=CARTESIAN_POINT('Ctrl Pts',(368.46225853107,-4.71225594868572,-2.1978861758204));
#33770=CARTESIAN_POINT('Ctrl Pts',(368.739749156881,-4.73765921718434,-2.45169504942337));
#33771=CARTESIAN_POINT('Ctrl Pts',(368.823968767106,-4.7449912016118,-2.52121521921582));
#33772=CARTESIAN_POINT('Ctrl Pts',(368.941239434253,-4.7545640243675,-2.60839789022961));
#33773=CARTESIAN_POINT('Ctrl Pts',(368.971299750482,-4.7569650906298,-2.62995232684662));
#33774=CARTESIAN_POINT('Ctrl Pts',(369.023062455875,-4.76100219775396,-2.66573521965481));
#33775=CARTESIAN_POINT('Ctrl Pts',(369.044577285141,-4.76265236078809,-2.68022744816824));
#33776=CARTESIAN_POINT('Ctrl Pts',(369.073407207015,-4.76482441100863,-2.6991450911493));
#33777=CARTESIAN_POINT('Ctrl Pts',(369.080567591396,-4.76536070513963,-2.70380297914112));
#33778=CARTESIAN_POINT('Ctrl Pts',(369.094617881,-4.76640671404711,-2.7128635092179));
#33779=CARTESIAN_POINT('Ctrl Pts',(369.101506185877,-4.76691657976865,-2.71726850753316));
#33780=CARTESIAN_POINT('Ctrl Pts',(369.114935001524,-4.76790472565494,-2.72578426242777));
#33781=CARTESIAN_POINT('Ctrl Pts',(369.121473632023,-4.76838318269839,-2.72989778412489));
#33782=CARTESIAN_POINT('Ctrl Pts',(369.137563540009,-4.7695541343471,-2.73993954883162));
#33783=CARTESIAN_POINT('Ctrl Pts',(369.147131275099,-4.7702449166131,-2.74584147211256));
#33784=CARTESIAN_POINT('Ctrl Pts',(369.17970226886,-4.77257855395983,-2.76569859346902));
#33785=CARTESIAN_POINT('Ctrl Pts',(369.20285001411,-4.77420681799314,-2.77941616874181));
#33786=CARTESIAN_POINT('Ctrl Pts',(369.365414364712,-4.78545232999753,-2.87302254474681));
#33787=CARTESIAN_POINT('Ctrl Pts',(369.510480136433,-4.79453092395336,-2.94268619286354));
#33788=CARTESIAN_POINT('Ctrl Pts',(369.835516443079,-4.81409272413024,-3.06984894306167));
#33789=CARTESIAN_POINT('Ctrl Pts',(370.016546079625,-4.82452491184807,-3.12295089737209));
#33790=CARTESIAN_POINT('Ctrl Pts',(370.264007762305,-4.83907789093516,-3.17253380302107));
#33791=CARTESIAN_POINT('Ctrl Pts',(370.327201399934,-4.84281630296755,-3.18324622114236));
#33792=CARTESIAN_POINT('Ctrl Pts',(370.436082814754,-4.84932467247368,-3.19837905885008));
#33793=CARTESIAN_POINT('Ctrl Pts',(370.481623606829,-4.85206672020446,-3.20372068107175));
#33794=CARTESIAN_POINT('Ctrl Pts',(370.546658504854,-4.85601742984184,-3.20994538329748));
#33795=CARTESIAN_POINT('Ctrl Pts',(370.56607190082,-4.85720114455174,-3.21162596634361));
#33796=CARTESIAN_POINT('Ctrl Pts',(370.599715813797,-4.85926065809297,-3.21423128832623));
#33797=CARTESIAN_POINT('Ctrl Pts',(370.613939573923,-4.86013386999416,-3.2152378287568));
#33798=CARTESIAN_POINT('Ctrl Pts',(370.643081708342,-4.86192825955075,-3.21710577863768));
#33799=CARTESIAN_POINT('Ctrl Pts',(370.658000311999,-4.86284970664928,-3.21795788765467));
#33800=CARTESIAN_POINT('Ctrl Pts',(370.695814222956,-4.86519275008332,-3.21985396901567));
#33801=CARTESIAN_POINT('Ctrl Pts',(370.718715442905,-4.86661870224337,-3.22075750042442));
#33802=CARTESIAN_POINT('Ctrl Pts',(370.806011772148,-4.87208169168222,-3.22326939001521));
#33803=CARTESIAN_POINT('Ctrl Pts',(370.870436706153,-4.87617069144845,-3.22319116274022));
#33804=CARTESIAN_POINT('Ctrl Pts',(371.270331054117,-4.90192170300657,-3.21071523171121));
#33805=CARTESIAN_POINT('Ctrl Pts',(371.602062342495,-4.92520163733484,-3.14790228335611));
#33806=CARTESIAN_POINT('Ctrl Pts',(371.962182829444,-4.95044256361864,-3.0193096845631));
#33807=CARTESIAN_POINT('Ctrl Pts',(372.005936928852,-4.95350313697301,-3.00260213193215));
#33808=CARTESIAN_POINT('Ctrl Pts',(372.077984227813,-4.95851541854305,-2.97327592352257));
#33809=CARTESIAN_POINT('Ctrl Pts',(372.106486621939,-4.9604910258847,-2.96119275921003));
#33810=CARTESIAN_POINT('Ctrl Pts',(372.145558182348,-4.96318477632228,-2.94396065076232));
#33811=CARTESIAN_POINT('Ctrl Pts',(372.156278891141,-4.96392238701745,-2.93916221706436));
#33812=CARTESIAN_POINT('Ctrl Pts',(372.174347706462,-4.96516269709834,-2.93095601357467));
#33813=CARTESIAN_POINT('Ctrl Pts',(372.1817095747,-4.96566723267963,-2.9275789852835));
#33814=CARTESIAN_POINT('Ctrl Pts',(372.19578270486,-4.96663005582166,-2.92105904345576));
#33815=CARTESIAN_POINT('Ctrl Pts',(372.202495939613,-4.96708862819769,-2.91792069873949));
#33816=CARTESIAN_POINT('Ctrl Pts',(372.218544847323,-4.96818332561718,-2.91035049170517));
#33817=CARTESIAN_POINT('Ctrl Pts',(372.227870213606,-4.96881812228117,-2.90589679468957));
#33818=CARTESIAN_POINT('Ctrl Pts',(372.261463792011,-4.97110081962247,-2.88965394944243));
#33819=CARTESIAN_POINT('Ctrl Pts',(372.285605908921,-4.97273355670686,-2.87760465762333));
#33820=CARTESIAN_POINT('Ctrl Pts',(372.457232121304,-4.98430520807724,-2.78923683433564));
#33821=CARTESIAN_POINT('Ctrl Pts',(372.5987922299,-4.99366823639472,-2.70191346638495));
#33822=CARTESIAN_POINT('Ctrl Pts',(372.860040759497,-5.01177753712549,-2.51143033901138));
#33823=CARTESIAN_POINT('Ctrl Pts',(372.980127787805,-5.02050877192922,-2.40963343452384));
#33824=CARTESIAN_POINT('Ctrl Pts',(373.177519001036,-5.03631980452203,-2.21580461291884));
#33825=CARTESIAN_POINT('Ctrl Pts',(373.258010337101,-5.04327702672265,-2.12746136562321));
#33826=CARTESIAN_POINT('Ctrl Pts',(373.350526322932,-5.05207079180567,-2.01383899041327));
#33827=CARTESIAN_POINT('Ctrl Pts',(373.367377678986,-5.05370803698993,-1.99260141355721));
#33828=CARTESIAN_POINT('Ctrl Pts',(373.393656996375,-5.05631977412781,-1.95860974520919));
#33829=CARTESIAN_POINT('Ctrl Pts',(373.403262430015,-5.05728722614092,-1.94599402132065));
#33830=CARTESIAN_POINT('Ctrl Pts',(373.421165326502,-5.05911503633787,-1.9221168970291));
#33831=CARTESIAN_POINT('Ctrl Pts',(373.42948335571,-5.05997456172435,-1.9108713250162));
#33832=CARTESIAN_POINT('Ctrl Pts',(373.448054977356,-5.06191719154415,-1.88541846394029));
#33833=CARTESIAN_POINT('Ctrl Pts',(373.458266384025,-5.06300189202151,-1.87118107796508));
#33834=CARTESIAN_POINT('Ctrl Pts',(373.484149126359,-5.06579458313312,-1.8344652183583));
#33835=CARTESIAN_POINT('Ctrl Pts',(373.499650535105,-5.06750895898634,-1.81186920992117));
#33836=CARTESIAN_POINT('Ctrl Pts',(373.634721617425,-5.08282862561395,-1.60949470714902));
#33837=CARTESIAN_POINT('Ctrl Pts',(373.736209965257,-5.09711416821223,-1.41835311086057));
#33838=CARTESIAN_POINT('Ctrl Pts',(373.881592565808,-5.12305659503884,-1.06239466764015));
#33839=CARTESIAN_POINT('Ctrl Pts',(373.933011139083,-5.13455036461611,-0.901481487870583));
#33840=CARTESIAN_POINT('Ctrl Pts',(373.982437730418,-5.14881683692809,-0.691160760332164));
#33841=CARTESIAN_POINT('Ctrl Pts',(373.992258202229,-5.15191426667614,-0.644806303276504));
#33842=CARTESIAN_POINT('Ctrl Pts',(374.006849284367,-5.15698014063531,-0.567570856328441));
#33843=CARTESIAN_POINT('Ctrl Pts',(374.012199202389,-5.15897309814704,-0.536807840724318));
#33844=CARTESIAN_POINT('Ctrl Pts',(374.018951618596,-5.16168635478182,-0.494332096734604));
#33845=CARTESIAN_POINT('Ctrl Pts',(374.020737992468,-5.1624264823062,-0.482683278927524));
#33846=CARTESIAN_POINT('Ctrl Pts',(374.023645356971,-5.16366979310232,-0.463004709257983));
#33847=CARTESIAN_POINT('Ctrl Pts',(374.024800008722,-5.16417483246384,-0.454980117632955));
#33848=CARTESIAN_POINT('Ctrl Pts',(374.026950962201,-5.16513765447608,-0.43962050152736));
#33849=CARTESIAN_POINT('Ctrl Pts',(374.027952288016,-5.16559572831676,-0.432286309539131));
#33850=CARTESIAN_POINT('Ctrl Pts',(374.030286794076,-5.16668799422482,-0.414736335829573));
#33851=CARTESIAN_POINT('Ctrl Pts',(374.03159628511,-5.16732087123557,-0.404517409809721));
#33852=CARTESIAN_POINT('Ctrl Pts',(374.036129707252,-5.16958779118483,-0.367741824506884));
#33853=CARTESIAN_POINT('Ctrl Pts',(374.039072053837,-5.17120694875675,-0.341150725042209));
#33854=CARTESIAN_POINT('Ctrl Pts',(374.059739493092,-5.18390397495795,-0.130394811709377));
#33855=CARTESIAN_POINT('Ctrl Pts',(374.061908748277,-5.19426255870464,0.0549731295664442));
#33856=CARTESIAN_POINT('Ctrl Pts',(374.035357905991,-5.21424318585932,0.411224608262495));
#33857=CARTESIAN_POINT('Ctrl Pts',(374.008822082956,-5.22383835415168,0.581619532240991));
#33858=CARTESIAN_POINT('Ctrl Pts',(373.954945366254,-5.23724444174472,0.807067104760386));
#33859=CARTESIAN_POINT('Ctrl Pts',(373.939478912231,-5.24073195937061,0.864666168279185));
#33860=CARTESIAN_POINT('Ctrl Pts',(373.910010248708,-5.24684135682526,0.963388552580442));
#33861=CARTESIAN_POINT('Ctrl Pts',(373.896757918642,-5.24943983191205,1.00471975742616));
#33862=CARTESIAN_POINT('Ctrl Pts',(373.876487902059,-5.25321914263788,1.06380569319686));
#33863=CARTESIAN_POINT('Ctrl Pts',(373.870140499877,-5.25437795698478,1.08178648206707));
#33864=CARTESIAN_POINT('Ctrl Pts',(373.858792129035,-5.25640833400212,1.11304728351068));
#33865=CARTESIAN_POINT('Ctrl Pts',(373.853862276741,-5.25727751481283,1.1263526821669));
#33866=CARTESIAN_POINT('Ctrl Pts',(373.843509540213,-5.25907698678434,1.15373765974165));
#33867=CARTESIAN_POINT('Ctrl Pts',(373.838075335545,-5.26000763949256,1.16781255842225));
#33868=CARTESIAN_POINT('Ctrl Pts',(373.823891583472,-5.26240199504537,1.20379523536076));
#33869=CARTESIAN_POINT('Ctrl Pts',(373.815000076283,-5.26387044215318,1.2256457460806));
#33870=CARTESIAN_POINT('Ctrl Pts',(373.778963788829,-5.26969816501012,1.31149152155546));
#33871=CARTESIAN_POINT('Ctrl Pts',(373.749993010801,-5.27411871197094,1.37469519565188));
#33872=CARTESIAN_POINT('Ctrl Pts',(373.693283396761,-5.2823269444942,1.48854330779087));
#33873=CARTESIAN_POINT('Ctrl Pts',(373.666183137504,-5.28609279136623,1.53947509423521));
#33874=CARTESIAN_POINT('Ctrl Pts',(373.524893301944,-5.30497582567348,1.78864561345945));
#33875=CARTESIAN_POINT('Ctrl Pts',(373.391190336137,-5.3206423688271,1.97505358556245));
#33876=CARTESIAN_POINT('Ctrl Pts',(373.166295787833,-5.343259300714,2.22708083387742));
#33877=CARTESIAN_POINT('Ctrl Pts',(373.089596701636,-5.35045574351338,2.30471960462456));
#33878=CARTESIAN_POINT('Ctrl Pts',(372.996236868403,-5.35850040755049,2.39008945022414));
#33879=CARTESIAN_POINT('Ctrl Pts',(372.983277444187,-5.35960204742744,2.40174813754398));
#33880=CARTESIAN_POINT('Ctrl Pts',(372.963234798735,-5.36128199031781,2.41948699280532));
#33881=CARTESIAN_POINT('Ctrl Pts',(372.956218925378,-5.36186563473029,2.42564228904179));
#33882=CARTESIAN_POINT('Ctrl Pts',(372.943264027227,-5.36293508759162,2.43690890078574));
#33883=CARTESIAN_POINT('Ctrl Pts',(372.937333107867,-5.3634215295444,2.44202903271365));
#33884=CARTESIAN_POINT('Ctrl Pts',(372.92385876704,-5.36451956682261,2.45357586616033));
#33885=CARTESIAN_POINT('Ctrl Pts',(372.916304346764,-5.36513020483426,2.45998943256101));
#33886=CARTESIAN_POINT('Ctrl Pts',(372.896644362223,-5.36670686378338,2.47652496921642));
#33887=CARTESIAN_POINT('Ctrl Pts',(372.884493666959,-5.36766913245581,2.48659319320744));
#33888=CARTESIAN_POINT('Ctrl Pts',(372.802510091008,-5.37408442786569,2.55351637515286));
#33889=CARTESIAN_POINT('Ctrl Pts',(372.730388073186,-5.37935507280865,2.60751746871394));
#33890=CARTESIAN_POINT('Ctrl Pts',(372.586728704315,-5.38935477448608,2.70596461712801));
#33891=CARTESIAN_POINT('Ctrl Pts',(372.515528521158,-5.39409276530735,2.75076718665827));
#33892=CARTESIAN_POINT('Ctrl Pts',(372.398932304311,-5.40163546964469,2.81791498784454));
#33893=CARTESIAN_POINT('Ctrl Pts',(372.354641551306,-5.40445302519935,2.84205473788886));
#33894=CARTESIAN_POINT('Ctrl Pts',(372.309820461314,-5.4072724248197,2.86513692797036));
#33895=CARTESIAN_POINT('Origin',(370.834317853224,2.31077344927308,0.));
#33896=CARTESIAN_POINT('',(372.309820841127,-6.90205582396877,2.86513673237215));
#33897=CARTESIAN_POINT('',(372.309820613387,-6.65415806382429,2.86513684965521));
#33898=CARTESIAN_POINT('',(372.309820613641,2.31077344927308,2.86513684952399));
#33899=CARTESIAN_POINT('',(367.611568185609,-6.06328577097763,-0.00146369061351841));
#33900=CARTESIAN_POINT('Ctrl Pts',(372.309820841127,-6.90205582396877,2.86513673237218));
#33901=CARTESIAN_POINT('Ctrl Pts',(372.446892394609,-6.89335341312441,2.79454691219575));
#33902=CARTESIAN_POINT('Ctrl Pts',(372.578798052852,-6.88482060320103,2.71417238188656));
#33903=CARTESIAN_POINT('Ctrl Pts',(372.834224677179,-6.86711783945021,2.53216542364717));
#33904=CARTESIAN_POINT('Ctrl Pts',(372.956898778901,-6.85796300922688,2.43025308518973));
#33905=CARTESIAN_POINT('Ctrl Pts',(373.09098498409,-6.84680990289232,2.30093495123234));
#33906=CARTESIAN_POINT('Ctrl Pts',(373.110203648382,-6.84518154058616,2.28192724901351));
#33907=CARTESIAN_POINT('Ctrl Pts',(373.14139789483,-6.84248752696836,2.25028932561982));
#33908=CARTESIAN_POINT('Ctrl Pts',(373.153514522936,-6.84142808893705,2.23779962375938));
#33909=CARTESIAN_POINT('Ctrl Pts',(373.175173777093,-6.83951026579169,2.21510862347118));
#33910=CARTESIAN_POINT('Ctrl Pts',(373.184752413597,-6.83865346919856,2.20494218467981));
#33911=CARTESIAN_POINT('Ctrl Pts',(373.205103405779,-6.83681427000154,2.18305903350481));
#33912=CARTESIAN_POINT('Ctrl Pts',(373.215855626105,-6.83583104204865,2.17132418164365));
#33913=CARTESIAN_POINT('Ctrl Pts',(373.244893132356,-6.83314384750216,2.139157818121));
#33914=CARTESIAN_POINT('Ctrl Pts',(373.263004978278,-6.83143268790175,2.11857218927035));
#33915=CARTESIAN_POINT('Ctrl Pts',(373.362098925185,-6.8218708082262,2.00300279412954));
#33916=CARTESIAN_POINT('Ctrl Pts',(373.43776309168,-6.81380693543997,1.90361856566612));
#33917=CARTESIAN_POINT('Ctrl Pts',(373.590511133459,-6.79575020330898,1.67678860460122));
#33918=CARTESIAN_POINT('Ctrl Pts',(373.664916411395,-6.7857015446068,1.54787839974188));
#33919=CARTESIAN_POINT('Ctrl Pts',(373.804199150838,-6.76423127927737,1.26269210935036));
#33920=CARTESIAN_POINT('Ctrl Pts',(373.866231334591,-6.75283865110786,1.10548526078697));
#33921=CARTESIAN_POINT('Ctrl Pts',(373.923561418022,-6.74026581267486,0.918377516961789));
#33922=CARTESIAN_POINT('Ctrl Pts',(373.931129427964,-6.73855011828964,0.892525208007266));
#33923=CARTESIAN_POINT('Ctrl Pts',(373.941148526574,-6.73620086657586,0.856637202069017));
#33924=CARTESIAN_POINT('Ctrl Pts',(373.943876606714,-6.73555255390665,0.846680869181379));
#33925=CARTESIAN_POINT('Ctrl Pts',(373.948479139774,-6.73444389578485,0.829561248101092));
#33926=CARTESIAN_POINT('Ctrl Pts',(373.950376813739,-6.73398224344689,0.82240436538717));
#33927=CARTESIAN_POINT('Ctrl Pts',(373.95429729247,-6.73301896247213,0.807410287350992));
#33928=CARTESIAN_POINT('Ctrl Pts',(373.956315260584,-6.73251763246957,0.7995719252528));
#33929=CARTESIAN_POINT('Ctrl Pts',(373.961187639811,-6.73129330532713,0.780346531507207));
#33930=CARTESIAN_POINT('Ctrl Pts',(373.964009439518,-6.73057216271791,0.768951205270003));
#33931=CARTESIAN_POINT('Ctrl Pts',(373.974043906044,-6.72796198450127,0.727458406749683));
#33932=CARTESIAN_POINT('Ctrl Pts',(373.980885446218,-6.72609292165653,0.697271800410228));
#33933=CARTESIAN_POINT('Ctrl Pts',(373.996982421315,-6.7214456161622,0.621178710459467));
#33934=CARTESIAN_POINT('Ctrl Pts',(374.00567440897,-6.71869324573128,0.575159273926589));
#33935=CARTESIAN_POINT('Ctrl Pts',(374.068454496733,-6.69648204196127,0.197854993716503));
#33936=CARTESIAN_POINT('Ctrl Pts',(374.07148820629,-6.67860091751119,-0.139836432719794));
#33937=CARTESIAN_POINT('Ctrl Pts',(374.012897362792,-6.6551823444063,-0.535625657501086));
#33938=CARTESIAN_POINT('Ctrl Pts',(374.001563567063,-6.65136357540348,-0.599012767866996));
#33939=CARTESIAN_POINT('Ctrl Pts',(373.983634672657,-6.64610512671085,-0.684430966943835));
#33940=CARTESIAN_POINT('Ctrl Pts',(373.978690911363,-6.64471781268548,-0.706795732458364));
#33941=CARTESIAN_POINT('Ctrl Pts',(373.970131015667,-6.64241344662177,-0.743650690081685));
#33942=CARTESIAN_POINT('Ctrl Pts',(373.966651752029,-6.64150079934517,-0.758172060434328));
#33943=CARTESIAN_POINT('Ctrl Pts',(373.959655649395,-6.63971093570322,-0.786501262742072));
#33944=CARTESIAN_POINT('Ctrl Pts',(373.956147904371,-6.6388340307947,-0.800311000707794));
#33945=CARTESIAN_POINT('Ctrl Pts',(373.947630670008,-6.63675185004074,-0.832934518771759));
#33946=CARTESIAN_POINT('Ctrl Pts',(373.942542085688,-6.63554404046041,-0.851726893882208));
#33947=CARTESIAN_POINT('Ctrl Pts',(373.924912884816,-6.63147624093134,-0.914569612306046));
#33948=CARTESIAN_POINT('Ctrl Pts',(373.911604043972,-6.6285915166329,-0.958396879757595));
#33949=CARTESIAN_POINT('Ctrl Pts',(373.877467718884,-6.62160394354454,-1.06275731639248));
#33950=CARTESIAN_POINT('Ctrl Pts',(373.855762434972,-6.61747415369357,-1.12298084149327));
#33951=CARTESIAN_POINT('Ctrl Pts',(373.763326588186,-6.6010200597628,-1.35732807196608));
#33952=CARTESIAN_POINT('Ctrl Pts',(373.679221629631,-6.58831567479994,-1.52575899481742));
#33953=CARTESIAN_POINT('Ctrl Pts',(373.542229000303,-6.57060449359006,-1.74894528109535));
#33954=CARTESIAN_POINT('Ctrl Pts',(373.501361069712,-6.56560896492734,-1.81065551816899));
#33955=CARTESIAN_POINT('Ctrl Pts',(373.44098132957,-6.55865727947021,-1.89534266333292));
#33956=CARTESIAN_POINT('Ctrl Pts',(373.423217458109,-6.55665991678401,-1.91953567475778));
#33957=CARTESIAN_POINT('Ctrl Pts',(373.360515991192,-6.54978094402636,-2.00247614013516));
#33958=CARTESIAN_POINT('Ctrl Pts',(373.313892447476,-6.54495999603694,-2.05992703600282));
#33959=CARTESIAN_POINT('Ctrl Pts',(373.254580636894,-6.53922091527929,-2.12807746373779));
#33960=CARTESIAN_POINT('Ctrl Pts',(373.243737656792,-6.53818692128459,-2.14034620332716));
#33961=CARTESIAN_POINT('Ctrl Pts',(373.226655825798,-6.53658224054839,-2.15937982929537));
#33962=CARTESIAN_POINT('Ctrl Pts',(373.220480879619,-6.53600702305893,-2.1662013384265));
#33963=CARTESIAN_POINT('Ctrl Pts',(373.208990054352,-6.53494573298259,-2.1787865830763));
#33964=CARTESIAN_POINT('Ctrl Pts',(373.203682378979,-6.53445909343855,-2.18455734267345));
#33965=CARTESIAN_POINT('Ctrl Pts',(373.191512849654,-6.53335138689304,-2.19769211180579));
#33966=CARTESIAN_POINT('Ctrl Pts',(373.184637524374,-6.53273135560205,-2.2050433826243));
#33967=CARTESIAN_POINT('Ctrl Pts',(373.163266056152,-6.53082137009418,-2.2276807722289));
#33968=CARTESIAN_POINT('Ctrl Pts',(373.148654061155,-6.52953991727228,-2.24285740183799));
#33969=CARTESIAN_POINT('Ctrl Pts',(373.114125204356,-6.52656521624545,-2.27802374156552));
#33970=CARTESIAN_POINT('Ctrl Pts',(373.094092292398,-6.52487991779016,-2.29789758696194));
#33971=CARTESIAN_POINT('Ctrl Pts',(373.022272209683,-6.51896827323452,-2.36729968616246));
#33972=CARTESIAN_POINT('Ctrl Pts',(372.969094493663,-6.51482532170411,-2.41536375030839));
#33973=CARTESIAN_POINT('Ctrl Pts',(372.744273465411,-6.49803271466705,-2.60533483974566));
#33974=CARTESIAN_POINT('Ctrl Pts',(372.559753280602,-6.48585916314058,-2.73103995950967));
#33975=CARTESIAN_POINT('Ctrl Pts',(372.251943300907,-6.46593764364697,-2.89699630579767));
#33976=CARTESIAN_POINT('Ctrl Pts',(372.136691447572,-6.45856297045994,-2.95060454869883));
#33977=CARTESIAN_POINT('Ctrl Pts',(371.992290975987,-6.44925650623475,-3.00765941634025));
#33978=CARTESIAN_POINT('Ctrl Pts',(371.965861299857,-6.44755080829368,-3.01770215049889));
#33979=CARTESIAN_POINT('Ctrl Pts',(371.924021409797,-6.44484538739048,-3.03297352075642));
#33980=CARTESIAN_POINT('Ctrl Pts',(371.908697494484,-6.44385344139408,-3.03843554977043));
#33981=CARTESIAN_POINT('Ctrl Pts',(371.880167647274,-6.44200435787329,-3.04836186860532));
#33982=CARTESIAN_POINT('Ctrl Pts',(371.8669727836,-6.44114826531107,-3.05285696664257));
#33983=CARTESIAN_POINT('Ctrl Pts',(371.837679272839,-6.43924549464988,-3.06262475410036));
#33984=CARTESIAN_POINT('Ctrl Pts',(371.821567462975,-6.43819749130379,-3.06785637103739));
#33985=CARTESIAN_POINT('Ctrl Pts',(371.774673251665,-6.43514263972458,-3.08267558247427));
#33986=CARTESIAN_POINT('Ctrl Pts',(371.743787990991,-6.43312493735024,-3.09192835773758));
#33987=CARTESIAN_POINT('Ctrl Pts',(371.51372314424,-6.41804810885342,-3.1571071611854));
#33988=CARTESIAN_POINT('Ctrl Pts',(371.309744021941,-6.40437421990259,-3.19419157391678));
#33989=CARTESIAN_POINT('Ctrl Pts',(370.873228545825,-6.37484117695963,-3.23080057504636));
#33990=CARTESIAN_POINT('Ctrl Pts',(370.641381343263,-6.35899736323217,-3.22527138914597));
#33991=CARTESIAN_POINT('Ctrl Pts',(370.387670777281,-6.34259864488468,-3.19174431074535));
#33992=CARTESIAN_POINT('Ctrl Pts',(370.363266789622,-6.34103163207958,-3.18823404674786));
#33993=CARTESIAN_POINT('Ctrl Pts',(370.329358362898,-6.33887098415899,-3.18295881418284));
#33994=CARTESIAN_POINT('Ctrl Pts',(370.319818662773,-6.33826495491931,-3.18143072976608));
#33995=CARTESIAN_POINT('Ctrl Pts',(370.302431506568,-6.33716393930254,-3.17856537491825));
#33996=CARTESIAN_POINT('Ctrl Pts',(370.294581857678,-6.3366681920633,-3.17724188387632));
#33997=CARTESIAN_POINT('Ctrl Pts',(370.278372924292,-6.33564734401255,-3.17444717017625));
#33998=CARTESIAN_POINT('Ctrl Pts',(370.27001444868,-6.33512246817047,-3.17297199353753));
#33999=CARTESIAN_POINT('Ctrl Pts',(370.248297181179,-6.33376251190411,-3.16905061028242));
#34000=CARTESIAN_POINT('Ctrl Pts',(370.234947691061,-6.33293029178216,-3.16655292429836));
#34001=CARTESIAN_POINT('Ctrl Pts',(370.176713327614,-6.32931467659187,-3.15527582553062));
#34002=CARTESIAN_POINT('Ctrl Pts',(370.132000091599,-6.32657693748643,-3.14562545339615));
#34003=CARTESIAN_POINT('Ctrl Pts',(370.008410714701,-6.31907878876051,-3.11618450289966));
#34004=CARTESIAN_POINT('Ctrl Pts',(369.930052477949,-6.31440344224549,-3.09435523613195));
#34005=CARTESIAN_POINT('Ctrl Pts',(369.600246962528,-6.29474813856902,-2.98887636784676));
#34006=CARTESIAN_POINT('Ctrl Pts',(369.358818170017,-6.2803272324562,-2.87736290000783));
#34007=CARTESIAN_POINT('Ctrl Pts',(369.067385788044,-6.26038725858426,-2.69632593445081));
#34008=CARTESIAN_POINT('Ctrl Pts',(369.002540926176,-6.25577614474766,-2.65269943919194));
#34009=CARTESIAN_POINT('Ctrl Pts',(368.919455444492,-6.24959751185227,-2.59230098450764));
#34010=CARTESIAN_POINT('Ctrl Pts',(368.899728718044,-6.2481097057964,-2.57761270665809));
#34011=CARTESIAN_POINT('Ctrl Pts',(368.86800707355,-6.24568216215418,-2.5534238837455));
#34012=CARTESIAN_POINT('Ctrl Pts',(368.855908078481,-6.24474783205663,-2.54406099826553));
#34013=CARTESIAN_POINT('Ctrl Pts',(368.833235093359,-6.24298071598243,-2.52625581063233));
#34014=CARTESIAN_POINT('Ctrl Pts',(368.822646682586,-6.24214869153614,-2.51783234647173));
#34015=CARTESIAN_POINT('Ctrl Pts',(368.797981664877,-6.24019443576712,-2.49795552691375));
#34016=CARTESIAN_POINT('Ctrl Pts',(368.783948243745,-6.23907009968133,-2.4864495428932));
#34017=CARTESIAN_POINT('Ctrl Pts',(368.754838493488,-6.23671138649727,-2.4621684809128));
#34018=CARTESIAN_POINT('Ctrl Pts',(368.739781028224,-6.23547616548171,-2.44937206172184));
#34019=CARTESIAN_POINT('Ctrl Pts',(368.699984154187,-6.23217043294926,-2.4149158106224));
#34020=CARTESIAN_POINT('Ctrl Pts',(368.675457452492,-6.23009009851335,-2.3930149088394));
#34021=CARTESIAN_POINT('Ctrl Pts',(368.600871512289,-6.2236281338583,-2.32433407742402));
#34022=CARTESIAN_POINT('Ctrl Pts',(368.551968043607,-6.21919710828186,-2.27633251774844));
#34023=CARTESIAN_POINT('Ctrl Pts',(368.356101315751,-6.20062939238671,-2.07141732366066));
#34024=CARTESIAN_POINT('Ctrl Pts',(368.223500222658,-6.18599376763104,-1.9015626888273));
#34025=CARTESIAN_POINT('Ctrl Pts',(368.0344254805,-6.16211132973905,-1.60192033437473));
#34026=CARTESIAN_POINT('Ctrl Pts',(367.967760098142,-6.15281687364757,-1.47932464634205));
#34027=CARTESIAN_POINT('Ctrl Pts',(367.901454239857,-6.14275633088275,-1.33595376161416));
#34028=CARTESIAN_POINT('Ctrl Pts',(367.893815554852,-6.14158290300053,-1.31905560863843));
#34029=CARTESIAN_POINT('Ctrl Pts',(367.882411098926,-6.13980967031998,-1.29323540717272));
#34030=CARTESIAN_POINT('Ctrl Pts',(367.878539121885,-6.13920373995296,-1.28436108689566));
#34031=CARTESIAN_POINT('Ctrl Pts',(367.871611748158,-6.13811273588198,-1.26828674529169));
#34032=CARTESIAN_POINT('Ctrl Pts',(367.868542536894,-6.13762684725247,-1.26109298217696));
#34033=CARTESIAN_POINT('Ctrl Pts',(367.861796606737,-6.13655326646389,-1.24512070728884));
#34034=CARTESIAN_POINT('Ctrl Pts',(367.85813257332,-6.13596633891776,-1.23633705826225));
#34035=CARTESIAN_POINT('Ctrl Pts',(367.847526010034,-6.13425566946592,-1.21058993773158));
#34036=CARTESIAN_POINT('Ctrl Pts',(367.840689089049,-6.13313806371801,-1.19358299669216));
#34037=CARTESIAN_POINT('Ctrl Pts',(367.780222024197,-6.12310804971261,-1.03938175458849));
#34038=CARTESIAN_POINT('Ctrl Pts',(367.735904898476,-6.11468928018671,-0.898701273464923));
#34039=CARTESIAN_POINT('Ctrl Pts',(367.641820444849,-6.09208711059418,-0.508528810391087));
#34040=CARTESIAN_POINT('Ctrl Pts',(367.611683538068,-6.07815590120095,-0.255446393395135));
#34041=CARTESIAN_POINT('Ctrl Pts',(367.611568185609,-6.06328577097763,-0.00146369061351841));
#34042=CARTESIAN_POINT('Ctrl Pts',(367.611568184028,-6.06328556681864,-0.00146020356699756));
#34043=CARTESIAN_POINT('Ctrl Pts',(367.611539244412,-6.05954603902345,0.062411120851928));
#34044=CARTESIAN_POINT('Ctrl Pts',(367.613409087385,-6.05575672432227,0.126266582787961));
#34045=CARTESIAN_POINT('Ctrl Pts',(367.618182957693,-6.05087840916228,0.207089875612405));
#34046=CARTESIAN_POINT('Ctrl Pts',(367.619326856252,-6.04984414080902,0.224148957221984));
#34047=CARTESIAN_POINT('Ctrl Pts',(367.621615547105,-6.04798666905739,0.254643387303945));
#34048=CARTESIAN_POINT('Ctrl Pts',(367.622709026922,-6.04716507779549,0.268082264691209));
#34049=CARTESIAN_POINT('Ctrl Pts',(367.625085669961,-6.04550183866907,0.295185911476749));
#34050=CARTESIAN_POINT('Ctrl Pts',(367.626371856455,-6.04466011273546,0.308850127116892));
#34051=CARTESIAN_POINT('Ctrl Pts',(367.629321910275,-6.04284619567293,0.338181597033085));
#34052=CARTESIAN_POINT('Ctrl Pts',(367.631013460942,-6.04187315438594,0.353845648839862));
#34053=CARTESIAN_POINT('Ctrl Pts',(367.635878782547,-6.03924247684461,0.396001176480478));
#34054=CARTESIAN_POINT('Ctrl Pts',(367.639266736747,-6.03757815017155,0.422466229345509));
#34055=CARTESIAN_POINT('Ctrl Pts',(367.6552555992,-6.03037271326554,0.5361384512225));
#34056=CARTESIAN_POINT('Ctrl Pts',(367.671100442776,-6.02473081457682,0.622843867273276));
#34057=CARTESIAN_POINT('Ctrl Pts',(367.749485152616,-6.00150712561223,0.970522076588505));
#34058=CARTESIAN_POINT('Ctrl Pts',(367.840948055225,-5.98308396179967,1.22385001830504));
#34059=CARTESIAN_POINT('Ctrl Pts',(368.009489108193,-5.95826542715404,1.55469658778462));
#34060=CARTESIAN_POINT('Ctrl Pts',(368.06065307993,-5.95147878890013,1.64424055670162));
#34061=CARTESIAN_POINT('Ctrl Pts',(368.125272828011,-5.94383115329439,1.745705855968));
#34062=CARTESIAN_POINT('Ctrl Pts',(368.134636209348,-5.94274345555182,1.76015139584845));
#34063=CARTESIAN_POINT('Ctrl Pts',(368.149226465424,-5.94108050121446,1.78227045436131));
#34064=CARTESIAN_POINT('Ctrl Pts',(368.154371337295,-5.9405000611648,1.78999732127292));
#34065=CARTESIAN_POINT('Ctrl Pts',(368.163918816166,-5.93943399659535,1.8042028424957));
#34066=CARTESIAN_POINT('Ctrl Pts',(368.168311645713,-5.9389477620736,1.81068766430725));
#34067=CARTESIAN_POINT('Ctrl Pts',(368.178341994965,-5.93784710102366,1.82537911859818));
#34068=CARTESIAN_POINT('Ctrl Pts',(368.183993925263,-5.93723365688225,1.83357567864285));
#34069=CARTESIAN_POINT('Ctrl Pts',(368.198797117646,-5.93564406068218,1.8548321522468));
#34070=CARTESIAN_POINT('Ctrl Pts',(368.208007612657,-5.93467176730296,1.86785074471336));
#34071=CARTESIAN_POINT('Ctrl Pts',(368.272340714533,-5.9279910604388,1.95736577711319));
#34072=CARTESIAN_POINT('Ctrl Pts',(368.330705976247,-5.92248278159927,2.03148681455096));
#34073=CARTESIAN_POINT('Ctrl Pts',(368.574619507245,-5.90106205422521,2.3147344375505));
#34074=CARTESIAN_POINT('Ctrl Pts',(368.783768902299,-5.88594776528905,2.50189825819353));
#34075=CARTESIAN_POINT('Ctrl Pts',(369.062872364133,-5.86637546771942,2.69286846076214));
#34076=CARTESIAN_POINT('Ctrl Pts',(369.112185755965,-5.86294221292882,2.72466881132525));
#34077=CARTESIAN_POINT('Ctrl Pts',(369.187565934845,-5.85771163265759,2.77041450901184));
#34078=CARTESIAN_POINT('Ctrl Pts',(369.213002706554,-5.85594954045975,2.78537709184092));
#34079=CARTESIAN_POINT('Ctrl Pts',(369.26010913922,-5.8526893287266,2.81222244178752));
#34080=CARTESIAN_POINT('Ctrl Pts',(369.28171703119,-5.85119500215675,2.82420940670251));
#34081=CARTESIAN_POINT('Ctrl Pts',(369.313473676777,-5.84899956767055,2.84135179821847));
#34082=CARTESIAN_POINT('Ctrl Pts',(369.323515630691,-5.84830544561255,2.84670400454189));
#34083=CARTESIAN_POINT('Ctrl Pts',(369.345681470656,-5.84677341666518,2.85836773424642));
#34084=CARTESIAN_POINT('Ctrl Pts',(369.35781753995,-5.84593469208649,2.86465551148483));
#34085=CARTESIAN_POINT('Ctrl Pts',(369.384382160909,-5.84409880537337,2.87820516326082));
#34086=CARTESIAN_POINT('Ctrl Pts',(369.398825987761,-5.8431005863361,2.88543611308199));
#34087=CARTESIAN_POINT('Ctrl Pts',(369.438242490569,-5.84037617479904,2.90479981544941));
#34088=CARTESIAN_POINT('Ctrl Pts',(369.463318124988,-5.83864262613811,2.91671871350854));
#34089=CARTESIAN_POINT('Ctrl Pts',(369.595130666028,-5.82952594022202,2.97729623363457));
#34090=CARTESIAN_POINT('Ctrl Pts',(369.704300119261,-5.82195659181683,3.02041920593439));
#34091=CARTESIAN_POINT('Ctrl Pts',(370.033243110302,-5.7991092016066,3.13002242793859));
#34092=CARTESIAN_POINT('Ctrl Pts',(370.258035125555,-5.78339689622959,3.17909470302125));
#34093=CARTESIAN_POINT('Ctrl Pts',(370.559930554501,-5.76306051872167,3.2119067123616));
#34094=CARTESIAN_POINT('Ctrl Pts',(370.634022713615,-5.75813544528334,3.21737724870512));
#34095=CARTESIAN_POINT('Ctrl Pts',(370.737116578394,-5.75142769137663,3.221413431359));
#34096=CARTESIAN_POINT('Ctrl Pts',(370.766006159496,-5.74956385637366,3.2221555235457));
#34097=CARTESIAN_POINT('Ctrl Pts',(370.816360771322,-5.74634716202605,3.22277141875104));
#34098=CARTESIAN_POINT('Ctrl Pts',(370.837821468653,-5.74498635293178,3.2228195507165));
#34099=CARTESIAN_POINT('Ctrl Pts',(370.869422040718,-5.74299903829848,3.22257476113986));
#34100=CARTESIAN_POINT('Ctrl Pts',(370.879562113329,-5.74236383949316,3.22244834847615));
#34101=CARTESIAN_POINT('Ctrl Pts',(370.897547290067,-5.7412418329857,3.22213922327345));
#34102=CARTESIAN_POINT('Ctrl Pts',(370.905392506158,-5.74075398162457,3.22197571903854));
#34103=CARTESIAN_POINT('Ctrl Pts',(370.922382310282,-5.73970091844178,3.22155954393622));
#34104=CARTESIAN_POINT('Ctrl Pts',(370.931526448042,-5.73913628038372,3.22129659262414));
#34105=CARTESIAN_POINT('Ctrl Pts',(370.956798681234,-5.7375813509795,3.22046214761416));
#34106=CARTESIAN_POINT('Ctrl Pts',(370.972924044491,-5.73659550455844,3.21980843311473));
#34107=CARTESIAN_POINT('Ctrl Pts',(371.059423094149,-5.73133784858712,3.21565076238878));
#34108=CARTESIAN_POINT('Ctrl Pts',(371.129677865334,-5.72717612557223,3.20996047387969));
#34109=CARTESIAN_POINT('Ctrl Pts',(371.235447617676,-5.72099990598649,3.19789108264644));
#34110=CARTESIAN_POINT('Ctrl Pts',(371.27113049078,-5.718931765215,3.19321269628482));
#34111=CARTESIAN_POINT('Ctrl Pts',(371.377983281881,-5.7127661268078,3.17737851210452));
#34112=CARTESIAN_POINT('Ctrl Pts',(371.44886629653,-5.70871242291332,3.16443314720259));
#34113=CARTESIAN_POINT('Ctrl Pts',(371.702802991032,-5.69414850917993,3.10920145387516));
#34114=CARTESIAN_POINT('Ctrl Pts',(371.882496989033,-5.68374071244819,3.05331242588356));
#34115=CARTESIAN_POINT('Ctrl Pts',(372.115510217665,-5.66921920274728,2.95783004317388));
#34116=CARTESIAN_POINT('Ctrl Pts',(372.173984236574,-5.66548598465645,2.93180928669995));
#34117=CARTESIAN_POINT('Ctrl Pts',(372.257877872205,-5.65997371746155,2.89144290609159));
#34118=CARTESIAN_POINT('Ctrl Pts',(372.283939590603,-5.65823885468281,2.87846519053259));
#34119=CARTESIAN_POINT('Ctrl Pts',(372.30982061461,-5.65649214416028,2.86513684902516));
#34120=CARTESIAN_POINT('Ctrl Pts',(372.309820461314,-5.4072724248197,2.86513692797033));
#34121=CARTESIAN_POINT('Ctrl Pts',(372.186239463848,-5.4150460915779,2.92877929085081));
#34122=CARTESIAN_POINT('Ctrl Pts',(372.058627177371,-5.42284083113338,2.98438186264552));
#34123=CARTESIAN_POINT('Ctrl Pts',(371.867273855704,-5.43456887136001,3.05340065678803));
#34124=CARTESIAN_POINT('Ctrl Pts',(371.806139567173,-5.43832013238138,3.07340454444319));
#34125=CARTESIAN_POINT('Ctrl Pts',(371.700348157215,-5.44484885616589,3.10454870238293));
#34126=CARTESIAN_POINT('Ctrl Pts',(371.655974979956,-5.44759816664708,3.11658633448786));
#34127=CARTESIAN_POINT('Ctrl Pts',(371.592429936567,-5.45155752707934,3.1323735635436));
#34128=CARTESIAN_POINT('Ctrl Pts',(371.573456789038,-5.45274247695973,3.13690479297624));
#34129=CARTESIAN_POINT('Ctrl Pts',(371.540541678734,-5.4548034435136,3.14445049293052));
#34130=CARTESIAN_POINT('Ctrl Pts',(371.526618541187,-5.45567686300672,3.14754519289953));
#34131=CARTESIAN_POINT('Ctrl Pts',(371.498073849647,-5.45747103982129,3.15369127088984));
#34132=CARTESIAN_POINT('Ctrl Pts',(371.483450725912,-5.45839206219915,3.15673362140282));
#34133=CARTESIAN_POINT('Ctrl Pts',(371.446367399543,-5.46073272770172,3.1641802672731));
#34134=CARTESIAN_POINT('Ctrl Pts',(371.423880737914,-5.46215670891125,3.16844709164471));
#34135=CARTESIAN_POINT('Ctrl Pts',(371.338162263589,-5.46760354590136,3.18376801036029));
#34136=CARTESIAN_POINT('Ctrl Pts',(371.274654148141,-5.47167797227647,3.19317098493991));
#34137=CARTESIAN_POINT('Ctrl Pts',(370.877256354232,-5.4974291217939,3.23992909185907));
#34138=CARTESIAN_POINT('Ctrl Pts',(370.539607690508,-5.52072828445761,3.22677088942471));
#34139=CARTESIAN_POINT('Ctrl Pts',(370.164178289157,-5.5459881856634,3.15265353728662));
#34140=CARTESIAN_POINT('Ctrl Pts',(370.118428010833,-5.54904946714131,3.14258071344138));
#34141=CARTESIAN_POINT('Ctrl Pts',(370.042827808043,-5.55406277923187,3.12419903259107));
#34142=CARTESIAN_POINT('Ctrl Pts',(370.01284989712,-5.55603872070489,3.11645097003691));
#34143=CARTESIAN_POINT('Ctrl Pts',(369.971658253245,-5.55873284699157,3.10516890787206));
#34144=CARTESIAN_POINT('Ctrl Pts',(369.960346300446,-5.55947050632391,3.10200407266341));
#34145=CARTESIAN_POINT('Ctrl Pts',(369.941263824579,-5.56071087436503,3.0965525452388));
#34146=CARTESIAN_POINT('Ctrl Pts',(369.933484222796,-5.56121541965395,3.09429829507254));
#34147=CARTESIAN_POINT('Ctrl Pts',(369.918603341941,-5.56217824264502,3.08992546981398));
#34148=CARTESIAN_POINT('Ctrl Pts',(369.911500784834,-5.56263680528618,3.08781170670755));
#34149=CARTESIAN_POINT('Ctrl Pts',(369.894511558581,-5.56373145531434,3.082691757458));
#34150=CARTESIAN_POINT('Ctrl Pts',(369.884631861335,-5.56436621458216,3.07966245983421));
#34151=CARTESIAN_POINT('Ctrl Pts',(369.849014855198,-5.56664859678286,3.06855393192067));
#34152=CARTESIAN_POINT('Ctrl Pts',(369.823363857998,-5.5682810617331,3.06019890833389));
#34153=CARTESIAN_POINT('Ctrl Pts',(369.634697472273,-5.58022519345597,2.99611537870492));
#34154=CARTESIAN_POINT('Ctrl Pts',(369.476259274897,-5.589916022736,2.92771036007857));
#34155=CARTESIAN_POINT('Ctrl Pts',(369.298807585165,-5.60116034997856,2.83357394148913));
#34156=CARTESIAN_POINT('Ctrl Pts',(369.273759454107,-5.60275682758361,2.81985647756629));
#34157=CARTESIAN_POINT('Ctrl Pts',(369.109318899195,-5.61331755039553,2.72693938952893));
#34158=CARTESIAN_POINT('Ctrl Pts',(368.975826813608,-5.62228812348054,2.63776916406592));
#34159=CARTESIAN_POINT('Ctrl Pts',(368.804413680532,-5.63489234161843,2.50377435913618));
#34160=CARTESIAN_POINT('Ctrl Pts',(368.760246525718,-5.63824624820379,2.46731120468146));
#34161=CARTESIAN_POINT('Ctrl Pts',(368.685354763773,-5.6441419642904,2.402050272421));
#34162=CARTESIAN_POINT('Ctrl Pts',(368.654179139217,-5.64666259071267,2.37379081057311));
#34163=CARTESIAN_POINT('Ctrl Pts',(368.609861956208,-5.65034864833123,2.33200949541366));
#34164=CARTESIAN_POINT('Ctrl Pts',(368.596270949407,-5.65149356851119,2.31896924461198));
#34165=CARTESIAN_POINT('Ctrl Pts',(368.572669405879,-5.6535078311931,2.29592337793145));
#34166=CARTESIAN_POINT('Ctrl Pts',(368.56260893164,-5.65437490505648,2.28596947097292));
#34167=CARTESIAN_POINT('Ctrl Pts',(368.543197891067,-5.65606460104076,2.26650935899122));
#34168=CARTESIAN_POINT('Ctrl Pts',(368.533840104199,-5.65688687773175,2.25701073836825));
#34169=CARTESIAN_POINT('Ctrl Pts',(368.508979071966,-5.65909232983623,2.23146031118641));
#34170=CARTESIAN_POINT('Ctrl Pts',(368.493583372466,-5.66048013314703,2.21530531042468));
#34171=CARTESIAN_POINT('Ctrl Pts',(368.437323955151,-5.66563470700402,2.1550299740053));
#34172=CARTESIAN_POINT('Ctrl Pts',(368.397531829565,-5.66944621620575,2.10993057575255));
#34173=CARTESIAN_POINT('Ctrl Pts',(368.175314089758,-5.69172948204876,1.84339902400083));
#34174=CARTESIAN_POINT('Ctrl Pts',(368.021868594206,-5.71134792605097,1.59952964443848));
#34175=CARTESIAN_POINT('Ctrl Pts',(367.857022921374,-5.73799640278554,1.23852645710416));
#34176=CARTESIAN_POINT('Ctrl Pts',(367.816457563919,-5.7452964325378,1.13611480142608));
#34177=CARTESIAN_POINT('Ctrl Pts',(367.773403710924,-5.75391104960634,1.0087203098643));
#34178=CARTESIAN_POINT('Ctrl Pts',(367.765859465314,-5.75546052358208,0.985532980055936));
#34179=CARTESIAN_POINT('Ctrl Pts',(367.755389394627,-5.75766815478191,0.952066811207538));
#34180=CARTESIAN_POINT('Ctrl Pts',(367.752250593291,-5.75833789029135,0.941856188082666));
#34181=CARTESIAN_POINT('Ctrl Pts',(367.746874362096,-5.75949880478419,0.924052437148957));
#34182=CARTESIAN_POINT('Ctrl Pts',(367.74461405419,-5.75999129187723,0.916466397142653));
#34183=CARTESIAN_POINT('Ctrl Pts',(367.739888503829,-5.7610302960024,0.900390313591055));
#34184=CARTESIAN_POINT('Ctrl Pts',(367.737430230393,-5.76157641215277,0.891898408533948));
#34185=CARTESIAN_POINT('Ctrl Pts',(367.730852388209,-5.76305344236891,0.868820683870069));
#34186=CARTESIAN_POINT('Ctrl Pts',(367.726800659244,-5.7639805253179,0.854215536666795));
#34187=CARTESIAN_POINT('Ctrl Pts',(367.708351195327,-5.76828712690331,0.785842375956361));
#34188=CARTESIAN_POINT('Ctrl Pts',(367.695244059027,-5.77159891140568,0.73173241766537));
#34189=CARTESIAN_POINT('Ctrl Pts',(367.674240686848,-5.7774511503991,0.634026490146115));
#34190=CARTESIAN_POINT('Ctrl Pts',(367.665829375583,-5.78001001950418,0.590557656326112));
#34191=CARTESIAN_POINT('Ctrl Pts',(367.627365642879,-5.79299171439672,0.367199311458932));
#34192=CARTESIAN_POINT('Ctrl Pts',(367.611725866657,-5.80303882109623,0.185161274399618));
#34193=CARTESIAN_POINT('Ctrl Pts',(367.611419465318,-5.82308882301199,-0.171195433130785));
#34194=CARTESIAN_POINT('Ctrl Pts',(367.625355720298,-5.83304143910263,-0.344866322988589));
#34195=CARTESIAN_POINT('Ctrl Pts',(367.657623113375,-5.8450906358744,-0.543578693342448));
#34196=CARTESIAN_POINT('Ctrl Pts',(367.662355922668,-5.84673972965104,-0.570547725989014));
#34197=CARTESIAN_POINT('Ctrl Pts',(367.670678608738,-5.84946144372453,-0.614663360760454));
#34198=CARTESIAN_POINT('Ctrl Pts',(367.674065726059,-5.85052763272903,-0.631847125681856));
#34199=CARTESIAN_POINT('Ctrl Pts',(367.680409424716,-5.85245333840517,-0.662702666909461));
#34200=CARTESIAN_POINT('Ctrl Pts',(367.683315284648,-5.85331121677272,-0.676384508407327));
#34201=CARTESIAN_POINT('Ctrl Pts',(367.689706079449,-5.85514800174256,-0.705539445109354));
#34202=CARTESIAN_POINT('Ctrl Pts',(367.693216349764,-5.85612770033602,-0.721006551264223));
#34203=CARTESIAN_POINT('Ctrl Pts',(367.703040149695,-5.85879322649739,-0.762858786501047));
#34204=CARTESIAN_POINT('Ctrl Pts',(367.709572806134,-5.86048604505668,-0.789190663364817));
#34205=CARTESIAN_POINT('Ctrl Pts',(367.746735799547,-5.86970890343693,-0.931286112576606));
#34206=CARTESIAN_POINT('Ctrl Pts',(367.7834643043,-5.87743433897533,-1.04534374219022));
#34207=CARTESIAN_POINT('Ctrl Pts',(367.883206651629,-5.89574451353938,-1.30462668954683));
#34208=CARTESIAN_POINT('Ctrl Pts',(367.95073986068,-5.90643416708659,-1.44778419797886));
#34209=CARTESIAN_POINT('Ctrl Pts',(368.109553035553,-5.92827086630111,-1.72885020926833));
#34210=CARTESIAN_POINT('Ctrl Pts',(368.201499436149,-5.93938519581037,-1.86588956408876));
#34211=CARTESIAN_POINT('Ctrl Pts',(368.320277867226,-5.95171211272316,-2.01654457803009));
#34212=CARTESIAN_POINT('Ctrl Pts',(368.337290681605,-5.95343503684842,-2.03757318934979));
#34213=CARTESIAN_POINT('Ctrl Pts',(368.361173006976,-5.95579265964947,-2.06634438335263));
#34214=CARTESIAN_POINT('Ctrl Pts',(368.367817541967,-5.9564422433307,-2.07427114007633));
#34215=CARTESIAN_POINT('Ctrl Pts',(368.379289538424,-5.95755271877109,-2.08782386376487));
#34216=CARTESIAN_POINT('Ctrl Pts',(368.384098412003,-5.9580149243778,-2.0934653579804));
#34217=CARTESIAN_POINT('Ctrl Pts',(368.394200783242,-5.95897897110095,-2.10523438424517));
#34218=CARTESIAN_POINT('Ctrl Pts',(368.399497966312,-5.95948051531581,-2.11135862607016));
#34219=CARTESIAN_POINT('Ctrl Pts',(368.412528065296,-5.96070475901002,-2.12630888608184));
#34220=CARTESIAN_POINT('Ctrl Pts',(368.420286307752,-5.96142560826559,-2.13511286898364));
#34221=CARTESIAN_POINT('Ctrl Pts',(368.448635518875,-5.96403133900457,-2.16693123783337));
#34222=CARTESIAN_POINT('Ctrl Pts',(368.469509638147,-5.96589634637568,-2.1896925481519));
#34223=CARTESIAN_POINT('Ctrl Pts',(368.522747754332,-5.97053092370751,-2.24609436269053));
#34224=CARTESIAN_POINT('Ctrl Pts',(368.555522180627,-5.97327481306805,-2.27933914119107));
#34225=CARTESIAN_POINT('Ctrl Pts',(368.826968421333,-5.99525100898732,-2.54297112291339));
#34226=CARTESIAN_POINT('Ctrl Pts',(369.099185866976,-6.01293529023208,-2.73596591989263));
#34227=CARTESIAN_POINT('Ctrl Pts',(369.456610086862,-6.03627228767671,-2.91420869580126));
#34228=CARTESIAN_POINT('Ctrl Pts',(369.518060963434,-6.04027863151131,-2.94247478348002));
#34229=CARTESIAN_POINT('Ctrl Pts',(369.601856275252,-6.04575669451562,-2.97786852213719));
#34230=CARTESIAN_POINT('Ctrl Pts',(369.623457722889,-6.04717012579401,-2.98671729113938));
#34231=CARTESIAN_POINT('Ctrl Pts',(369.659126259294,-6.0495068977796,-3.0008779227979));
#34232=CARTESIAN_POINT('Ctrl Pts',(369.673138009274,-6.05042558363183,-3.00632748514916));
#34233=CARTESIAN_POINT('Ctrl Pts',(369.700469797614,-6.05221924207341,-3.0167380020541));
#34234=CARTESIAN_POINT('Ctrl Pts',(369.713785553786,-6.05309384432302,-3.02170927487675));
#34235=CARTESIAN_POINT('Ctrl Pts',(369.745179601369,-6.05515782555169,-3.0331938068646));
#34236=CARTESIAN_POINT('Ctrl Pts',(369.763283969941,-6.0563496105485,-3.03963372742106));
#34237=CARTESIAN_POINT('Ctrl Pts',(369.823270520261,-6.0603040423247,-3.06036914382988));
#34238=CARTESIAN_POINT('Ctrl Pts',(369.86538808978,-6.06308956684437,-3.07396337112632));
#34239=CARTESIAN_POINT('Ctrl Pts',(369.966357865119,-6.06979182859552,-3.10427201982976));
#34240=CARTESIAN_POINT('Ctrl Pts',(370.025430656397,-6.0737326709091,-3.12018589783273));
#34241=CARTESIAN_POINT('Ctrl Pts',(370.26034608079,-6.08947921254514,-3.17635142081367));
#34242=CARTESIAN_POINT('Ctrl Pts',(370.438969159845,-6.10164017966511,-3.20348849598836));
#34243=CARTESIAN_POINT('Ctrl Pts',(370.792282445117,-6.12559644672119,-3.22715754906267));
#34244=CARTESIAN_POINT('Ctrl Pts',(370.96633357674,-6.13734497591492,-3.22473190618839));
#34245=CARTESIAN_POINT('Ctrl Pts',(371.166197746252,-6.1502440447933,-3.2057293140122));
#34246=CARTESIAN_POINT('Ctrl Pts',(371.193010081644,-6.15196170685305,-3.20284009807007));
#34247=CARTESIAN_POINT('Ctrl Pts',(371.230041939978,-6.15431346637567,-3.19837877094988));
#34248=CARTESIAN_POINT('Ctrl Pts',(371.24029405509,-6.15496235218232,-3.19709362478578));
#34249=CARTESIAN_POINT('Ctrl Pts',(371.257887873061,-6.15607194878778,-3.19480217044204));
#34250=CARTESIAN_POINT('Ctrl Pts',(371.265232536767,-6.15653396892638,-3.19381981459431));
#34251=CARTESIAN_POINT('Ctrl Pts',(371.280598459769,-6.15749798822373,-3.19171063704249));
#34252=CARTESIAN_POINT('Ctrl Pts',(371.288618947901,-6.15799968843602,-3.19057889536439));
#34253=CARTESIAN_POINT('Ctrl Pts',(371.308261322736,-6.15922490370889,-3.1877316634573));
#34254=CARTESIAN_POINT('Ctrl Pts',(371.319878403891,-6.15994656165555,-3.18598282042769));
#34255=CARTESIAN_POINT('Ctrl Pts',(371.36208627872,-6.16255856943343,-3.17939259365022));
#34256=CARTESIAN_POINT('Ctrl Pts',(371.392617512743,-6.1644289195043,-3.1741736604391));
#34257=CARTESIAN_POINT('Ctrl Pts',(371.469142194923,-6.16907954763586,-3.15995435886714));
#34258=CARTESIAN_POINT('Ctrl Pts',(371.515024481363,-6.17183391679983,-3.15038924827447));
#34259=CARTESIAN_POINT('Ctrl Pts',(371.888485220933,-6.19409262858897,-3.06399299279539));
#34260=CARTESIAN_POINT('Ctrl Pts',(372.202398297669,-6.21201358385623,-2.93729768488005));
#34261=CARTESIAN_POINT('Ctrl Pts',(372.545687215412,-6.23544765087213,-2.73155462476746));
#34262=CARTESIAN_POINT('Ctrl Pts',(372.599343085592,-6.23922719549706,-2.6971950022383));
#34263=CARTESIAN_POINT('Ctrl Pts',(372.670787501203,-6.24444021101523,-2.64839905596115));
#34264=CARTESIAN_POINT('Ctrl Pts',(372.689494318392,-6.24582251914817,-2.63532893005722));
#34265=CARTESIAN_POINT('Ctrl Pts',(372.718987452923,-6.24803038246378,-2.61425294044089));
#34266=CARTESIAN_POINT('Ctrl Pts',(372.729865463735,-6.24885097723792,-2.60637625533105));
#34267=CARTESIAN_POINT('Ctrl Pts',(372.75206730125,-6.25053887106962,-2.59008756639953));
#34268=CARTESIAN_POINT('Ctrl Pts',(372.763385752716,-6.25140642281705,-2.58166875801697));
#34269=CARTESIAN_POINT('Ctrl Pts',(372.789438071178,-6.25341993850836,-2.56202373191591));
#34270=CARTESIAN_POINT('Ctrl Pts',(372.804131036853,-6.2545679739355,-2.55074433610989));
#34271=CARTESIAN_POINT('Ctrl Pts',(372.850513409426,-6.25823240996628,-2.51449807625842));
#34272=CARTESIAN_POINT('Ctrl Pts',(372.881830638747,-6.26076731335264,-2.48906332831767));
#34273=CARTESIAN_POINT('Ctrl Pts',(373.041221218716,-6.27399261236492,-2.35456806503931));
#34274=CARTESIAN_POINT('Ctrl Pts',(373.161072123743,-6.28506324721286,-2.23620506278547));
#34275=CARTESIAN_POINT('Ctrl Pts',(373.327844290165,-6.30217209919381,-2.04351532255935));
#34276=CARTESIAN_POINT('Ctrl Pts',(373.381894558315,-6.30803808864141,-1.97572298571586));
#34277=CARTESIAN_POINT('Ctrl Pts',(373.531389509746,-6.32513809661236,-1.77186936324884));
#34278=CARTESIAN_POINT('Ctrl Pts',(373.619137203418,-6.3363479292754,-1.6304932444753));
#34279=CARTESIAN_POINT('Ctrl Pts',(373.708012340677,-6.34875729366153,-1.4590152444706));
#34280=CARTESIAN_POINT('Ctrl Pts',(373.720126612015,-6.35047590745691,-1.43490536590241));
#34281=CARTESIAN_POINT('Ctrl Pts',(373.736460513246,-6.35282872848166,-1.40135375167505));
#34282=CARTESIAN_POINT('Ctrl Pts',(373.740939263383,-6.35347774150518,-1.39204035188978));
#34283=CARTESIAN_POINT('Ctrl Pts',(373.748552639291,-6.35458749829496,-1.37601166034474));
#34284=CARTESIAN_POINT('Ctrl Pts',(373.751709011472,-6.35504955222302,-1.36930687215259));
#34285=CARTESIAN_POINT('Ctrl Pts',(373.758266719398,-6.35601357640553,-1.35525133853584));
#34286=CARTESIAN_POINT('Ctrl Pts',(373.761663509263,-6.35651524808664,-1.34789857721087));
#34287=CARTESIAN_POINT('Ctrl Pts',(373.769918111233,-6.35774028581146,-1.32985211139402));
#34288=CARTESIAN_POINT('Ctrl Pts',(373.774745312679,-6.35846179600048,-1.31914437367508));
#34289=CARTESIAN_POINT('Ctrl Pts',(373.792081288789,-6.36107265594432,-1.28012156141589));
#34290=CARTESIAN_POINT('Ctrl Pts',(373.804240929777,-6.36294202894683,-1.25165204143015));
#34291=CARTESIAN_POINT('Ctrl Pts',(373.83375947724,-6.36758972050476,-1.17968651364065));
#34292=CARTESIAN_POINT('Ctrl Pts',(373.850584497862,-6.37034217201583,-1.13597811962276));
#34293=CARTESIAN_POINT('Ctrl Pts',(373.980149387566,-6.39254822546715,-0.77619044425526));
#34294=CARTESIAN_POINT('Ctrl Pts',(374.043845046602,-6.41042504550552,-0.444637494304166));
#34295=CARTESIAN_POINT('Ctrl Pts',(374.057400341852,-6.43384043187916,-0.0448069411441706));
#34296=CARTESIAN_POINT('Ctrl Pts',(374.057651872717,-6.4376618020501,0.0196303817915023));
#34297=CARTESIAN_POINT('Ctrl Pts',(374.055374571373,-6.44292389101207,0.106941743267279));
#34298=CARTESIAN_POINT('Ctrl Pts',(374.05453253706,-6.44431217079368,0.12984708855978));
#34299=CARTESIAN_POINT('Ctrl Pts',(374.05273803169,-6.44661817461632,0.16766758839743));
#34300=CARTESIAN_POINT('Ctrl Pts',(374.051925999098,-6.44753148784421,0.182588808939438));
#34301=CARTESIAN_POINT('Ctrl Pts',(374.050136373031,-6.44932268809116,0.211735999864728));
#34302=CARTESIAN_POINT('Ctrl Pts',(374.04916807607,-6.45020026335615,0.225962209781886));
#34303=CARTESIAN_POINT('Ctrl Pts',(374.046653275178,-6.45228409406142,0.259611933047504));
#34304=CARTESIAN_POINT('Ctrl Pts',(374.045024976747,-6.45349288755933,0.279028599144768));
#34305=CARTESIAN_POINT('Ctrl Pts',(374.03897566626,-6.45756436300435,0.344074730035997));
#34306=CARTESIAN_POINT('Ctrl Pts',(374.033757322504,-6.46045182619141,0.389622706998321));
#34307=CARTESIAN_POINT('Ctrl Pts',(374.018920380266,-6.46744655095895,0.498527321177381));
#34308=CARTESIAN_POINT('Ctrl Pts',(374.008380493129,-6.4715808129513,0.561736782739229));
#34309=CARTESIAN_POINT('Ctrl Pts',(373.959481311576,-6.48806132015112,0.809263486138512));
#34310=CARTESIAN_POINT('Ctrl Pts',(373.906890783748,-6.50078891824815,0.99037160556896));
#34311=CARTESIAN_POINT('Ctrl Pts',(373.810588761087,-6.51879287909948,1.23855287275506));
#34312=CARTESIAN_POINT('Ctrl Pts',(373.779740210269,-6.52405819203512,1.31022499802935));
#34313=CARTESIAN_POINT('Ctrl Pts',(373.736044100385,-6.53086626734648,1.40238287158192));
#34314=CARTESIAN_POINT('Ctrl Pts',(373.725525664752,-6.53246163041849,1.42394184020765));
#34315=CARTESIAN_POINT('Ctrl Pts',(373.680967156958,-6.53903880636466,1.51274089347325));
#34316=CARTESIAN_POINT('Ctrl Pts',(373.644811590333,-6.54395395856,1.57889966590804));
#34317=CARTESIAN_POINT('Ctrl Pts',(373.597970883461,-6.54978841168879,1.65789337363744));
#34318=CARTESIAN_POINT('Ctrl Pts',(373.589466804292,-6.55082802564608,1.67198767757387));
#34319=CARTESIAN_POINT('Ctrl Pts',(373.576028756203,-6.55243978822487,1.6938783861857));
#34320=CARTESIAN_POINT('Ctrl Pts',(373.571168804601,-6.55301652606224,1.70171958255));
#34321=CARTESIAN_POINT('Ctrl Pts',(373.562113860181,-6.5540796010804,1.71618997982436));
#34322=CARTESIAN_POINT('Ctrl Pts',(373.557928348137,-6.55456651500292,1.72282470855387));
#34323=CARTESIAN_POINT('Ctrl Pts',(373.548325259104,-6.55567358391706,1.73792473023129));
#34324=CARTESIAN_POINT('Ctrl Pts',(373.542892284489,-6.55629271271324,1.74638000554083));
#34325=CARTESIAN_POINT('Ctrl Pts',(373.526003763162,-6.55819568423188,1.77239501449796));
#34326=CARTESIAN_POINT('Ctrl Pts',(373.514416093333,-6.55947112100088,1.78986887822688));
#34327=CARTESIAN_POINT('Ctrl Pts',(373.486935469234,-6.56242931638564,1.83044351798534));
#34328=CARTESIAN_POINT('Ctrl Pts',(373.470909733037,-6.56410425008228,1.85345273945323));
#34329=CARTESIAN_POINT('Ctrl Pts',(373.413273615909,-6.56996536372484,1.93394413587852));
#34330=CARTESIAN_POINT('Ctrl Pts',(373.37006518626,-6.57406970619767,1.99026115369087));
#34331=CARTESIAN_POINT('Ctrl Pts',(373.185798105848,-6.59064283709314,2.21467769875871));
#34332=CARTESIAN_POINT('Ctrl Pts',(373.029612304558,-6.60264404547919,2.36958764979766));
#34333=CARTESIAN_POINT('Ctrl Pts',(372.757039786174,-6.62257607109155,2.58967091665331));
#34334=CARTESIAN_POINT('Ctrl Pts',(372.650280601474,-6.63016767624629,2.66561974775489));
#34335=CARTESIAN_POINT('Ctrl Pts',(372.515030912718,-6.63971901318882,2.74993323761919));
#34336=CARTESIAN_POINT('Ctrl Pts',(372.49065644522,-6.64143753371583,2.76468290942012));
#34337=CARTESIAN_POINT('Ctrl Pts',(372.452012924334,-6.64415928925798,2.78737272520168));
#34338=CARTESIAN_POINT('Ctrl Pts',(372.437873245029,-6.64515459617277,2.79553110202655));
#34339=CARTESIAN_POINT('Ctrl Pts',(372.411654742565,-6.64699936070706,2.81039440977952));
#34340=CARTESIAN_POINT('Ctrl Pts',(372.399593562393,-6.64784769649852,2.81712980635673));
#34341=CARTESIAN_POINT('Ctrl Pts',(372.372732512545,-6.64973651083064,2.83190422745332));
#34342=CARTESIAN_POINT('Ctrl Pts',(372.357912255929,-6.65077831752186,2.83990515621556));
#34343=CARTESIAN_POINT('Ctrl Pts',(372.331993764463,-6.65259994732182,2.85363634972696));
#34344=CARTESIAN_POINT('Ctrl Pts',(372.320923718942,-6.65337787613019,2.85941891583469));
#34345=CARTESIAN_POINT('Ctrl Pts',(372.309820613387,-6.65415806382428,2.86513684965516));
#34346=CARTESIAN_POINT('Origin',(370.834317853224,2.31077344927308,0.));
#34347=CARTESIAN_POINT('',(372.309820650725,-8.15202831126679,2.86513683042648));
#34348=CARTESIAN_POINT('',(372.309820607824,-7.90820793933162,2.86513685252006));
#34349=CARTESIAN_POINT('',(372.309820613641,2.31077344927308,2.86513684952399));
#34350=CARTESIAN_POINT('Ctrl Pts',(372.309820650725,-8.15202831126679,2.86513683042647));
#34351=CARTESIAN_POINT('Ctrl Pts',(372.323157571693,-8.15102149794463,2.85826851475322));
#34352=CARTESIAN_POINT('Ctrl Pts',(372.336448474012,-8.15001625546536,2.85130607789403));
#34353=CARTESIAN_POINT('Ctrl Pts',(372.441400777517,-8.14206547264375,2.79538903575093));
#34354=CARTESIAN_POINT('Ctrl Pts',(372.53070234652,-8.13522062520822,2.74211587856899));
#34355=CARTESIAN_POINT('Ctrl Pts',(372.631646819999,-8.12751651434263,2.67507449152134));
#34356=CARTESIAN_POINT('Ctrl Pts',(372.645935751365,-8.12642683112325,2.66541846089678));
#34357=CARTESIAN_POINT('Ctrl Pts',(372.667801608005,-8.12476149377197,2.65038509965079));
#34358=CARTESIAN_POINT('Ctrl Pts',(372.675433692125,-8.1241806335481,2.645089096483));
#34359=CARTESIAN_POINT('Ctrl Pts',(372.689458234654,-8.12311417906914,2.63526717255438));
#34360=CARTESIAN_POINT('Ctrl Pts',(372.695857082674,-8.12262797136739,2.63075095836954));
#34361=CARTESIAN_POINT('Ctrl Pts',(372.71034593757,-8.1215278512809,2.62044560045896));
#34362=CARTESIAN_POINT('Ctrl Pts',(372.71842564001,-8.12091491714605,2.61464230290493));
#34363=CARTESIAN_POINT('Ctrl Pts',(372.739364531988,-8.11932753178647,2.59945535011332));
#34364=CARTESIAN_POINT('Ctrl Pts',(372.752181470257,-8.11835692159696,2.59001353961863));
#34365=CARTESIAN_POINT('Ctrl Pts',(372.839870118988,-8.11171962291826,2.52440837494779));
#34366=CARTESIAN_POINT('Ctrl Pts',(372.912341449471,-8.10625011593137,2.46509611666199));
#34367=CARTESIAN_POINT('Ctrl Pts',(373.190987653675,-8.08482534328028,2.2160100859226));
#34368=CARTESIAN_POINT('Ctrl Pts',(373.374608888315,-8.06967948590491,2.00288013568444));
#34369=CARTESIAN_POINT('Ctrl Pts',(373.560593229343,-8.05006733033921,1.71958972527295));
#34370=CARTESIAN_POINT('Ctrl Pts',(373.591473130989,-8.04663090798016,1.66962883496073));
#34371=CARTESIAN_POINT('Ctrl Pts',(373.642514071746,-8.04060347027495,1.58176834041408));
#34372=CARTESIAN_POINT('Ctrl Pts',(373.663315143799,-8.0380350026733,1.54425747654311));
#34373=CARTESIAN_POINT('Ctrl Pts',(373.692227763668,-8.03429211329185,1.48957322332976));
#34374=CARTESIAN_POINT('Ctrl Pts',(373.700946370354,-8.03313912880729,1.4727248096038));
#34375=CARTESIAN_POINT('Ctrl Pts',(373.715914443979,-8.03111604140217,1.44316295276664));
#34376=CARTESIAN_POINT('Ctrl Pts',(373.722229837002,-8.03024827618769,1.43048333927043));
#34377=CARTESIAN_POINT('Ctrl Pts',(373.735107500368,-8.02844894997796,1.40419557843276));
#34378=CARTESIAN_POINT('Ctrl Pts',(373.741658073453,-8.027517008733,1.39058211944082));
#34379=CARTESIAN_POINT('Ctrl Pts',(373.758245514548,-8.02511343484465,1.35548038274676));
#34380=CARTESIAN_POINT('Ctrl Pts',(373.768141195735,-8.02363698020214,1.33392675335642));
#34381=CARTESIAN_POINT('Ctrl Pts',(373.806551858351,-8.01773161845332,1.24776968568249));
#34382=CARTESIAN_POINT('Ctrl Pts',(373.833176265874,-8.01323931822478,1.18234983921741));
#34383=CARTESIAN_POINT('Ctrl Pts',(373.971318862361,-7.98748304324973,0.808150860148312));
#34384=CARTESIAN_POINT('Ctrl Pts',(374.037265187733,-7.96472207678056,0.484707553345173));
#34385=CARTESIAN_POINT('Ctrl Pts',(374.055510525264,-7.9399942349586,0.110454362570149));
#34386=CARTESIAN_POINT('Ctrl Pts',(374.056769568199,-7.93695384560728,0.0639357420940327));
#34387=CARTESIAN_POINT('Ctrl Pts',(374.057187210583,-7.9319712493563,-0.0133994785397873));
#34388=CARTESIAN_POINT('Ctrl Pts',(374.056911919766,-7.93000546910445,-0.0442050364260089));
#34389=CARTESIAN_POINT('Ctrl Pts',(374.055922254066,-7.92732310805148,-0.0867176435588243));
#34390=CARTESIAN_POINT('Ctrl Pts',(374.055585657342,-7.92658725898352,-0.0984307337497683));
#34391=CARTESIAN_POINT('Ctrl Pts',(374.054908705317,-7.92534931591621,-0.118226759624611));
#34392=CARTESIAN_POINT('Ctrl Pts',(374.054601788839,-7.9248453979212,-0.126310658308434));
#34393=CARTESIAN_POINT('Ctrl Pts',(374.053955474544,-7.92388330419433,-0.141795765460727));
#34394=CARTESIAN_POINT('Ctrl Pts',(374.053620991389,-7.92342484704272,-0.149197047335861));
#34395=CARTESIAN_POINT('Ctrl Pts',(374.052758516461,-7.92232986400548,-0.166925702656494));
#34396=CARTESIAN_POINT('Ctrl Pts',(374.052206332691,-7.92169467055758,-0.177251892698772));
#34397=CARTESIAN_POINT('Ctrl Pts',(374.050029071712,-7.91940630419859,-0.214596193861981));
#34398=CARTESIAN_POINT('Ctrl Pts',(374.048113293538,-7.91776840435768,-0.241597069532205));
#34399=CARTESIAN_POINT('Ctrl Pts',(374.032169695779,-7.90630095566361,-0.432248266640488));
#34400=CARTESIAN_POINT('Ctrl Pts',(374.005987382573,-7.89703406587436,-0.59465987295074));
#34401=CARTESIAN_POINT('Ctrl Pts',(373.909999865642,-7.87406182893423,-0.993329125360318));
#34402=CARTESIAN_POINT('Ctrl Pts',(373.825332180905,-7.86045494851778,-1.22488525863979));
#34403=CARTESIAN_POINT('Ctrl Pts',(373.693666467329,-7.8430871635382,-1.48746296230229));
#34404=CARTESIAN_POINT('Ctrl Pts',(373.671201036714,-7.8402198124507,-1.52987385218172));
#34405=CARTESIAN_POINT('Ctrl Pts',(373.638126957642,-7.83612063277615,-1.58907686100853));
#34406=CARTESIAN_POINT('Ctrl Pts',(373.628296620073,-7.83491645981166,-1.60629803818117));
#34407=CARTESIAN_POINT('Ctrl Pts',(373.611098560172,-7.83283329000884,-1.63579072784455));
#34408=CARTESIAN_POINT('Ctrl Pts',(373.603806782248,-7.83195705423776,-1.64810602249446));
#34409=CARTESIAN_POINT('Ctrl Pts',(373.589696093211,-7.8302744698756,-1.67157988733902));
#34410=CARTESIAN_POINT('Ctrl Pts',(373.582890808186,-7.82946863143004,-1.68274634700933));
#34411=CARTESIAN_POINT('Ctrl Pts',(373.56675890601,-7.82757133727133,-1.70885744822382));
#34412=CARTESIAN_POINT('Ctrl Pts',(373.557377411126,-7.82647787498777,-1.72376753353049));
#34413=CARTESIAN_POINT('Ctrl Pts',(373.529272924605,-7.82323067319133,-1.76763220776888));
#34414=CARTESIAN_POINT('Ctrl Pts',(373.510207430439,-7.82106429128604,-1.79636334887088));
#34415=CARTESIAN_POINT('Ctrl Pts',(373.33765255225,-7.80176567000371,-2.04755450253322));
#34416=CARTESIAN_POINT('Ctrl Pts',(373.157230007828,-7.78354596247333,-2.2501528156186));
#34417=CARTESIAN_POINT('Ctrl Pts',(372.829493271979,-7.75413405289148,-2.53625254655176));
#34418=CARTESIAN_POINT('Ctrl Pts',(372.697133136911,-7.74304758107349,-2.63500151689255));
#34419=CARTESIAN_POINT('Ctrl Pts',(372.540652015528,-7.73123338819568,-2.73403590439073));
#34420=CARTESIAN_POINT('Ctrl Pts',(372.523418181754,-7.72994895536709,-2.74471651157215));
#34421=CARTESIAN_POINT('Ctrl Pts',(372.497611366226,-7.72805164044615,-2.76037505978007));
#34422=CARTESIAN_POINT('Ctrl Pts',(372.489114731316,-7.72743112682183,-2.76547700757778));
#34423=CARTESIAN_POINT('Ctrl Pts',(372.474508783813,-7.72637173762073,-2.7741559774975));
#34424=CARTESIAN_POINT('Ctrl Pts',(372.46841108259,-7.72593163433138,-2.77775214830033));
#34425=CARTESIAN_POINT('Ctrl Pts',(372.45452368636,-7.72493426176666,-2.78588080125242));
#34426=CARTESIAN_POINT('Ctrl Pts',(372.446726802409,-7.72437780467917,-2.79040071777072));
#34427=CARTESIAN_POINT('Ctrl Pts',(372.425430052538,-7.72286711090915,-2.80262754712821));
#34428=CARTESIAN_POINT('Ctrl Pts',(372.411893024294,-7.72191691725905,-2.81026970246221));
#34429=CARTESIAN_POINT('Ctrl Pts',(372.343535287058,-7.7171664166256,-2.84821058562495));
#34430=CARTESIAN_POINT('Ctrl Pts',(372.287891038818,-7.7134526572714,-2.87700659480662));
#34431=CARTESIAN_POINT('Ctrl Pts',(371.95518424719,-7.691930420183,-3.0370635331236));
#34432=CARTESIAN_POINT('Ctrl Pts',(371.661367406825,-7.67551157967861,-3.12987553083968));
#34433=CARTESIAN_POINT('Ctrl Pts',(371.296503535557,-7.65417528237968,-3.1900616464876));
#34434=CARTESIAN_POINT('Ctrl Pts',(371.233882925903,-7.65048786005654,-3.19850839667869));
#34435=CARTESIAN_POINT('Ctrl Pts',(371.125955601382,-7.64406070290072,-3.2098475958595));
#34436=CARTESIAN_POINT('Ctrl Pts',(371.080760867094,-7.6413479346913,-3.21363341086185));
#34437=CARTESIAN_POINT('Ctrl Pts',(371.016147307277,-7.63743263312576,-3.21767489303943));
#34438=CARTESIAN_POINT('Ctrl Pts',(370.996781505073,-7.63625444010609,-3.21871079845043));
#34439=CARTESIAN_POINT('Ctrl Pts',(370.963186613776,-7.63420191680255,-3.22020388301992));
#34440=CARTESIAN_POINT('Ctrl Pts',(370.948961525339,-7.63333013111012,-3.22074168847104));
#34441=CARTESIAN_POINT('Ctrl Pts',(370.919783655442,-7.63153626076234,-3.22165126522741));
#34442=CARTESIAN_POINT('Ctrl Pts',(370.904830934777,-7.63061389047283,-3.22201321713528));
#34443=CARTESIAN_POINT('Ctrl Pts',(370.866859975986,-7.62826358734271,-3.22266791456972));
#34444=CARTESIAN_POINT('Ctrl Pts',(370.843840421863,-7.62683123769316,-3.22281813850644));
#34445=CARTESIAN_POINT('Ctrl Pts',(370.755597316853,-7.62131067278134,-3.22244859304872));
#34446=CARTESIAN_POINT('Ctrl Pts',(370.690400384602,-7.61716905993425,-3.22019543387633));
#34447=CARTESIAN_POINT('Ctrl Pts',(370.291298361409,-7.59141642045302,-3.194258793749));
#34448=CARTESIAN_POINT('Ctrl Pts',(369.962787658226,-7.56820328390233,-3.12065960283085));
#34449=CARTESIAN_POINT('Ctrl Pts',(369.608007679616,-7.54302893225164,-2.98068277514726));
#34450=CARTESIAN_POINT('Ctrl Pts',(369.564863831115,-7.53997120041452,-2.96256533731893));
#34451=CARTESIAN_POINT('Ctrl Pts',(369.493877736847,-7.53496335372641,-2.93092042130605));
#34452=CARTESIAN_POINT('Ctrl Pts',(369.465809288591,-7.53298937911568,-2.91792026868126));
#34453=CARTESIAN_POINT('Ctrl Pts',(369.427353755438,-7.5302977979533,-2.89943224299359));
#34454=CARTESIAN_POINT('Ctrl Pts',(369.416803992326,-7.52956075391121,-2.89428916460341));
#34455=CARTESIAN_POINT('Ctrl Pts',(369.399027069736,-7.52832138715674,-2.8855022837462));
#34456=CARTESIAN_POINT('Ctrl Pts',(369.391785171819,-7.52781723101786,-2.88188870896051));
#34457=CARTESIAN_POINT('Ctrl Pts',(369.377943654053,-7.52685514260679,-2.87491679602573));
#34458=CARTESIAN_POINT('Ctrl Pts',(369.371341915294,-7.52639692587111,-2.87156295416354));
#34459=CARTESIAN_POINT('Ctrl Pts',(369.355562279615,-7.525303112136,-2.86347797800529));
#34460=CARTESIAN_POINT('Ctrl Pts',(369.346395378789,-7.52466884116482,-2.85872539671211));
#34461=CARTESIAN_POINT('Ctrl Pts',(369.313383481942,-7.52238833038305,-2.84140856451865));
#34462=CARTESIAN_POINT('Ctrl Pts',(369.289672743804,-7.520757223314,-2.82858897437589));
#34463=CARTESIAN_POINT('Ctrl Pts',(369.115420176268,-7.50880040062977,-2.73153186273132));
#34464=CARTESIAN_POINT('Ctrl Pts',(368.971678985961,-7.49909736519989,-2.63561504726192));
#34465=CARTESIAN_POINT('Ctrl Pts',(368.694002091452,-7.4792875841634,-2.41620660401064));
#34466=CARTESIAN_POINT('Ctrl Pts',(368.561462072474,-7.46921219845437,-2.29197033975356));
#34467=CARTESIAN_POINT('Ctrl Pts',(368.399016158113,-7.45519289122496,-2.11167847528777));
#34468=CARTESIAN_POINT('Ctrl Pts',(368.359266765488,-7.45160885639228,-2.06494595403237));
#34469=CARTESIAN_POINT('Ctrl Pts',(368.293122554077,-7.44534598711505,-1.98252624511162));
#34470=CARTESIAN_POINT('Ctrl Pts',(368.266086228567,-7.44269224625346,-1.94737512978056));
#34471=CARTESIAN_POINT('Ctrl Pts',(368.228382321813,-7.43884737968185,-1.89620332964473));
#34472=CARTESIAN_POINT('Ctrl Pts',(368.217118842233,-7.43767938450671,-1.88062659061397));
#34473=CARTESIAN_POINT('Ctrl Pts',(368.197774577265,-7.43563880836797,-1.85336422160413));
#34474=CARTESIAN_POINT('Ctrl Pts',(368.189630389842,-7.43476868794977,-1.84172408214783));
#34475=CARTESIAN_POINT('Ctrl Pts',(368.173037068899,-7.4329728092505,-1.81767093061318));
#34476=CARTESIAN_POINT('Ctrl Pts',(368.164597206876,-7.43204672798182,-1.8052519722493));
#34477=CARTESIAN_POINT('Ctrl Pts',(368.143288198828,-7.42967572275531,-1.77342026075095));
#34478=CARTESIAN_POINT('Ctrl Pts',(368.130542319421,-7.42822622592957,-1.75392640642534));
#34479=CARTESIAN_POINT('Ctrl Pts',(368.08179318308,-7.42255752835863,-1.67757400424202));
#34480=CARTESIAN_POINT('Ctrl Pts',(368.047365227766,-7.41828118425131,-1.61973472511951));
#34481=CARTESIAN_POINT('Ctrl Pts',(367.880049433157,-7.39601259155364,-1.31749556208095));
#34482=CARTESIAN_POINT('Ctrl Pts',(367.777415490948,-7.37698557944799,-1.05773187813221));
#34483=CARTESIAN_POINT('Ctrl Pts',(367.680111915811,-7.35027017100145,-0.671907276102211));
#34484=CARTESIAN_POINT('Ctrl Pts',(367.657309979484,-7.34233413642857,-0.554167597318695));
#34485=CARTESIAN_POINT('Ctrl Pts',(367.638720169622,-7.33358130100331,-0.417837180098143));
#34486=CARTESIAN_POINT('Ctrl Pts',(367.636467811545,-7.33245947710066,-0.400234442104032));
#34487=CARTESIAN_POINT('Ctrl Pts',(367.633245482514,-7.33075561254188,-0.37328475771412));
#34488=CARTESIAN_POINT('Ctrl Pts',(367.632170838178,-7.33016799345792,-0.363951002411286));
#34489=CARTESIAN_POINT('Ctrl Pts',(367.630275959976,-7.32909515796473,-0.346834750679004));
#34490=CARTESIAN_POINT('Ctrl Pts',(367.629443251316,-7.32860927305682,-0.339053958120386));
#34491=CARTESIAN_POINT('Ctrl Pts',(367.627629655405,-7.32751736791617,-0.321503901199308));
#34492=CARTESIAN_POINT('Ctrl Pts',(367.626665065784,-7.32691226224077,-0.311733151380875));
#34493=CARTESIAN_POINT('Ctrl Pts',(367.624293843185,-7.32535870049262,-0.286536798747629));
#34494=CARTESIAN_POINT('Ctrl Pts',(367.62295372125,-7.32441382017259,-0.271104990043831));
#34495=CARTESIAN_POINT('Ctrl Pts',(367.615011734892,-7.31834262474473,-0.171308412292787));
#34496=CARTESIAN_POINT('Ctrl Pts',(367.611623045353,-7.31337726984258,-0.0867134915978316));
#34497=CARTESIAN_POINT('Ctrl Pts',(367.611398677425,-7.29332513466613,0.261575697431371));
#34498=CARTESIAN_POINT('Ctrl Pts',(367.643581452442,-7.27904210008449,0.524258573570218));
#34499=CARTESIAN_POINT('Ctrl Pts',(367.733961813044,-7.25763832999817,0.886534589102296));
#34500=CARTESIAN_POINT('Ctrl Pts',(367.765929793215,-7.25123338405258,0.991535287627039));
#34501=CARTESIAN_POINT('Ctrl Pts',(367.812416071019,-7.24302267440763,1.12025245319812));
#34502=CARTESIAN_POINT('Ctrl Pts',(367.821968802864,-7.24138217694595,1.14569152500224));
#34503=CARTESIAN_POINT('Ctrl Pts',(367.837662172459,-7.23875760046087,1.18592954094534));
#34504=CARTESIAN_POINT('Ctrl Pts',(367.843593580217,-7.23778053325284,1.2008090828753));
#34505=CARTESIAN_POINT('Ctrl Pts',(367.854900349201,-7.23594509224851,1.22856977968898));
#34506=CARTESIAN_POINT('Ctrl Pts',(367.860248963296,-7.2350876387046,1.24146147547367));
#34507=CARTESIAN_POINT('Ctrl Pts',(367.872397832818,-7.23316358341588,1.27021461839161));
#34508=CARTESIAN_POINT('Ctrl Pts',(367.879242053537,-7.23209550602635,1.28605691305561));
#34509=CARTESIAN_POINT('Ctrl Pts',(367.89986559245,-7.22892274708251,1.33276019660347));
#34510=CARTESIAN_POINT('Ctrl Pts',(367.914003165366,-7.22680588802463,1.36345949577465));
#34511=CARTESIAN_POINT('Ctrl Pts',(367.947318411436,-7.22194373666216,1.43290633405652));
#34512=CARTESIAN_POINT('Ctrl Pts',(367.966797900388,-7.21918844284527,1.47150106144193));
#34513=CARTESIAN_POINT('Ctrl Pts',(368.034988357602,-7.20982476546895,1.6001079828204));
#34514=CARTESIAN_POINT('Ctrl Pts',(368.087205169262,-7.2031030347132,1.68818240651719));
#34515=CARTESIAN_POINT('Ctrl Pts',(368.262551758136,-7.18187098121895,1.95420506679225));
#34516=CARTESIAN_POINT('Ctrl Pts',(368.399454113501,-7.16703821124287,2.12234092774425));
#34517=CARTESIAN_POINT('Ctrl Pts',(368.612262213029,-7.14700621075816,2.33577226344528));
#34518=CARTESIAN_POINT('Ctrl Pts',(368.674734942209,-7.14143370600362,2.393651529463));
#34519=CARTESIAN_POINT('Ctrl Pts',(368.751220366321,-7.1350349565875,2.45907768911558));
#34520=CARTESIAN_POINT('Ctrl Pts',(368.763081882362,-7.13405413794183,2.46907670925603));
#34521=CARTESIAN_POINT('Ctrl Pts',(368.782573159931,-7.1324617668334,2.48526815695573));
#34522=CARTESIAN_POINT('Ctrl Pts',(368.790159701091,-7.13184669449722,2.49151190113257));
#34523=CARTESIAN_POINT('Ctrl Pts',(368.80383982628,-7.13074622739279,2.50266613516056));
#34524=CARTESIAN_POINT('Ctrl Pts',(368.809922825616,-7.13025994572069,2.50758919640876));
#34525=CARTESIAN_POINT('Ctrl Pts',(368.823343735524,-7.12919376210525,2.5183702696963));
#34526=CARTESIAN_POINT('Ctrl Pts',(368.830689332612,-7.12861455975534,2.52421838871857));
#34527=CARTESIAN_POINT('Ctrl Pts',(368.851968703662,-7.12694883614547,2.54100831892204));
#34528=CARTESIAN_POINT('Ctrl Pts',(368.865967529408,-7.12586796980399,2.55186764210009));
#34529=CARTESIAN_POINT('Ctrl Pts',(368.974486765301,-7.11759729905259,2.63462504487918));
#34530=CARTESIAN_POINT('Ctrl Pts',(369.072837534192,-7.11072753403957,2.70137266597804));
#34531=CARTESIAN_POINT('Ctrl Pts',(369.401727301336,-7.08894275969346,2.89896034947317));
#34532=CARTESIAN_POINT('Ctrl Pts',(369.644739486146,-7.07452662493812,3.00685783437668));
#34533=CARTESIAN_POINT('Ctrl Pts',(369.973626959232,-7.05455706417947,3.10669258537339));
#34534=CARTESIAN_POINT('Ctrl Pts',(370.049842495721,-7.04990751279688,3.12680740869598));
#34535=CARTESIAN_POINT('Ctrl Pts',(370.150781871333,-7.04368448810621,3.14952452084542));
#34536=CARTESIAN_POINT('Ctrl Pts',(370.174910237852,-7.0421922091585,3.15466443399327));
#34537=CARTESIAN_POINT('Ctrl Pts',(370.214109418506,-7.0397591711853,3.16254543260609));
#34538=CARTESIAN_POINT('Ctrl Pts',(370.229145221786,-7.03882386606374,3.16545702691748));
#34539=CARTESIAN_POINT('Ctrl Pts',(370.258053162049,-7.03702146179978,3.17084138790783));
#34540=CARTESIAN_POINT('Ctrl Pts',(370.271921911155,-7.03615490780868,3.17333056832926));
#34541=CARTESIAN_POINT('Ctrl Pts',(370.304009206815,-7.03414556912704,3.17887268228503));
#34542=CARTESIAN_POINT('Ctrl Pts',(370.322238431475,-7.03300073368005,3.18186005878463));
#34543=CARTESIAN_POINT('Ctrl Pts',(370.380127875912,-7.02935418407008,3.19083653620975));
#34544=CARTESIAN_POINT('Ctrl Pts',(370.419873484355,-7.0268342094576,3.1962418507338));
#34545=CARTESIAN_POINT('Ctrl Pts',(370.624903415305,-7.01374565902768,3.22023700644114));
#34546=CARTESIAN_POINT('Ctrl Pts',(370.791323285555,-7.00280570432569,3.2267503742865));
#34547=CARTESIAN_POINT('Ctrl Pts',(371.094498413275,-6.98244568196471,3.21515547391714));
#34548=CARTESIAN_POINT('Ctrl Pts',(371.231040246453,-6.97312078503562,3.20117615178233));
#34549=CARTESIAN_POINT('Ctrl Pts',(371.495712460876,-6.95505694371268,3.15688118846149));
#34550=CARTESIAN_POINT('Ctrl Pts',(371.623723969885,-6.9463279985614,3.12732909856004));
#34551=CARTESIAN_POINT('Ctrl Pts',(371.76572018431,-6.93689701975914,3.08526989477441));
#34552=CARTESIAN_POINT('Ctrl Pts',(371.78181463671,-6.93583187166918,3.08036531912207));
#34553=CARTESIAN_POINT('Ctrl Pts',(371.807516755451,-6.93413779228415,3.07231242672921));
#34554=CARTESIAN_POINT('Ctrl Pts',(371.817149056633,-6.93350447064289,3.06924462739969));
#34555=CARTESIAN_POINT('Ctrl Pts',(371.834245375026,-6.93238337401258,3.06371087090298));
#34556=CARTESIAN_POINT('Ctrl Pts',(371.841714999078,-6.93189457627174,3.06126286761943));
#34557=CARTESIAN_POINT('Ctrl Pts',(371.857770834179,-6.93084616677663,3.05593579192734));
#34558=CARTESIAN_POINT('Ctrl Pts',(371.866353897612,-6.93028707934126,3.05304785032756));
#34559=CARTESIAN_POINT('Ctrl Pts',(371.890217403953,-6.92873616194583,3.04490636735421));
#34560=CARTESIAN_POINT('Ctrl Pts',(371.905470921954,-6.92774884187755,3.0395739463662));
#34561=CARTESIAN_POINT('Ctrl Pts',(371.995615437618,-6.9219343370987,3.00729778987409));
#34562=CARTESIAN_POINT('Ctrl Pts',(372.069533992445,-6.91724962241963,2.97769968093071));
#34563=CARTESIAN_POINT('Ctrl Pts',(372.198919375538,-6.90907263694122,2.92024313659028));
#34564=CARTESIAN_POINT('Ctrl Pts',(372.254786456931,-6.90554985179344,2.89347862523926));
#34565=CARTESIAN_POINT('Ctrl Pts',(372.309820841127,-6.90205582396876,2.86513673237218));
#34566=CARTESIAN_POINT('',(367.611569021564,-7.06162094379804,-0.00160891364598954));
#34567=CARTESIAN_POINT('Ctrl Pts',(372.309820613387,-6.65415806382428,2.86513684965516));
#34568=CARTESIAN_POINT('Ctrl Pts',(372.292714814035,-6.65536004592608,2.87394608128435));
#34569=CARTESIAN_POINT('Ctrl Pts',(372.275530545294,-6.65656739170384,2.8826019051552));
#34570=CARTESIAN_POINT('Ctrl Pts',(372.050564813285,-6.67237282628404,2.99340403598632));
#34571=CARTESIAN_POINT('Ctrl Pts',(371.832478903887,-6.68776556693163,3.07300526760262));
#34572=CARTESIAN_POINT('Ctrl Pts',(371.409105348385,-6.71724093813562,3.17767631938501));
#34573=CARTESIAN_POINT('Ctrl Pts',(371.206174504654,-6.73118248846332,3.20776299651676));
#34574=CARTESIAN_POINT('Ctrl Pts',(370.975790578942,-6.74599160673359,3.21974822736512));
#34575=CARTESIAN_POINT('Ctrl Pts',(370.949816687413,-6.74764624100932,3.22078457808238));
#34576=CARTESIAN_POINT('Ctrl Pts',(370.913653238748,-6.74992655959511,3.22178943285873));
#34577=CARTESIAN_POINT('Ctrl Pts',(370.903472865778,-6.75056590929184,3.22202402906313));
#34578=CARTESIAN_POINT('Ctrl Pts',(370.885921488494,-6.75166352459439,3.22234525788378));
#34579=CARTESIAN_POINT('Ctrl Pts',(370.878551055494,-6.75212303827263,3.22245485966527));
#34580=CARTESIAN_POINT('Ctrl Pts',(370.863042820153,-6.75308684240395,3.22263225714373));
#34581=CARTESIAN_POINT('Ctrl Pts',(370.854905031971,-6.75359080547268,3.22269451837233));
#34582=CARTESIAN_POINT('Ctrl Pts',(370.834828492493,-6.7548299083099,3.22277207267103));
#34583=CARTESIAN_POINT('Ctrl Pts',(370.822889580034,-6.75556309208547,3.22275185177327));
#34584=CARTESIAN_POINT('Ctrl Pts',(370.778670236786,-6.75826595864589,3.22243122460895));
#34585=CARTESIAN_POINT('Ctrl Pts',(370.746393564111,-6.76021377567416,3.22171214651434));
#34586=CARTESIAN_POINT('Ctrl Pts',(370.51164755989,-6.77423279404112,3.21295166462082));
#34587=CARTESIAN_POINT('Ctrl Pts',(370.310301049912,-6.78547882240443,3.18631470827144));
#34588=CARTESIAN_POINT('Ctrl Pts',(369.908343296722,-6.80854281449839,3.09397552209954));
#34589=CARTESIAN_POINT('Ctrl Pts',(369.709013461959,-6.82032748692682,3.0271752803054));
#34590=CARTESIAN_POINT('Ctrl Pts',(369.479312238753,-6.83526531066406,2.92435235518205));
#34591=CARTESIAN_POINT('Ctrl Pts',(369.441367910337,-6.83777827620923,2.90646987339364));
#34592=CARTESIAN_POINT('Ctrl Pts',(369.3871098529,-6.84144283512145,2.87959247882223));
#34593=CARTESIAN_POINT('Ctrl Pts',(369.370507182731,-6.84257395538906,2.87118827991933));
#34594=CARTESIAN_POINT('Ctrl Pts',(369.34139340426,-6.84457518527662,2.85613285602634));
#34595=CARTESIAN_POINT('Ctrl Pts',(369.328851532944,-6.84544315654891,2.84954197196294));
#34596=CARTESIAN_POINT('Ctrl Pts',(369.31482980478,-6.84642025051363,2.84205499901586));
#34597=CARTESIAN_POINT('Ctrl Pts',(369.313306580803,-6.8465264844598,2.84124009121787));
#34598=CARTESIAN_POINT('Ctrl Pts',(369.298320249221,-6.84757255336302,2.83320706612694));
#34599=CARTESIAN_POINT('Ctrl Pts',(369.284908155408,-6.84851573178744,2.82589463613572));
#34600=CARTESIAN_POINT('Ctrl Pts',(369.257497529659,-6.85045793605267,2.81069624214544));
#34601=CARTESIAN_POINT('Ctrl Pts',(369.243504988307,-6.85145729699466,2.80280040534842));
#34602=CARTESIAN_POINT('Ctrl Pts',(369.208866699075,-6.85395117135782,2.78291145661275));
#34603=CARTESIAN_POINT('Ctrl Pts',(369.188294347554,-6.85545015644211,2.77079306326534));
#34604=CARTESIAN_POINT('Ctrl Pts',(369.130792736727,-6.85969106238078,2.73605465662089));
#34605=CARTESIAN_POINT('Ctrl Pts',(369.094183110506,-6.86245134426193,2.71291793037405));
#34606=CARTESIAN_POINT('Ctrl Pts',(368.972455356669,-6.87183626518595,2.63251008330424));
#34607=CARTESIAN_POINT('Ctrl Pts',(368.889614430949,-6.87857478917699,2.57191886111249));
#34608=CARTESIAN_POINT('Ctrl Pts',(368.635864483499,-6.90031020789244,2.36704475180542));
#34609=CARTESIAN_POINT('Ctrl Pts',(368.477014553453,-6.91565888791342,2.20889417015381));
#34610=CARTESIAN_POINT('Ctrl Pts',(368.286472538878,-6.9356530371954,1.97502003431186));
#34611=CARTESIAN_POINT('Ctrl Pts',(368.239345180718,-6.94075329982927,1.91267844525905));
#34612=CARTESIAN_POINT('Ctrl Pts',(368.18498718465,-6.94677476770478,1.8350588872182));
#34613=CARTESIAN_POINT('Ctrl Pts',(368.175553126101,-6.94782524413817,1.82136329826252));
#34614=CARTESIAN_POINT('Ctrl Pts',(368.161029669103,-6.9494501941447,1.79992601353452));
#34615=CARTESIAN_POINT('Ctrl Pts',(368.155867077405,-6.95002937441498,1.79223458735709));
#34616=CARTESIAN_POINT('Ctrl Pts',(368.146395881394,-6.9510946786067,1.77799170893899));
#34617=CARTESIAN_POINT('Ctrl Pts',(368.142078033952,-6.95158139943007,1.77144681018766));
#34618=CARTESIAN_POINT('Ctrl Pts',(368.132308237288,-6.95268515688996,1.75651973397462));
#34619=CARTESIAN_POINT('Ctrl Pts',(368.126871385587,-6.95330119238561,1.74812790480814));
#34620=CARTESIAN_POINT('Ctrl Pts',(368.110298055638,-6.95518507856482,1.72228403259902));
#34621=CARTESIAN_POINT('Ctrl Pts',(368.099290363321,-6.95644476499212,1.70474949094696));
#34622=CARTESIAN_POINT('Ctrl Pts',(368.074011026351,-6.95936063101553,1.66360594754182));
#34623=CARTESIAN_POINT('Ctrl Pts',(368.059871843923,-6.96100929032781,1.63991706274016));
#34624=CARTESIAN_POINT('Ctrl Pts',(368.011309865285,-6.96674596015214,1.55612975027016));
#34625=CARTESIAN_POINT('Ctrl Pts',(367.978519915078,-6.97075585652661,1.49510307797678));
#34626=CARTESIAN_POINT('Ctrl Pts',(367.823527142657,-6.99066965287483,1.18290356230497));
#34627=CARTESIAN_POINT('Ctrl Pts',(367.732379285683,-7.00579167713607,0.917665187718701));
#34628=CARTESIAN_POINT('Ctrl Pts',(367.660375132727,-7.02670475077214,0.564597279851319));
#34629=CARTESIAN_POINT('Ctrl Pts',(367.647185239816,-7.03148147685216,0.484630364062586));
#34630=CARTESIAN_POINT('Ctrl Pts',(367.633895666356,-7.03785220601611,0.379521983584453));
#34631=CARTESIAN_POINT('Ctrl Pts',(367.631055567865,-7.03936002166402,0.354753136926414));
#34632=CARTESIAN_POINT('Ctrl Pts',(367.626928570105,-7.04181259935233,0.314655499392359));
#34633=CARTESIAN_POINT('Ctrl Pts',(367.625463511737,-7.04275174832619,0.299345785059292));
#34634=CARTESIAN_POINT('Ctrl Pts',(367.622915484472,-7.04452374600888,0.270546692274248));
#34635=CARTESIAN_POINT('Ctrl Pts',(367.621807785001,-7.04535579774585,0.257059797362288));
#34636=CARTESIAN_POINT('Ctrl Pts',(367.619753967572,-7.04703210872499,0.229962433911934));
#34637=CARTESIAN_POINT('Ctrl Pts',(367.618809271689,-7.04787639473124,0.216352140870095));
#34638=CARTESIAN_POINT('Ctrl Pts',(367.616844520928,-7.04981543936561,0.185181821329923));
#34639=CARTESIAN_POINT('Ctrl Pts',(367.615881759504,-7.05091196771938,0.167618739758486));
#34640=CARTESIAN_POINT('Ctrl Pts',(367.612708007927,-7.05517899842007,0.0995268477100366));
#34641=CARTESIAN_POINT('Ctrl Pts',(367.611542957261,-7.05838171058188,0.04895922325798));
#34642=CARTESIAN_POINT('Ctrl Pts',(367.611568256498,-7.06161982618061,-0.00161223563090186));
#34643=CARTESIAN_POINT('Ctrl Pts',(367.611568254881,-7.06161961892771,-0.00160899884609024));
#34644=CARTESIAN_POINT('Ctrl Pts',(367.611737235074,-7.08329133490289,-0.340068440858395));
#34645=CARTESIAN_POINT('Ctrl Pts',(367.665231320938,-7.10671891120355,-0.67639080493669));
#34646=CARTESIAN_POINT('Ctrl Pts',(367.794381854883,-7.13434941397816,-1.07288818642694));
#34647=CARTESIAN_POINT('Ctrl Pts',(367.821464099035,-7.13948047276956,-1.14674076032872));
#34648=CARTESIAN_POINT('Ctrl Pts',(367.857320765052,-7.14549618592994,-1.23444948557229));
#34649=CARTESIAN_POINT('Ctrl Pts',(367.863530123105,-7.14651325527707,-1.24931880762661));
#34650=CARTESIAN_POINT('Ctrl Pts',(367.8734008267,-7.14809148099084,-1.27246604203168));
#34651=CARTESIAN_POINT('Ctrl Pts',(367.876985863791,-7.14865704107256,-1.28077592695885));
#34652=CARTESIAN_POINT('Ctrl Pts',(367.883753324101,-7.14971033106886,-1.29628254583913));
#34653=CARTESIAN_POINT('Ctrl Pts',(367.886927075202,-7.15019854408521,-1.30348267434354));
#34654=CARTESIAN_POINT('Ctrl Pts',(367.894249632532,-7.15131199810259,-1.31993149996014));
#34655=CARTESIAN_POINT('Ctrl Pts',(367.898415726098,-7.15193617807314,-1.32917230385051));
#34656=CARTESIAN_POINT('Ctrl Pts',(367.909646272212,-7.15359460698061,-1.35377232508654));
#34657=CARTESIAN_POINT('Ctrl Pts',(367.916788202708,-7.15462432127332,-1.36909610005323));
#34658=CARTESIAN_POINT('Ctrl Pts',(367.982869881789,-7.16393506312115,-1.50801580729049));
#34659=CARTESIAN_POINT('Ctrl Pts',(368.049517702996,-7.17179105464176,-1.62780971233834));
#34660=CARTESIAN_POINT('Ctrl Pts',(368.240898971664,-7.19176483792071,-1.92544500554169));
#34661=CARTESIAN_POINT('Ctrl Pts',(368.376317251127,-7.20367490969703,-2.095565052367));
#34662=CARTESIAN_POINT('Ctrl Pts',(368.575855084087,-7.22009998685957,-2.30004315068532));
#34663=CARTESIAN_POINT('Ctrl Pts',(368.625476020897,-7.224103682233,-2.3477370922521));
#34664=CARTESIAN_POINT('Ctrl Pts',(368.701085346637,-7.23012079500241,-2.41589005770033));
#34665=CARTESIAN_POINT('Ctrl Pts',(368.72592442422,-7.23208484004625,-2.4375977377705));
#34666=CARTESIAN_POINT('Ctrl Pts',(368.766204957531,-7.23525280248554,-2.47172388618119));
#34667=CARTESIAN_POINT('Ctrl Pts',(368.781435678765,-7.23644686178719,-2.48438818831003));
#34668=CARTESIAN_POINT('Ctrl Pts',(368.810790446389,-7.23874165976861,-2.50834234283804));
#34669=CARTESIAN_POINT('Ctrl Pts',(368.824894691603,-7.23984141744036,-2.51965533594577));
#34670=CARTESIAN_POINT('Ctrl Pts',(368.849739001197,-7.24177407751539,-2.53924164170816));
#34671=CARTESIAN_POINT('Ctrl Pts',(368.860437554667,-7.24260487805318,-2.54756705368057));
#34672=CARTESIAN_POINT('Ctrl Pts',(368.881818160794,-7.24426249275967,-2.56398950372236));
#34673=CARTESIAN_POINT('Ctrl Pts',(368.89249883648,-7.24508923036988,-2.57208789151719));
#34674=CARTESIAN_POINT('Ctrl Pts',(368.921388769529,-7.24732209474109,-2.59371053901141));
#34675=CARTESIAN_POINT('Ctrl Pts',(368.939690538482,-7.24873306062043,-2.60710938309576));
#34676=CARTESIAN_POINT('Ctrl Pts',(369.009121902536,-7.2540735659085,-2.65682333749758));
#34677=CARTESIAN_POINT('Ctrl Pts',(369.061163675774,-7.25805213216131,-2.69183466965255));
#34678=CARTESIAN_POINT('Ctrl Pts',(369.399822900707,-7.28380437890523,-2.9055858410807));
#34679=CARTESIAN_POINT('Ctrl Pts',(369.711936760824,-7.30723037477153,-3.03979988864536));
#34680=CARTESIAN_POINT('Ctrl Pts',(370.084600425111,-7.33261541774669,-3.13468364931452));
#34681=CARTESIAN_POINT('Ctrl Pts',(370.130306544316,-7.33568132364134,-3.14526411090766));
#34682=CARTESIAN_POINT('Ctrl Pts',(370.206570090419,-7.34070136474734,-3.16117239510582));
#34683=CARTESIAN_POINT('Ctrl Pts',(370.237001664605,-7.34267948751487,-3.16706357708475));
#34684=CARTESIAN_POINT('Ctrl Pts',(370.279082600522,-7.34537606724552,-3.17458177761866));
#34685=CARTESIAN_POINT('Ctrl Pts',(370.290661864862,-7.34611404392689,-3.17658524598284));
#34686=CARTESIAN_POINT('Ctrl Pts',(370.3102412994,-7.34735479017406,-3.17986272424727));
#34687=CARTESIAN_POINT('Ctrl Pts',(370.318235720087,-7.34785939882693,-3.1811699760106));
#34688=CARTESIAN_POINT('Ctrl Pts',(370.333551738313,-7.34882222094985,-3.18361520250084));
#34689=CARTESIAN_POINT('Ctrl Pts',(370.340872420381,-7.34928072016564,-3.1847580860805));
#34690=CARTESIAN_POINT('Ctrl Pts',(370.358408300754,-7.3503750613516,-3.18743382007305));
#34691=CARTESIAN_POINT('Ctrl Pts',(370.368627129046,-7.35100957689574,-3.18894283668358));
#34692=CARTESIAN_POINT('Ctrl Pts',(370.405528348079,-7.35328991282478,-3.19421088668329));
#34693=CARTESIAN_POINT('Ctrl Pts',(370.432251203193,-7.35492061160393,-3.19768449740244));
#34694=CARTESIAN_POINT('Ctrl Pts',(370.62542270702,-7.36657985750924,-3.22033421450083));
#34695=CARTESIAN_POINT('Ctrl Pts',(370.793119564321,-7.3760217122969,-3.22684149060996));
#34696=CARTESIAN_POINT('Ctrl Pts',(371.116654714395,-7.39415431732153,-3.21415627551405));
#34697=CARTESIAN_POINT('Ctrl Pts',(371.272076725129,-7.40283116220469,-3.1966982529753));
#34698=CARTESIAN_POINT('Ctrl Pts',(371.54265045725,-7.41856434178197,-3.14619724817188));
#34699=CARTESIAN_POINT('Ctrl Pts',(371.658374907922,-7.42550054096438,-3.11788672454404));
#34700=CARTESIAN_POINT('Ctrl Pts',(371.798174858124,-7.43427057135227,-3.07535867146352));
#34701=CARTESIAN_POINT('Ctrl Pts',(371.823988540252,-7.43590643892557,-3.06714902593804));
#34702=CARTESIAN_POINT('Ctrl Pts',(371.864738992345,-7.43851648187748,-3.05362098161577));
#34703=CARTESIAN_POINT('Ctrl Pts',(371.879745632013,-7.43948363320663,-3.04851596167851));
#34704=CARTESIAN_POINT('Ctrl Pts',(371.907923194807,-7.44131118832227,-3.03869787993647));
#34705=CARTESIAN_POINT('Ctrl Pts',(371.921102320756,-7.44217076192382,-3.03400935172418));
#34706=CARTESIAN_POINT('Ctrl Pts',(371.950726227592,-7.44411392166302,-3.02325274316792));
#34707=CARTESIAN_POINT('Ctrl Pts',(371.967152763123,-7.44519910747048,-3.0171360352015));
#34708=CARTESIAN_POINT('Ctrl Pts',(372.009152308528,-7.44799388415985,-3.00110543094856));
#34709=CARTESIAN_POINT('Ctrl Pts',(372.034649731752,-7.44970987639238,-2.99099868133295));
#34710=CARTESIAN_POINT('Ctrl Pts',(372.254765927177,-7.4646956437799,-2.90048047448044));
#34711=CARTESIAN_POINT('Ctrl Pts',(372.441164298007,-7.47861007205944,-2.80151302856067));
#34712=CARTESIAN_POINT('Ctrl Pts',(372.760639029563,-7.50446409931744,-2.58946167500162));
#34713=CARTESIAN_POINT('Ctrl Pts',(372.896796432942,-7.5162577173633,-2.48237995002616));
#34714=CARTESIAN_POINT('Ctrl Pts',(373.058918865243,-7.53085261190641,-2.33228868700919));
#34715=CARTESIAN_POINT('Ctrl Pts',(373.093400608728,-7.53399115836358,-2.29890533956787));
#34716=CARTESIAN_POINT('Ctrl Pts',(373.149274510799,-7.53911671423045,-2.24233953918816));
#34717=CARTESIAN_POINT('Ctrl Pts',(373.171094265287,-7.54112893030326,-2.2195916536104));
#34718=CARTESIAN_POINT('Ctrl Pts',(373.20063938389,-7.54386381452045,-2.18787108403626));
#34719=CARTESIAN_POINT('Ctrl Pts',(373.208653498791,-7.54460671514471,-2.17917133775323));
#34720=CARTESIAN_POINT('Ctrl Pts',(373.222085350019,-7.54585333557096,-2.16442828662905));
#34721=CARTESIAN_POINT('Ctrl Pts',(373.22752843721,-7.54635893341554,-2.15840833309759));
#34722=CARTESIAN_POINT('Ctrl Pts',(373.237886453824,-7.54732176987865,-2.14686520372296));
#34723=CARTESIAN_POINT('Ctrl Pts',(373.242805183746,-7.54777930664708,-2.14134560546803));
#34724=CARTESIAN_POINT('Ctrl Pts',(373.254509705343,-7.54886894217175,-2.12811991891983));
#34725=CARTESIAN_POINT('Ctrl Pts',(373.261277797574,-7.54949974026796,-2.12039817617203));
#34726=CARTESIAN_POINT('Ctrl Pts',(373.285392543592,-7.55175043150226,-2.09261884345245));
#34727=CARTESIAN_POINT('Ctrl Pts',(373.302528925134,-7.55335571976284,-2.072379060183));
#34728=CARTESIAN_POINT('Ctrl Pts',(373.441774012092,-7.56647131394683,-1.90373901782998));
#34729=CARTESIAN_POINT('Ctrl Pts',(373.550650052763,-7.5772031526525,-1.74488064433265));
#34730=CARTESIAN_POINT('Ctrl Pts',(373.682595817303,-7.5922785978866,-1.509773784623));
#34731=CARTESIAN_POINT('Ctrl Pts',(373.718020701275,-7.59660055451943,-1.44095866765114));
#34732=CARTESIAN_POINT('Ctrl Pts',(373.816689762544,-7.60966616493837,-1.23104387852857));
#34733=CARTESIAN_POINT('Ctrl Pts',(373.87228856369,-7.61851166975053,-1.08661736524141));
#34734=CARTESIAN_POINT('Ctrl Pts',(373.92858184387,-7.63000758238224,-0.901745947322941));
#34735=CARTESIAN_POINT('Ctrl Pts',(373.93918726849,-7.63232986865382,-0.864523636628074));
#34736=CARTESIAN_POINT('Ctrl Pts',(373.953795578101,-7.63577729023261,-0.809511114016146));
#34737=CARTESIAN_POINT('Ctrl Pts',(373.958322180466,-7.6368855220434,-0.791862653459371));
#34738=CARTESIAN_POINT('Ctrl Pts',(373.966077516124,-7.63885784522248,-0.760524027585623));
#34739=CARTESIAN_POINT('Ctrl Pts',(373.969366754259,-7.6397199634918,-0.746849222345889));
#34740=CARTESIAN_POINT('Ctrl Pts',(373.976082010248,-7.64153543839229,-0.718104706916323));
#34741=CARTESIAN_POINT('Ctrl Pts',(373.979489347771,-7.64248937039048,-0.703031041324144));
#34742=CARTESIAN_POINT('Ctrl Pts',(373.988182371304,-7.64501243310841,-0.663245626646811));
#34743=CARTESIAN_POINT('Ctrl Pts',(373.993285957855,-7.64658733235627,-0.638495587424803));
#34744=CARTESIAN_POINT('Ctrl Pts',(374.014089557158,-7.65343636603863,-0.53124574344785));
#34745=CARTESIAN_POINT('Ctrl Pts',(374.026851399402,-7.65880232043154,-0.448216028682624));
#34746=CARTESIAN_POINT('Ctrl Pts',(374.06256070805,-7.67930581152035,-0.134767092402776));
#34747=CARTESIAN_POINT('Ctrl Pts',(374.063900551766,-7.6950498575698,0.0973863939785096));
#34748=CARTESIAN_POINT('Ctrl Pts',(374.025652589839,-7.72042561626714,0.471652412540713));
#34749=CARTESIAN_POINT('Ctrl Pts',(374.001247125828,-7.73009142531755,0.6145257545992));
#34750=CARTESIAN_POINT('Ctrl Pts',(373.9630248196,-7.7404730992766,0.773075075186207));
#34751=CARTESIAN_POINT('Ctrl Pts',(373.958585120696,-7.74163037428862,0.790826422800244));
#34752=CARTESIAN_POINT('Ctrl Pts',(373.951607259095,-7.7433768912815,0.817749871478434));
#34753=CARTESIAN_POINT('Ctrl Pts',(373.949179347836,-7.74397213319706,0.826949797206087));
#34754=CARTESIAN_POINT('Ctrl Pts',(373.944679904098,-7.74505276218778,0.843698252808411));
#34755=CARTESIAN_POINT('Ctrl Pts',(373.942621608022,-7.74553887658771,0.851250022073007));
#34756=CARTESIAN_POINT('Ctrl Pts',(373.937950882415,-7.74662383152421,0.868143809570159));
#34757=CARTESIAN_POINT('Ctrl Pts',(373.9353237814,-7.74722181823945,0.877481562834963));
#34758=CARTESIAN_POINT('Ctrl Pts',(373.927534240669,-7.74896007427734,0.90469673740681));
#34759=CARTESIAN_POINT('Ctrl Pts',(373.922258984267,-7.75009405373213,0.922541822769922));
#34760=CARTESIAN_POINT('Ctrl Pts',(373.870635078861,-7.76080123712691,1.09176908423008));
#34761=CARTESIAN_POINT('Ctrl Pts',(373.813338724544,-7.76980570429237,1.23960874869254));
#34762=CARTESIAN_POINT('Ctrl Pts',(373.686695191316,-7.78638916741775,1.50624791177519));
#34763=CARTESIAN_POINT('Ctrl Pts',(373.620181426628,-7.79397935946015,1.62597764351755));
#34764=CARTESIAN_POINT('Ctrl Pts',(373.468722904602,-7.80981707124958,1.86188747062503));
#34765=CARTESIAN_POINT('Ctrl Pts',(373.383213883506,-7.8180625026075,1.97733083356222));
#34766=CARTESIAN_POINT('Ctrl Pts',(373.266154626798,-7.82882769092561,2.11510720020611));
#34767=CARTESIAN_POINT('Ctrl Pts',(373.241515159255,-7.831067186585,2.14310744436421));
#34768=CARTESIAN_POINT('Ctrl Pts',(373.204303590403,-7.83441453951614,2.1839431066735));
#34769=CARTESIAN_POINT('Ctrl Pts',(373.192100642457,-7.83550689776189,2.19711178280888));
#34770=CARTESIAN_POINT('Ctrl Pts',(373.170165168159,-7.83746140903825,2.22039000746612));
#34771=CARTESIAN_POINT('Ctrl Pts',(373.160475373136,-7.83832171567159,2.2305393174434));
#34772=CARTESIAN_POINT('Ctrl Pts',(373.139877645865,-7.84014421114563,2.25183365102323));
#34773=CARTESIAN_POINT('Ctrl Pts',(373.128954509048,-7.84110705206922,2.26296340081473));
#34774=CARTESIAN_POINT('Ctrl Pts',(373.099667329586,-7.84367928483321,2.29237447748929));
#34775=CARTESIAN_POINT('Ctrl Pts',(373.081163147025,-7.84529485629347,2.31051404622877));
#34776=CARTESIAN_POINT('Ctrl Pts',(372.997142582082,-7.85258959482103,2.39091520004956));
#34777=CARTESIAN_POINT('Ctrl Pts',(372.929248543643,-7.858376075824,2.45062219217586));
#34778=CARTESIAN_POINT('Ctrl Pts',(372.688450949868,-7.87854936501975,2.64505690195918));
#34779=CARTESIAN_POINT('Ctrl Pts',(372.504442393296,-7.89343311657087,2.76490953516983));
#34780=CARTESIAN_POINT('Ctrl Pts',(372.309820607824,-7.90820793933161,2.86513685252006));
#34781=CARTESIAN_POINT('Origin',(370.834317853224,2.31077344927308,0.));
#34782=CARTESIAN_POINT('',(372.309820613643,-9.40650395364997,2.86513684952317));
#34783=CARTESIAN_POINT('',(372.309820498245,-9.15921048455973,2.86513690895124));
#34784=CARTESIAN_POINT('',(372.309820613641,2.31077344927308,2.86513684952399));
#34785=CARTESIAN_POINT('',(367.611569014087,-8.55988254489073,0.00273538678758171));
#34786=CARTESIAN_POINT('Ctrl Pts',(372.309820613642,-9.40650395365004,2.86513684952373));
#34787=CARTESIAN_POINT('Ctrl Pts',(372.310235252672,-9.40647438359926,2.86492331660494));
#34788=CARTESIAN_POINT('Ctrl Pts',(372.310649845599,-9.40644481045213,2.86470969354901));
#34789=CARTESIAN_POINT('Ctrl Pts',(372.460746735871,-9.39573600244663,2.78732956637538));
#34790=CARTESIAN_POINT('Ctrl Pts',(372.604128589944,-9.38465237160275,2.69856113744389));
#34791=CARTESIAN_POINT('Ctrl Pts',(372.804867072,-9.36794059467473,2.55138049742846));
#34792=CARTESIAN_POINT('Ctrl Pts',(372.868021324973,-9.36249139473812,2.50133091792677));
#34793=CARTESIAN_POINT('Ctrl Pts',(372.947463023267,-9.35541891085743,2.4333743217127));
#34794=CARTESIAN_POINT('Ctrl Pts',(372.965518642425,-9.35379618144939,2.41757653467915));
#34795=CARTESIAN_POINT('Ctrl Pts',(373.103615286895,-9.34127317902388,2.29399927014254));
#34796=CARTESIAN_POINT('Ctrl Pts',(373.215601010952,-9.33044557639409,2.17753203008764));
#34797=CARTESIAN_POINT('Ctrl Pts',(373.329134174731,-9.31909655968901,2.04016981703633));
#34798=CARTESIAN_POINT('Ctrl Pts',(373.3397649326,-9.31803000775799,2.02710047135573));
#34799=CARTESIAN_POINT('Ctrl Pts',(373.356614109945,-9.31633413346828,2.00605121382949));
#34800=CARTESIAN_POINT('Ctrl Pts',(373.362898129198,-9.3157004064943,1.99812453906841));
#34801=CARTESIAN_POINT('Ctrl Pts',(373.37399938043,-9.31457885958607,1.98398515636269));
#34802=CARTESIAN_POINT('Ctrl Pts',(373.37883132897,-9.31409001382978,1.97778424931847));
#34803=CARTESIAN_POINT('Ctrl Pts',(373.389178127794,-9.31304180923482,1.96440537333118));
#34804=CARTESIAN_POINT('Ctrl Pts',(373.394685447933,-9.31248297245838,1.95722182646843));
#34805=CARTESIAN_POINT('Ctrl Pts',(373.409927854732,-9.31093346841135,1.9371657517056));
#34806=CARTESIAN_POINT('Ctrl Pts',(373.419596775547,-9.30994729767633,1.92424295452978));
#34807=CARTESIAN_POINT('Ctrl Pts',(373.476162334993,-9.30415496411573,1.84744538910572));
#34808=CARTESIAN_POINT('Ctrl Pts',(373.520791292912,-9.2994900068193,1.78192575243756));
#34809=CARTESIAN_POINT('Ctrl Pts',(373.676875412186,-9.28254382888852,1.53356284640514));
#34810=CARTESIAN_POINT('Ctrl Pts',(373.772449935031,-9.27081910472854,1.34139487439183));
#34811=CARTESIAN_POINT('Ctrl Pts',(373.905534919934,-9.24961746995725,0.989900031823699));
#34812=CARTESIAN_POINT('Ctrl Pts',(373.951330776188,-9.24032890708503,0.834564118866942));
#34813=CARTESIAN_POINT('Ctrl Pts',(373.990963030249,-9.22902519565164,0.649956575266833));
#34814=CARTESIAN_POINT('Ctrl Pts',(373.996317980896,-9.22739231734514,0.62338386927893));
#34815=CARTESIAN_POINT('Ctrl Pts',(374.004563418352,-9.22469235787126,0.579624215887875));
#34816=CARTESIAN_POINT('Ctrl Pts',(374.007650885082,-9.22363153791964,0.562475444112357));
#34817=CARTESIAN_POINT('Ctrl Pts',(374.012962870042,-9.22171222410289,0.53153417600609));
#34818=CARTESIAN_POINT('Ctrl Pts',(374.015237070075,-9.22085532973306,0.517750566732708));
#34819=CARTESIAN_POINT('Ctrl Pts',(374.019907897939,-9.21901703227588,0.488248339236894));
#34820=CARTESIAN_POINT('Ctrl Pts',(374.022277951556,-9.21803481196214,0.472525947138395));
#34821=CARTESIAN_POINT('Ctrl Pts',(374.028407436891,-9.2153532185202,0.429717432479312));
#34822=CARTESIAN_POINT('Ctrl Pts',(374.031938554337,-9.21364670288811,0.402600444660568));
#34823=CARTESIAN_POINT('Ctrl Pts',(374.049518557405,-9.20416905991896,0.252723461269151));
#34824=CARTESIAN_POINT('Ctrl Pts',(374.056841966402,-9.19618925733215,0.129292913971071));
#34825=CARTESIAN_POINT('Ctrl Pts',(374.05732994103,-9.17816558293361,-0.143793467991667));
#34826=CARTESIAN_POINT('Ctrl Pts',(374.047186826692,-9.16805883277381,-0.293173302346878));
#34827=CARTESIAN_POINT('Ctrl Pts',(374.003536190119,-9.14649399125949,-0.608946596703439));
#34828=CARTESIAN_POINT('Ctrl Pts',(373.967188941042,-9.13506495643688,-0.774525891563327));
#34829=CARTESIAN_POINT('Ctrl Pts',(373.910172669352,-9.12245901464209,-0.962268236715053));
#34830=CARTESIAN_POINT('Ctrl Pts',(373.9020228287,-9.12074338881162,-0.987941953141894));
#34831=CARTESIAN_POINT('Ctrl Pts',(373.890305339226,-9.11839421360435,-1.02331061328434));
#34832=CARTESIAN_POINT('Ctrl Pts',(373.887011793877,-9.11774591013995,-1.03309430226435));
#34833=CARTESIAN_POINT('Ctrl Pts',(373.881275338012,-9.11663726360898,-1.04986783374305));
#34834=CARTESIAN_POINT('Ctrl Pts',(373.878855269032,-9.11617561371591,-1.05686532197827));
#34835=CARTESIAN_POINT('Ctrl Pts',(373.873739213191,-9.11521233309134,-1.0714946899445));
#34836=CARTESIAN_POINT('Ctrl Pts',(373.871038561442,-9.11471100102112,-1.07912483803275));
#34837=CARTESIAN_POINT('Ctrl Pts',(373.864350528575,-9.11348666101865,-1.09779659408055));
#34838=CARTESIAN_POINT('Ctrl Pts',(373.860331457331,-9.11276550770738,-1.10882688158799));
#34839=CARTESIAN_POINT('Ctrl Pts',(373.845497517911,-9.11015524633411,-1.14885705000511));
#34840=CARTESIAN_POINT('Ctrl Pts',(373.834324931301,-9.10828611270239,-1.17772373097182));
#34841=CARTESIAN_POINT('Ctrl Pts',(373.805207972477,-9.10363859445548,-1.24984890662164));
#34842=CARTESIAN_POINT('Ctrl Pts',(373.786732975756,-9.10088608509017,-1.29288660285058));
#34843=CARTESIAN_POINT('Ctrl Pts',(373.628200862637,-9.07867107788594,-1.64105058824508));
#34844=CARTESIAN_POINT('Ctrl Pts',(373.442188700875,-9.060786765978,-1.92298691041463));
#34845=CARTESIAN_POINT('Ctrl Pts',(373.172635579764,-9.03736684685816,-2.21867663895522));
#34846=CARTESIAN_POINT('Ctrl Pts',(373.127886259431,-9.03355110023065,-2.26490594744137));
#34847=CARTESIAN_POINT('Ctrl Pts',(373.065375173721,-9.02829619794196,-2.32573108469422));
#34848=CARTESIAN_POINT('Ctrl Pts',(373.048795225766,-9.02690931525824,-2.34152338674893));
#34849=CARTESIAN_POINT('Ctrl Pts',(373.021128231472,-9.0246054763901,-2.36731934090845));
#34850=CARTESIAN_POINT('Ctrl Pts',(373.010137257783,-9.02369292082535,-2.37742516164395));
#34851=CARTESIAN_POINT('Ctrl Pts',(372.98852066386,-9.02190309580222,-2.3970254172284));
#34852=CARTESIAN_POINT('Ctrl Pts',(372.977901503438,-9.02102613677911,-2.40652648528043));
#34853=CARTESIAN_POINT('Ctrl Pts',(372.95262108032,-9.01894360036062,-2.42884504097996));
#34854=CARTESIAN_POINT('Ctrl Pts',(372.937906087321,-9.01773548686279,-2.44160056309272));
#34855=CARTESIAN_POINT('Ctrl Pts',(372.888176487528,-9.01366557316071,-2.48392483158043));
#34856=CARTESIAN_POINT('Ctrl Pts',(372.85264824625,-9.0107790035216,-2.51287881451377));
#34857=CARTESIAN_POINT('Ctrl Pts',(372.766007813455,-9.00378610675437,-2.58046408540649));
#34858=CARTESIAN_POINT('Ctrl Pts',(372.714338988455,-8.99965278418863,-2.61834692889301));
#34859=CARTESIAN_POINT('Ctrl Pts',(372.50654368449,-8.98317565633936,-2.76137681311871));
#34860=CARTESIAN_POINT('Ctrl Pts',(372.342472802998,-8.9704505851579,-2.8542943230937));
#34861=CARTESIAN_POINT('Ctrl Pts',(372.024946931316,-8.94684943402383,-2.99906237760608));
#34862=CARTESIAN_POINT('Ctrl Pts',(371.873838512743,-8.93601484324683,-3.0547306722474));
#34863=CARTESIAN_POINT('Ctrl Pts',(371.693262896961,-8.92394927217498,-3.10629331854499));
#34864=CARTESIAN_POINT('Ctrl Pts',(371.667239640493,-8.92223153189595,-3.11337215503224));
#34865=CARTESIAN_POINT('Ctrl Pts',(371.631131117034,-8.91987999810629,-3.12270921475377));
#34866=CARTESIAN_POINT('Ctrl Pts',(371.621120074106,-8.91923141176799,-3.12524662855973));
#34867=CARTESIAN_POINT('Ctrl Pts',(371.603909957456,-8.91812240905198,-3.12952079283518));
#34868=CARTESIAN_POINT('Ctrl Pts',(371.596716850296,-8.91766068402621,-3.13128091546647));
#34869=CARTESIAN_POINT('Ctrl Pts',(371.581650141689,-8.91669739252614,-3.13491267937807));
#34870=CARTESIAN_POINT('Ctrl Pts',(371.573775470693,-8.91619612388408,-3.13677947749655));
#34871=CARTESIAN_POINT('Ctrl Pts',(371.554466171337,-8.91497217861105,-3.14128025617816));
#34872=CARTESIAN_POINT('Ctrl Pts',(371.543023887539,-8.91425135380599,-3.14388152046965));
#34873=CARTESIAN_POINT('Ctrl Pts',(371.501385863074,-8.91164364383092,-3.15310854453773));
#34874=CARTESIAN_POINT('Ctrl Pts',(371.471108337201,-8.90977668199887,-3.15936247730658));
#34875=CARTESIAN_POINT('Ctrl Pts',(371.394826943607,-8.90513568987098,-3.17397746006157));
#34876=CARTESIAN_POINT('Ctrl Pts',(371.348721320573,-8.90238744192274,-3.18177511176734));
#34877=CARTESIAN_POINT('Ctrl Pts',(370.972215557926,-8.88028805195974,-3.23705331939835));
#34878=CARTESIAN_POINT('Ctrl Pts',(370.636435223777,-8.8625006098788,-3.2339467583194));
#34879=CARTESIAN_POINT('Ctrl Pts',(370.242047286525,-8.83912076040069,-3.16854539704267));
#34880=CARTESIAN_POINT('Ctrl Pts',(370.177355306584,-8.83521243613071,-3.15576673338328));
#34881=CARTESIAN_POINT('Ctrl Pts',(370.090577235932,-8.82984924984167,-3.13584145923221));
#34882=CARTESIAN_POINT('Ctrl Pts',(370.06810740405,-8.82844954180482,-3.13042701052146));
#34883=CARTESIAN_POINT('Ctrl Pts',(370.031176443963,-8.82613002043022,-3.12110649486808));
#34884=CARTESIAN_POINT('Ctrl Pts',(370.016680615896,-8.82521473144255,-3.11734040679316));
#34885=CARTESIAN_POINT('Ctrl Pts',(369.988468987625,-8.82342370563535,-3.10980057444666));
#34886=CARTESIAN_POINT('Ctrl Pts',(369.974750867716,-8.82254830934492,-3.10603678396981));
#34887=CARTESIAN_POINT('Ctrl Pts',(369.942447845319,-8.82047612227923,-3.09694353277807));
#34888=CARTESIAN_POINT('Ctrl Pts',(369.923885256421,-8.81927686426009,-3.09153745194477));
#34889=CARTESIAN_POINT('Ctrl Pts',(369.86228578262,-8.81526821728355,-3.07299461893091));
#34890=CARTESIAN_POINT('Ctrl Pts',(369.819477036711,-8.81243506504613,-3.05912406793632));
#34891=CARTESIAN_POINT('Ctrl Pts',(369.717904046284,-8.80559583727269,-3.02384655322788));
#34892=CARTESIAN_POINT('Ctrl Pts',(369.659446730677,-8.80156431086839,-3.00161702765854));
#34893=CARTESIAN_POINT('Ctrl Pts',(369.289577077117,-8.77544341746029,-2.84850675220071));
#34894=CARTESIAN_POINT('Ctrl Pts',(368.999790558607,-8.75185733027583,-2.67108026706115));
#34895=CARTESIAN_POINT('Ctrl Pts',(368.714077869421,-8.72751766118726,-2.42737126107469));
#34896=CARTESIAN_POINT('Ctrl Pts',(368.685727653493,-8.72509219348832,-2.40231331664379));
#34897=CARTESIAN_POINT('Ctrl Pts',(368.648153858862,-8.72187114619697,-2.36790550415481));
#34898=CARTESIAN_POINT('Ctrl Pts',(368.638537771904,-8.72104621490378,-2.35899116893977));
#34899=CARTESIAN_POINT('Ctrl Pts',(368.6234700361,-8.71975306463301,-2.34485106328122));
#34900=CARTESIAN_POINT('Ctrl Pts',(368.617982014262,-8.7192819547028,-2.33966451252136));
#34901=CARTESIAN_POINT('Ctrl Pts',(368.606728257555,-8.71831575569929,-2.32895382372231));
#34902=CARTESIAN_POINT('Ctrl Pts',(368.600964789967,-8.71782086879321,-2.32342751461853));
#34903=CARTESIAN_POINT('Ctrl Pts',(368.587672132874,-8.71667919427406,-2.3105866696381));
#34904=CARTESIAN_POINT('Ctrl Pts',(368.580157951719,-8.71603359993077,-2.30325658498164));
#34905=CARTESIAN_POINT('Ctrl Pts',(368.555524355962,-8.71391588625051,-2.27899048886646));
#34906=CARTESIAN_POINT('Ctrl Pts',(368.538558484274,-8.71245530964267,-2.26189885925911));
#34907=CARTESIAN_POINT('Ctrl Pts',(368.497829716912,-8.70893910993424,-2.21993777743265));
#34908=CARTESIAN_POINT('Ctrl Pts',(368.474269872882,-8.70689672524812,-2.19487454480052));
#34909=CARTESIAN_POINT('Ctrl Pts',(368.385724278261,-8.6991658851745,-2.0976041319295));
#34910=CARTESIAN_POINT('Ctrl Pts',(368.323610172938,-8.69362542709458,-2.02284531400815));
#34911=CARTESIAN_POINT('Ctrl Pts',(368.190413642978,-8.68118128868767,-1.84692738991976));
#34912=CARTESIAN_POINT('Ctrl Pts',(368.121583524464,-8.67432377286514,-1.74426015045791));
#34913=CARTESIAN_POINT('Ctrl Pts',(367.964323094424,-8.65695042181107,-1.47777372018729));
#34914=CARTESIAN_POINT('Ctrl Pts',(367.883876583687,-8.6463531005557,-1.30979717732786));
#34915=CARTESIAN_POINT('Ctrl Pts',(367.808675775431,-8.63358351280057,-1.11011836402132));
#34916=CARTESIAN_POINT('Ctrl Pts',(367.799319883033,-8.63192849258957,-1.08427856924537));
#34917=CARTESIAN_POINT('Ctrl Pts',(367.784536501266,-8.62919939233742,-1.04175757560133));
#34918=CARTESIAN_POINT('Ctrl Pts',(367.778912609586,-8.62813181088882,-1.02514580393077));
#34919=CARTESIAN_POINT('Ctrl Pts',(367.7690499777,-8.62620516760918,-0.995211460094527));
#34920=CARTESIAN_POINT('Ctrl Pts',(367.764761783044,-8.62534775895542,-0.981905556206899));
#34921=CARTESIAN_POINT('Ctrl Pts',(367.755804455931,-8.62351370061803,-0.95347954156082));
#34922=CARTESIAN_POINT('Ctrl Pts',(367.751159859272,-8.62253627257639,-0.938352142615064));
#34923=CARTESIAN_POINT('Ctrl Pts',(367.738893040261,-8.61988128451211,-0.897324737810711));
#34924=CARTESIAN_POINT('Ctrl Pts',(367.731484697227,-8.61819681978445,-0.87136260683261));
#34925=CARTESIAN_POINT('Ctrl Pts',(367.715862537183,-8.61445725475984,-0.813888406633107));
#34926=CARTESIAN_POINT('Ctrl Pts',(367.707798480677,-8.61239755177541,-0.782339047878178));
#34927=CARTESIAN_POINT('Ctrl Pts',(367.641095844426,-8.59415230024176,-0.503851933487073));
#34928=CARTESIAN_POINT('Ctrl Pts',(367.611353684704,-8.57703667973339,-0.250959089753795));
#34929=CARTESIAN_POINT('Ctrl Pts',(367.611569014087,-8.55988254489073,0.00273538678758171));
#34930=CARTESIAN_POINT('Ctrl Pts',(367.611569016176,-8.5598823785129,0.00273784736845979));
#34931=CARTESIAN_POINT('Ctrl Pts',(367.611710073435,-8.54865520450604,0.168777824769111));
#34932=CARTESIAN_POINT('Ctrl Pts',(367.624682860913,-8.5374813403058,0.334581747335591));
#34933=CARTESIAN_POINT('Ctrl Pts',(367.652687367032,-8.52592348092959,0.513387817692194));
#34934=CARTESIAN_POINT('Ctrl Pts',(367.655095167938,-8.52497669480409,0.528093493947375));
#34935=CARTESIAN_POINT('Ctrl Pts',(367.659221475309,-8.52342866708339,0.552243314487704));
#34936=CARTESIAN_POINT('Ctrl Pts',(367.660880301606,-8.52282437709589,0.561697248361017));
#34937=CARTESIAN_POINT('Ctrl Pts',(367.664185425579,-8.52165470049485,0.580051615344668));
#34938=CARTESIAN_POINT('Ctrl Pts',(367.665827030268,-8.5210890652104,0.588952795079713));
#34939=CARTESIAN_POINT('Ctrl Pts',(367.668964487263,-8.52003614966302,0.605571987683803));
#34940=CARTESIAN_POINT('Ctrl Pts',(367.670451067393,-8.51954838270824,0.613291388094639));
#34941=CARTESIAN_POINT('Ctrl Pts',(367.673915194919,-8.51843662218971,0.630931795346051));
#34942=CARTESIAN_POINT('Ctrl Pts',(367.675911218284,-8.51781368197542,0.64084898986419));
#34943=CARTESIAN_POINT('Ctrl Pts',(367.68135611575,-8.51615994237848,0.667258362000366));
#34944=CARTESIAN_POINT('Ctrl Pts',(367.684887732579,-8.515133641166,0.683733414723344));
#34945=CARTESIAN_POINT('Ctrl Pts',(367.717434045385,-8.50606631976406,0.829957434330452));
#34946=CARTESIAN_POINT('Ctrl Pts',(367.754326454239,-8.49842584579882,0.957838955793525));
#34947=CARTESIAN_POINT('Ctrl Pts',(367.833825202285,-8.48505898317226,1.18062999785816));
#34948=CARTESIAN_POINT('Ctrl Pts',(367.873313215786,-8.47929114719,1.27643866269208));
#34949=CARTESIAN_POINT('Ctrl Pts',(367.95610779294,-8.46839233689487,1.45269961353418));
#34950=CARTESIAN_POINT('Ctrl Pts',(367.998352062536,-8.46327302329506,1.53353397823649));
#34951=CARTESIAN_POINT('Ctrl Pts',(368.103258836621,-8.45132299681722,1.71507383420621));
#34952=CARTESIAN_POINT('Ctrl Pts',(368.168161612095,-8.44444675266607,1.81432306891983));
#34953=CARTESIAN_POINT('Ctrl Pts',(368.257749982054,-8.43541423760068,1.93610028770842));
#34954=CARTESIAN_POINT('Ctrl Pts',(368.277521821667,-8.43344645502713,1.96213665524159));
#34955=CARTESIAN_POINT('Ctrl Pts',(368.308191949848,-8.43042989292646,2.00127349334745));
#34956=CARTESIAN_POINT('Ctrl Pts',(368.318804062212,-8.42939242109623,2.01459624360935));
#34957=CARTESIAN_POINT('Ctrl Pts',(368.338294879654,-8.42749792103585,2.03867145611712));
#34958=CARTESIAN_POINT('Ctrl Pts',(368.347138761054,-8.42664230654933,2.04945166919761));
#34959=CARTESIAN_POINT('Ctrl Pts',(368.366402777224,-8.42478698494851,2.07262512393192));
#34960=CARTESIAN_POINT('Ctrl Pts',(368.37684687266,-8.42378631415337,2.08499786357069));
#34961=CARTESIAN_POINT('Ctrl Pts',(368.40556256551,-8.42104873819463,2.1185007992694));
#34962=CARTESIAN_POINT('Ctrl Pts',(368.424016035646,-8.41930435799133,2.13947258766219));
#34963=CARTESIAN_POINT('Ctrl Pts',(368.523877736363,-8.40994029135481,2.25003038381158));
#34964=CARTESIAN_POINT('Ctrl Pts',(368.610003139831,-8.40212161839698,2.33520626645115));
#34965=CARTESIAN_POINT('Ctrl Pts',(368.857147886366,-8.38036315177978,2.55352473298532));
#34966=CARTESIAN_POINT('Ctrl Pts',(369.026639745582,-8.36611442495966,2.67618701099045));
#34967=CARTESIAN_POINT('Ctrl Pts',(369.280675047732,-8.34632871629645,2.82482596858817));
#34968=CARTESIAN_POINT('Ctrl Pts',(369.356270036233,-8.34062382844952,2.8651045815561));
#34969=CARTESIAN_POINT('Ctrl Pts',(369.461953680405,-8.33297274252521,2.91611737569494));
#34970=CARTESIAN_POINT('Ctrl Pts',(369.490726674257,-8.33092165918123,2.92948576935605));
#34971=CARTESIAN_POINT('Ctrl Pts',(369.540551523768,-8.32743017097682,2.95174662694954));
#34972=CARTESIAN_POINT('Ctrl Pts',(369.561508775393,-8.32597963866046,2.96084389745094));
#34973=CARTESIAN_POINT('Ctrl Pts',(369.59213729467,-8.32388771728713,2.97375402578185));
#34974=CARTESIAN_POINT('Ctrl Pts',(369.601732540538,-8.32323632750502,2.97774394464626));
#34975=CARTESIAN_POINT('Ctrl Pts',(369.618656140426,-8.32209461736922,2.9846853389217));
#34976=CARTESIAN_POINT('Ctrl Pts',(369.625976291165,-8.32160313956004,2.98765638034294));
#34977=CARTESIAN_POINT('Ctrl Pts',(369.641537313387,-8.32056343174632,2.99390560959195));
#34978=CARTESIAN_POINT('Ctrl Pts',(369.64978083243,-8.32001562209281,2.99717671587013));
#34979=CARTESIAN_POINT('Ctrl Pts',(369.672285079689,-8.31852797463428,3.00599926418696));
#34980=CARTESIAN_POINT('Ctrl Pts',(369.686572220416,-8.31759206600672,3.01148331005089));
#34981=CARTESIAN_POINT('Ctrl Pts',(369.754761254107,-8.31316331518592,3.03710155205793));
#34982=CARTESIAN_POINT('Ctrl Pts',(369.809160345929,-8.30974303628744,3.05589287830984));
#34983=CARTESIAN_POINT('Ctrl Pts',(369.904320288055,-8.30390669536128,3.08593690536323));
#34984=CARTESIAN_POINT('Ctrl Pts',(369.944851123363,-8.3014660611637,3.09786236649158));
#34985=CARTESIAN_POINT('Ctrl Pts',(370.057384557568,-8.29478493070474,3.12858247710776));
#34986=CARTESIAN_POINT('Ctrl Pts',(370.129822672428,-8.29059037874307,3.14568608802348));
#34987=CARTESIAN_POINT('Ctrl Pts',(370.326783099405,-8.2793246359618,3.18504540739398));
#34988=CARTESIAN_POINT('Ctrl Pts',(370.452125370521,-8.2722996112935,3.20250438614265));
#34989=CARTESIAN_POINT('Ctrl Pts',(370.735459976461,-8.25624423185949,3.22509574663828));
#34990=CARTESIAN_POINT('Ctrl Pts',(370.893441169133,-8.24716430606265,3.22606738962386));
#34991=CARTESIAN_POINT('Ctrl Pts',(371.079752218701,-8.23597487965228,3.2135212557643));
#34992=CARTESIAN_POINT('Ctrl Pts',(371.108629580974,-8.23422730335871,3.21118512113918));
#34993=CARTESIAN_POINT('Ctrl Pts',(371.153650157234,-8.23148041914378,3.20693132912214));
#34994=CARTESIAN_POINT('Ctrl Pts',(371.16981745274,-8.23048947741362,3.2052802800547));
#34995=CARTESIAN_POINT('Ctrl Pts',(371.198438471837,-8.22872693759028,3.20213851040646));
#34996=CARTESIAN_POINT('Ctrl Pts',(371.210897364925,-8.22795691110852,3.2006972254573));
#34997=CARTESIAN_POINT('Ctrl Pts',(371.239594160215,-8.22617673326256,3.19720761575582));
#34998=CARTESIAN_POINT('Ctrl Pts',(371.25582539991,-8.22516499189884,3.19510826037917));
#34999=CARTESIAN_POINT('Ctrl Pts',(371.300481151716,-8.22236776516191,3.18898627473215));
#35000=CARTESIAN_POINT('Ctrl Pts',(371.328868455988,-8.22057425551758,3.18470741151137));
#35001=CARTESIAN_POINT('Ctrl Pts',(371.490987138291,-8.21024099090766,3.15805122471671));
#35002=CARTESIAN_POINT('Ctrl Pts',(371.623241172016,-8.20144870670018,3.12763389163054));
#35003=CARTESIAN_POINT('Ctrl Pts',(371.945317704611,-8.17916813330987,3.03182834146058));
#35004=CARTESIAN_POINT('Ctrl Pts',(372.131675733991,-8.16547659336062,2.95687880945177));
#35005=CARTESIAN_POINT('Ctrl Pts',(372.309820650725,-8.15202831126679,2.86513683042647));
#35006=CARTESIAN_POINT('Ctrl Pts',(372.309820607824,-7.90820793933159,2.86513685252009));
#35007=CARTESIAN_POINT('Ctrl Pts',(372.280086990719,-7.91046518366678,2.88044922194635));
#35008=CARTESIAN_POINT('Ctrl Pts',(372.250105592529,-7.91271861207407,2.89530359235541));
#35009=CARTESIAN_POINT('Ctrl Pts',(372.123144234145,-7.92215390123291,2.95576140355205));
#35010=CARTESIAN_POINT('Ctrl Pts',(372.024154646074,-7.92925280294976,2.99698043300587));
#35011=CARTESIAN_POINT('Ctrl Pts',(371.90064077752,-7.93765725365726,3.04132404111153));
#35012=CARTESIAN_POINT('Ctrl Pts',(371.877903717594,-7.9391859834764,3.04920073553008));
#35013=CARTESIAN_POINT('Ctrl Pts',(371.845001799018,-7.94136957640213,3.06018764390311));
#35014=CARTESIAN_POINT('Ctrl Pts',(371.834907045115,-7.94203568195476,3.0635031794916));
#35015=CARTESIAN_POINT('Ctrl Pts',(371.817271076785,-7.94319246436888,3.06919908971726));
#35016=CARTESIAN_POINT('Ctrl Pts',(371.80973723436,-7.94368442135543,3.07160172031258));
#35017=CARTESIAN_POINT('Ctrl Pts',(371.793734337252,-7.94472466543712,3.07664041460402));
#35018=CARTESIAN_POINT('Ctrl Pts',(371.785263200904,-7.94527253492709,3.07926926083995));
#35019=CARTESIAN_POINT('Ctrl Pts',(371.762161253595,-7.94675935033236,3.08633405820965));
#35020=CARTESIAN_POINT('Ctrl Pts',(371.747509345397,-7.94769437851849,3.09070099076668));
#35021=CARTESIAN_POINT('Ctrl Pts',(371.677823149475,-7.95210625765782,3.11093181213383));
#35022=CARTESIAN_POINT('Ctrl Pts',(371.622399981856,-7.9555112425893,3.12543203121512));
#35023=CARTESIAN_POINT('Ctrl Pts',(371.529803482967,-7.96107326358394,3.14703769447499));
#35024=CARTESIAN_POINT('Ctrl Pts',(371.492841385017,-7.9632604330401,3.1549791524786));
#35025=CARTESIAN_POINT('Ctrl Pts',(371.373907483905,-7.97021662422249,3.17835129379364));
#35026=CARTESIAN_POINT('Ctrl Pts',(371.291471179694,-7.97491538445874,3.19125145335398));
#35027=CARTESIAN_POINT('Ctrl Pts',(371.047721419616,-7.98867206365104,3.21975469172786));
#35028=CARTESIAN_POINT('Ctrl Pts',(370.885630253705,-7.99765689301431,3.22641078265614));
#35029=CARTESIAN_POINT('Ctrl Pts',(370.602659606326,-8.01382900628593,3.2166951716844));
#35030=CARTESIAN_POINT('Ctrl Pts',(370.481929849426,-8.02088202712811,3.20571541323337));
#35031=CARTESIAN_POINT('Ctrl Pts',(370.335191684674,-8.02978393543228,3.18398041564805));
#35032=CARTESIAN_POINT('Ctrl Pts',(370.308322637838,-8.03142738105898,3.17965205389522));
#35033=CARTESIAN_POINT('Ctrl Pts',(370.26586856675,-8.03404674330235,3.17226025329552));
#35034=CARTESIAN_POINT('Ctrl Pts',(370.250245461198,-8.03501554826466,3.16942094596043));
#35035=CARTESIAN_POINT('Ctrl Pts',(370.220903815099,-8.0368445111308,3.16386414842194));
#35036=CARTESIAN_POINT('Ctrl Pts',(370.207180696864,-8.03770382449859,3.16117258452826));
#35037=CARTESIAN_POINT('Ctrl Pts',(370.176338439494,-8.03964409371157,3.15491464703476));
#35038=CARTESIAN_POINT('Ctrl Pts',(370.159230039825,-8.04072662942793,3.1512981077441));
#35039=CARTESIAN_POINT('Ctrl Pts',(370.115500467723,-8.04351002337406,3.14168168229503));
#35040=CARTESIAN_POINT('Ctrl Pts',(370.088924950514,-8.04521719513872,3.13548266995461));
#35041=CARTESIAN_POINT('Ctrl Pts',(369.898860192772,-8.05754191029404,3.0885952364427));
#35042=CARTESIAN_POINT('Ctrl Pts',(369.73872979055,-8.06856056585794,3.03548561696092));
#35043=CARTESIAN_POINT('Ctrl Pts',(369.391753120084,-8.09375346791797,2.88936216438681));
#35044=CARTESIAN_POINT('Ctrl Pts',(369.208279525975,-8.10801324738904,2.79023369857103));
#35045=CARTESIAN_POINT('Ctrl Pts',(368.970692334742,-8.12698279462253,2.63042670521092));
#35046=CARTESIAN_POINT('Ctrl Pts',(368.907349021084,-8.13209018822261,2.58438348545078));
#35047=CARTESIAN_POINT('Ctrl Pts',(368.833075972817,-8.13808215731996,2.52614478967241));
#35048=CARTESIAN_POINT('Ctrl Pts',(368.820485809273,-8.13909796617689,2.51611944987794));
#35049=CARTESIAN_POINT('Ctrl Pts',(368.800937002428,-8.14067467146286,2.50031232135528));
#35050=CARTESIAN_POINT('Ctrl Pts',(368.793926906349,-8.1412399582074,2.49459499264479));
#35051=CARTESIAN_POINT('Ctrl Pts',(368.780863494022,-8.14229301839339,2.48384876462252));
#35052=CARTESIAN_POINT('Ctrl Pts',(368.774804568482,-8.14278127261454,2.47882724737233));
#35053=CARTESIAN_POINT('Ctrl Pts',(368.760978202766,-8.14389517052357,2.46728254054745));
#35054=CARTESIAN_POINT('Ctrl Pts',(368.753223116981,-8.14451975002664,2.46074483567939));
#35055=CARTESIAN_POINT('Ctrl Pts',(368.732607649836,-8.14617995528916,2.44319838648328));
#35056=CARTESIAN_POINT('Ctrl Pts',(368.719802732146,-8.14721103104995,2.43212457852127));
#35057=CARTESIAN_POINT('Ctrl Pts',(368.602484079485,-8.15666297402621,2.32903941019326));
#35058=CARTESIAN_POINT('Ctrl Pts',(368.503935995164,-8.16464417543573,2.23043414790647));
#35059=CARTESIAN_POINT('Ctrl Pts',(368.387882662782,-8.17456952934213,2.09819367433383));
#35060=CARTESIAN_POINT('Ctrl Pts',(368.364170342609,-8.17662825253761,2.07022539108675));
#35061=CARTESIAN_POINT('Ctrl Pts',(368.239858184967,-8.18762204986215,1.91842388925832));
#35062=CARTESIAN_POINT('Ctrl Pts',(368.148082930536,-8.19647654078909,1.78765521064309));
#35063=CARTESIAN_POINT('Ctrl Pts',(368.004770448704,-8.21246346180662,1.54733462404254));
#35064=CARTESIAN_POINT('Ctrl Pts',(367.949006095433,-8.21946769979819,1.44067843270663));
#35065=CARTESIAN_POINT('Ctrl Pts',(367.888116111698,-8.22831454150035,1.30642666780241));
#35066=CARTESIAN_POINT('Ctrl Pts',(367.877210216209,-8.22995484545603,1.28154972385356));
#35067=CARTESIAN_POINT('Ctrl Pts',(367.860433640642,-8.23257034421545,1.24192674102022));
#35068=CARTESIAN_POINT('Ctrl Pts',(367.854355048219,-8.23353846373981,1.22726973669558));
#35069=CARTESIAN_POINT('Ctrl Pts',(367.843122710824,-8.23536684163724,1.19961026756124));
#35070=CARTESIAN_POINT('Ctrl Pts',(367.837944873807,-8.23622626141706,1.18661793867848));
#35071=CARTESIAN_POINT('Ctrl Pts',(367.826477688442,-8.23816772173516,1.15729058029123));
#35072=CARTESIAN_POINT('Ctrl Pts',(367.820236561862,-8.23925135030846,1.14093728741634));
#35073=CARTESIAN_POINT('Ctrl Pts',(367.804587178898,-8.24203943674257,1.09890736046548));
#35074=CARTESIAN_POINT('Ctrl Pts',(367.795372103528,-8.24375024427384,1.07316075319971));
#35075=CARTESIAN_POINT('Ctrl Pts',(367.719352860111,-8.25847836583262,0.851931177819804));
#35076=CARTESIAN_POINT('Ctrl Pts',(367.671171783565,-8.27211457550284,0.650594435583398));
#35077=CARTESIAN_POINT('Ctrl Pts',(367.621842352533,-8.29613128936243,0.297628820466118));
#35078=CARTESIAN_POINT('Ctrl Pts',(367.611477319688,-8.30633729566589,0.147924090474079));
#35079=CARTESIAN_POINT('Ctrl Pts',(367.611595484732,-8.31930199709675,-0.0464266309118273));
#35080=CARTESIAN_POINT('Ctrl Pts',(367.612542851662,-8.32224784993948,-0.0908902097798106));
#35081=CARTESIAN_POINT('Ctrl Pts',(367.616739587707,-8.32879973082755,-0.190749436956861));
#35082=CARTESIAN_POINT('Ctrl Pts',(367.620500025738,-8.33238772592903,-0.246111879924262));
#35083=CARTESIAN_POINT('Ctrl Pts',(367.62710395784,-8.33686573344007,-0.316426615952528));
#35084=CARTESIAN_POINT('Ctrl Pts',(367.628625877529,-8.33782041940696,-0.331490198857738));
#35085=CARTESIAN_POINT('Ctrl Pts',(367.631204149121,-8.33932326440921,-0.355328368646034));
#35086=CARTESIAN_POINT('Ctrl Pts',(367.632190512579,-8.3398751842414,-0.364110079067891));
#35087=CARTESIAN_POINT('Ctrl Pts',(367.63412899826,-8.34091767433136,-0.380751269397729));
#35088=CARTESIAN_POINT('Ctrl Pts',(367.63507394976,-8.34140860954351,-0.388611224535128));
#35089=CARTESIAN_POINT('Ctrl Pts',(367.637362880658,-8.34255861599188,-0.407075821014035));
#35090=CARTESIAN_POINT('Ctrl Pts',(367.638730668435,-8.34321634959959,-0.417677354710722));
#35091=CARTESIAN_POINT('Ctrl Pts',(367.643396795445,-8.34536766636677,-0.452478567840202));
#35092=CARTESIAN_POINT('Ctrl Pts',(367.646917564716,-8.34684936931321,-0.476648228589994));
#35093=CARTESIAN_POINT('Ctrl Pts',(367.667874803233,-8.35496004467795,-0.609880497263251));
#35094=CARTESIAN_POINT('Ctrl Pts',(367.690635811715,-8.3613340615535,-0.718041730571144));
#35095=CARTESIAN_POINT('Ctrl Pts',(367.794062685897,-8.38426282485431,-1.10868821028692));
#35096=CARTESIAN_POINT('Ctrl Pts',(367.907650662578,-8.40019927814039,-1.3809283401776));
#35097=CARTESIAN_POINT('Ctrl Pts',(368.084294270505,-8.42070211348759,-1.6812153366278));
#35098=CARTESIAN_POINT('Ctrl Pts',(368.113248759935,-8.42396179906062,-1.72768549722269));
#35099=CARTESIAN_POINT('Ctrl Pts',(368.155200102014,-8.42856160374572,-1.79134243183714));
#35100=CARTESIAN_POINT('Ctrl Pts',(368.167207736691,-8.42986506810926,-1.8091719721473));
#35101=CARTESIAN_POINT('Ctrl Pts',(368.186864084206,-8.43197860263268,-1.83773769116824));
#35102=CARTESIAN_POINT('Ctrl Pts',(368.194402001872,-8.43278446625057,-1.84854958556695));
#35103=CARTESIAN_POINT('Ctrl Pts',(368.210226023406,-8.43446676269025,-1.87095233311898));
#35104=CARTESIAN_POINT('Ctrl Pts',(368.218523080912,-8.43534360369057,-1.88253506286116));
#35105=CARTESIAN_POINT('Ctrl Pts',(368.238309556923,-8.43742259020282,-1.9097737023508));
#35106=CARTESIAN_POINT('Ctrl Pts',(368.249864115778,-8.43862724150266,-1.92538139629195));
#35107=CARTESIAN_POINT('Ctrl Pts',(368.288932171767,-8.44266997912132,-1.97716848021377));
#35108=CARTESIAN_POINT('Ctrl Pts',(368.317068880426,-8.445532371904,-2.01286878287935));
#35109=CARTESIAN_POINT('Ctrl Pts',(368.38620945163,-8.45245486558623,-2.09687780221178));
#35110=CARTESIAN_POINT('Ctrl Pts',(368.427900205423,-8.45654123444005,-2.14459425201078));
#35111=CARTESIAN_POINT('Ctrl Pts',(368.642178747393,-8.47711837533822,-2.3757233866474));
#35112=CARTESIAN_POINT('Ctrl Pts',(368.834435899457,-8.49436476774445,-2.53968101669466));
#35113=CARTESIAN_POINT('Ctrl Pts',(369.137148184271,-8.51877219145563,-2.74195998620847));
#35114=CARTESIAN_POINT('Ctrl Pts',(369.233730580566,-8.52619606239747,-2.79943836340262));
#35115=CARTESIAN_POINT('Ctrl Pts',(369.347787486643,-8.53440170116251,-2.8594788935041));
#35116=CARTESIAN_POINT('Ctrl Pts',(369.362508231564,-8.53545036804817,-2.86708362932596));
#35117=CARTESIAN_POINT('Ctrl Pts',(369.386336786683,-8.53713037258166,-2.87916156644804));
#35118=CARTESIAN_POINT('Ctrl Pts',(369.395408003137,-8.53776587949882,-2.88370576596471));
#35119=CARTESIAN_POINT('Ctrl Pts',(369.411538065397,-8.53888854459019,-2.89169101050481));
#35120=CARTESIAN_POINT('Ctrl Pts',(369.418588191206,-8.53937674661113,-2.89514917637948));
#35121=CARTESIAN_POINT('Ctrl Pts',(369.433887041093,-8.5404307279767,-2.90258418543496));
#35122=CARTESIAN_POINT('Ctrl Pts',(369.442140099764,-8.54099593147818,-2.90655165457691));
#35123=CARTESIAN_POINT('Ctrl Pts',(369.465407992438,-8.54258025177585,-2.91761531896628));
#35124=CARTESIAN_POINT('Ctrl Pts',(369.480461174431,-8.54359454220465,-2.9246308274129));
#35125=CARTESIAN_POINT('Ctrl Pts',(369.575854256771,-8.54995908941189,-2.96819424163794));
#35126=CARTESIAN_POINT('Ctrl Pts',(369.657620342324,-8.55513363284189,-3.00154853061383));
#35127=CARTESIAN_POINT('Ctrl Pts',(370.011507173406,-8.5767672644845,-3.12921810364449));
#35128=CARTESIAN_POINT('Ctrl Pts',(370.294228938767,-8.5922973475263,-3.19019520220454));
#35129=CARTESIAN_POINT('Ctrl Pts',(370.667600248984,-8.61397741452302,-3.21959870439427));
#35130=CARTESIAN_POINT('Ctrl Pts',(370.754127713609,-8.61907070089868,-3.222914550765));
#35131=CARTESIAN_POINT('Ctrl Pts',(370.866206202885,-8.62580659224822,-3.22269333834952));
#35132=CARTESIAN_POINT('Ctrl Pts',(370.891731653546,-8.62734986083329,-3.22233964974608));
#35133=CARTESIAN_POINT('Ctrl Pts',(370.932754814432,-8.62984601932619,-3.22128364106536));
#35134=CARTESIAN_POINT('Ctrl Pts',(370.948256665357,-8.63079291850305,-3.22077258828468));
#35135=CARTESIAN_POINT('Ctrl Pts',(370.977793593374,-8.63260433022701,-3.2195853308684));
#35136=CARTESIAN_POINT('Ctrl Pts',(370.991829151669,-8.63346819381622,-3.21892919643937));
#35137=CARTESIAN_POINT('Ctrl Pts',(371.023943843725,-8.63545209835819,-3.21721735482709));
#35138=CARTESIAN_POINT('Ctrl Pts',(371.042019141172,-8.63657401386671,-3.21610100556774));
#35139=CARTESIAN_POINT('Ctrl Pts',(371.0981077301,-8.64007231940927,-3.21216210901745));
#35140=CARTESIAN_POINT('Ctrl Pts',(371.13607993156,-8.64246492162768,-3.20881753324871));
#35141=CARTESIAN_POINT('Ctrl Pts',(371.323065390468,-8.6543709789313,-3.18899964625002));
#35142=CARTESIAN_POINT('Ctrl Pts',(371.470843709041,-8.66418340480201,-3.16281788971042));
#35143=CARTESIAN_POINT('Ctrl Pts',(371.808019720595,-8.68740877898196,-3.07848978745767));
#35144=CARTESIAN_POINT('Ctrl Pts',(371.994964430348,-8.70093656470399,-3.01298701823323));
#35145=CARTESIAN_POINT('Ctrl Pts',(372.258324434379,-8.72023247264507,-2.89253752275486));
#35146=CARTESIAN_POINT('Ctrl Pts',(372.340256801282,-8.726265901354,-2.85074011217185));
#35147=CARTESIAN_POINT('Ctrl Pts',(372.434101420843,-8.73312241580129,-2.79768861184771));
#35148=CARTESIAN_POINT('Ctrl Pts',(372.447848604417,-8.73412538383268,-2.78978271029323));
#35149=CARTESIAN_POINT('Ctrl Pts',(372.470111171759,-8.73574657819729,-2.77676006328427));
#35150=CARTESIAN_POINT('Ctrl Pts',(372.478662054648,-8.73636853007917,-2.77170495966517));
#35151=CARTESIAN_POINT('Ctrl Pts',(372.493917045511,-8.73747659588031,-2.76259108389033));
#35152=CARTESIAN_POINT('Ctrl Pts',(372.500629837353,-8.73796364820118,-2.7585473262954));
#35153=CARTESIAN_POINT('Ctrl Pts',(372.515288894549,-8.7390260496834,-2.74964373610651));
#35154=CARTESIAN_POINT('Ctrl Pts',(372.523228864249,-8.73960074045243,-2.74477392861657));
#35155=CARTESIAN_POINT('Ctrl Pts',(372.545891413785,-8.74123922101606,-2.73073877537181));
#35156=CARTESIAN_POINT('Ctrl Pts',(372.560561533682,-8.74229764303158,-2.72148876513128));
#35157=CARTESIAN_POINT('Ctrl Pts',(372.664710263777,-8.74980125781713,-2.65463843694444));
#35158=CARTESIAN_POINT('Ctrl Pts',(372.751371734914,-8.75598996992613,-2.59274966585779));
#35159=CARTESIAN_POINT('Ctrl Pts',(373.010350760912,-8.7748321634107,-2.38770266431179));
#35160=CARTESIAN_POINT('Ctrl Pts',(373.170923815391,-8.78707004260135,-2.23081203975934));
#35161=CARTESIAN_POINT('Ctrl Pts',(373.39405240962,-8.80698051993958,-1.96204129408293));
#35162=CARTESIAN_POINT('Ctrl Pts',(373.468453722652,-8.81426622328595,-1.86095945832559));
#35163=CARTESIAN_POINT('Ctrl Pts',(373.552135841529,-8.82347335762787,-1.73215998039783));
#35164=CARTESIAN_POINT('Ctrl Pts',(373.56718835851,-8.82517475105587,-1.70831248317346));
#35165=CARTESIAN_POINT('Ctrl Pts',(373.590422957371,-8.82787528104109,-1.6704091044658));
#35166=CARTESIAN_POINT('Ctrl Pts',(373.598815135508,-8.82886669560793,-1.65648322735324));
#35167=CARTESIAN_POINT('Ctrl Pts',(373.614211714903,-8.83071596970691,-1.6304914329712));
#35168=CARTESIAN_POINT('Ctrl Pts',(373.62124386395,-8.83157279323784,-1.61844233639485));
#35169=CARTESIAN_POINT('Ctrl Pts',(373.636660077512,-8.83347868913804,-1.59162931583972));
#35170=CARTESIAN_POINT('Ctrl Pts',(373.645006106512,-8.83452910087984,-1.57684410968404));
#35171=CARTESIAN_POINT('Ctrl Pts',(373.668933256872,-8.83759572173967,-1.53366298663896));
#35172=CARTESIAN_POINT('Ctrl Pts',(373.68420324782,-8.83962290476539,-1.50509792302008));
#35173=CARTESIAN_POINT('Ctrl Pts',(373.795591967154,-8.85495618681343,-1.28895223108716));
#35174=CARTESIAN_POINT('Ctrl Pts',(373.873514766549,-8.86890196104991,-1.09260953094886));
#35175=CARTESIAN_POINT('Ctrl Pts',(373.994218893703,-8.89838177070537,-0.672581343437026));
#35176=CARTESIAN_POINT('Ctrl Pts',(374.03364455971,-8.91387318540343,-0.449068537048291));
#35177=CARTESIAN_POINT('Ctrl Pts',(374.051031039861,-8.929963350414,-0.198695842773865));
#35178=CARTESIAN_POINT('Ctrl Pts',(374.05245521497,-8.93152917483734,-0.174114241255168));
#35179=CARTESIAN_POINT('Ctrl Pts',(374.054059219456,-8.93370732945663,-0.139578312620742));
#35180=CARTESIAN_POINT('Ctrl Pts',(374.05447483004,-8.93433182340271,-0.129636497798358));
#35181=CARTESIAN_POINT('Ctrl Pts',(374.055142970111,-8.93545630637857,-0.111659113525762));
#35182=CARTESIAN_POINT('Ctrl Pts',(374.055411489563,-8.93595716670393,-0.103624233659263));
#35183=CARTESIAN_POINT('Ctrl Pts',(374.055898440098,-8.93697648770251,-0.087213965188911));
#35184=CARTESIAN_POINT('Ctrl Pts',(374.056114282651,-8.93749480269508,-0.0788385980667228));
#35185=CARTESIAN_POINT('Ctrl Pts',(374.056583116144,-8.93881681083265,-0.0574006034985904));
#35186=CARTESIAN_POINT('Ctrl Pts',(374.05678934283,-8.93961794002964,-0.0443369604012309));
#35187=CARTESIAN_POINT('Ctrl Pts',(374.057314010573,-8.9429164726124,0.00973007392690714));
#35188=CARTESIAN_POINT('Ctrl Pts',(374.056929353104,-8.94537754778542,0.0507383650268841));
#35189=CARTESIAN_POINT('Ctrl Pts',(374.053790212408,-8.95191054952937,0.160980788662421));
#35190=CARTESIAN_POINT('Ctrl Pts',(374.049585704021,-8.95592172200404,0.230154105139503));
#35191=CARTESIAN_POINT('Ctrl Pts',(374.029619917176,-8.96821056709524,0.444323061536362));
#35192=CARTESIAN_POINT('Ctrl Pts',(374.006247755122,-8.97629888771257,0.588423605037938));
#35193=CARTESIAN_POINT('Ctrl Pts',(373.926928661078,-8.99590137912172,0.929272088240766));
#35194=CARTESIAN_POINT('Ctrl Pts',(373.861882524801,-9.00747079204436,1.12322093847833));
#35195=CARTESIAN_POINT('Ctrl Pts',(373.767783107977,-9.02132862110302,1.33478564010711));
#35196=CARTESIAN_POINT('Ctrl Pts',(373.756307574278,-9.02298185513137,1.35972317252434));
#35197=CARTESIAN_POINT('Ctrl Pts',(373.736981758354,-9.02570901715247,1.40034542629178));
#35198=CARTESIAN_POINT('Ctrl Pts',(373.729319383169,-9.02677646923472,1.41611835020823));
#35199=CARTESIAN_POINT('Ctrl Pts',(373.715313669313,-9.02870354703405,1.44436019077459));
#35200=CARTESIAN_POINT('Ctrl Pts',(373.709017101887,-9.02956152441111,1.45685190496375));
#35201=CARTESIAN_POINT('Ctrl Pts',(373.695414818185,-9.03139753168407,1.48340582142249));
#35202=CARTESIAN_POINT('Ctrl Pts',(373.688086333106,-9.03237634637523,1.49745588343914));
#35203=CARTESIAN_POINT('Ctrl Pts',(373.667960981138,-9.03503696789336,1.53535557357796));
#35204=CARTESIAN_POINT('Ctrl Pts',(373.654967023997,-9.03672572201427,1.55909855278998));
#35205=CARTESIAN_POINT('Ctrl Pts',(373.583377403597,-9.04587906329855,1.6860846744109));
#35206=CARTESIAN_POINT('Ctrl Pts',(373.519416571169,-9.0535355239846,1.78618283356527));
#35207=CARTESIAN_POINT('Ctrl Pts',(373.359394680087,-9.07158455493074,2.00853436468186));
#35208=CARTESIAN_POINT('Ctrl Pts',(373.259720159933,-9.08207575872823,2.12782521489966));
#35209=CARTESIAN_POINT('Ctrl Pts',(373.034486012881,-9.10400256145632,2.36091118785168));
#35210=CARTESIAN_POINT('Ctrl Pts',(372.907748531155,-9.11540677438659,2.47296128975212));
#35211=CARTESIAN_POINT('Ctrl Pts',(372.751278684957,-9.12799060859756,2.59077296261676));
#35212=CARTESIAN_POINT('Ctrl Pts',(372.729553149703,-9.12970667999619,2.60670801113934));
#35213=CARTESIAN_POINT('Ctrl Pts',(372.699224948657,-9.13205666435531,2.62837321771799));
#35214=CARTESIAN_POINT('Ctrl Pts',(372.690791413357,-9.13270533652586,2.63433676160869));
#35215=CARTESIAN_POINT('Ctrl Pts',(372.676259281883,-9.13381466415075,2.64450831542047));
#35216=CARTESIAN_POINT('Ctrl Pts',(372.670174638739,-9.13427662756676,2.64873598583141));
#35217=CARTESIAN_POINT('Ctrl Pts',(372.657406982543,-9.13524063877535,2.65754194887807));
#35218=CARTESIAN_POINT('Ctrl Pts',(372.650721213465,-9.13574238699454,2.66211607902084));
#35219=CARTESIAN_POINT('Ctrl Pts',(372.634294188691,-9.13696790086603,2.67326408328522));
#35220=CARTESIAN_POINT('Ctrl Pts',(372.624533965104,-9.13768980728556,2.6798100585528));
#35221=CARTESIAN_POINT('Ctrl Pts',(372.588898999434,-9.14030374623606,2.7034281013089));
#35222=CARTESIAN_POINT('Ctrl Pts',(372.5628131861,-9.1421757402663,2.72018060855473));
#35223=CARTESIAN_POINT('Ctrl Pts',(372.496649094611,-9.14683131053973,2.76133548802704));
#35224=CARTESIAN_POINT('Ctrl Pts',(372.456271155149,-9.14958890736441,2.78524446962735));
#35225=CARTESIAN_POINT('Ctrl Pts',(372.380529333718,-9.15463595027393,2.82788746361087));
#35226=CARTESIAN_POINT('Ctrl Pts',(372.345335160387,-9.1569324153513,2.84684738925577));
#35227=CARTESIAN_POINT('Ctrl Pts',(372.309820498245,-9.15921048455975,2.86513690895141));
#35228=CARTESIAN_POINT('Origin',(370.834317853224,2.31077344927308,0.));
#35229=CARTESIAN_POINT('',(372.309820694103,-10.6540649855006,2.86513680808755));
#35230=CARTESIAN_POINT('',(372.30982057914,-10.4044982614434,2.86513686729153));
#35231=CARTESIAN_POINT('',(372.309820613641,2.31077344927308,2.86513684952399));
#35232=CARTESIAN_POINT('Ctrl Pts',(372.309820694103,-10.6540649855006,2.86513680808753));
#35233=CARTESIAN_POINT('Ctrl Pts',(372.415741525282,-10.6473842167664,2.81058915546863));
#35234=CARTESIAN_POINT('Ctrl Pts',(372.518580798336,-10.6406504991396,2.75019705918438));
#35235=CARTESIAN_POINT('Ctrl Pts',(372.689950599824,-10.6287318346147,2.63633005567726));
#35236=CARTESIAN_POINT('Ctrl Pts',(372.760076734383,-10.6236348626481,2.5855482700573));
#35237=CARTESIAN_POINT('Ctrl Pts',(372.847388158359,-10.6169502380564,2.51679758430738));
#35238=CARTESIAN_POINT('Ctrl Pts',(372.866531028819,-10.6154628004408,2.5013659651471));
#35239=CARTESIAN_POINT('Ctrl Pts',(372.897293933122,-10.613035709347,2.47598086920582));
#35240=CARTESIAN_POINT('Ctrl Pts',(372.909023179202,-10.6121014595408,2.46616085619295));
#35241=CARTESIAN_POINT('Ctrl Pts',(372.931425337172,-10.6102997498211,2.44713229312994));
#35242=CARTESIAN_POINT('Ctrl Pts',(372.942108637489,-10.6094328248293,2.43793647559723));
#35243=CARTESIAN_POINT('Ctrl Pts',(372.96644637373,-10.6074399092532,2.41670783489947));
#35244=CARTESIAN_POINT('Ctrl Pts',(372.980059799273,-10.6063120152557,2.40462892488927));
#35245=CARTESIAN_POINT('Ctrl Pts',(373.023043057009,-10.6027081602531,2.36583511495597));
#35246=CARTESIAN_POINT('Ctrl Pts',(373.052020967307,-10.6002142601995,2.33869332760768));
#35247=CARTESIAN_POINT('Ctrl Pts',(373.264490521334,-10.5814331886314,2.13218617716722));
#35248=CARTESIAN_POINT('Ctrl Pts',(373.426443558802,-10.5641845555086,1.93204392985168));
#35249=CARTESIAN_POINT('Ctrl Pts',(373.629624906426,-10.53835596795,1.60875283777286));
#35250=CARTESIAN_POINT('Ctrl Pts',(373.690075553573,-10.5298954413006,1.49882580397127));
#35251=CARTESIAN_POINT('Ctrl Pts',(373.761250745643,-10.5190223178478,1.34936888296517));
#35252=CARTESIAN_POINT('Ctrl Pts',(373.777850077721,-10.5164073757771,1.31276459435082));
#35253=CARTESIAN_POINT('Ctrl Pts',(373.804693393816,-10.5120507616063,1.25049960492534));
#35254=CARTESIAN_POINT('Ctrl Pts',(373.815299717004,-10.5102920479727,1.22500096351926));
#35255=CARTESIAN_POINT('Ctrl Pts',(373.829754117939,-10.5078442784519,1.18895126212215));
#35256=CARTESIAN_POINT('Ctrl Pts',(373.833876487293,-10.5071400020856,1.17851242218445));
#35257=CARTESIAN_POINT('Ctrl Pts',(373.840842876917,-10.5059393896853,1.16059846735347));
#35258=CARTESIAN_POINT('Ctrl Pts',(373.843713738303,-10.5054414766271,1.15313396138523));
#35259=CARTESIAN_POINT('Ctrl Pts',(373.849233797692,-10.5044780319269,1.1386202682177));
#35260=CARTESIAN_POINT('Ctrl Pts',(373.851886094659,-10.5040123039837,1.13157243622031));
#35261=CARTESIAN_POINT('Ctrl Pts',(373.859052311108,-10.5027460584633,1.11232558616725));
#35262=CARTESIAN_POINT('Ctrl Pts',(373.863517176132,-10.5019484094258,1.10010827910782));
#35263=CARTESIAN_POINT('Ctrl Pts',(373.880422393603,-10.4988929268736,1.05296681646964));
#35264=CARTESIAN_POINT('Ctrl Pts',(373.892334263822,-10.4966640817572,1.01785455082374));
#35265=CARTESIAN_POINT('Ctrl Pts',(373.970297874108,-10.4814759300663,0.774307632696504));
#35266=CARTESIAN_POINT('Ctrl Pts',(374.015601465828,-10.4694320878432,0.559804046312851));
#35267=CARTESIAN_POINT('Ctrl Pts',(374.053506787591,-10.4494456948658,0.204991168080699));
#35268=CARTESIAN_POINT('Ctrl Pts',(374.059333589791,-10.4416540011318,0.0668444972291463));
#35269=CARTESIAN_POINT('Ctrl Pts',(374.054537275212,-10.4290396379657,-0.150072582958748));
#35270=CARTESIAN_POINT('Ctrl Pts',(374.049901859715,-10.4243838796136,-0.228807595503647));
#35271=CARTESIAN_POINT('Ctrl Pts',(374.040112152152,-10.4182036649417,-0.331011139607474));
#35272=CARTESIAN_POINT('Ctrl Pts',(374.037576901499,-10.4167612575597,-0.354706758597773));
#35273=CARTESIAN_POINT('Ctrl Pts',(374.03300251922,-10.4143894342811,-0.393399232292983));
#35274=CARTESIAN_POINT('Ctrl Pts',(374.03112009593,-10.4134649634536,-0.408413953272359));
#35275=CARTESIAN_POINT('Ctrl Pts',(374.027272268394,-10.4116692263162,-0.437447180121927));
#35276=CARTESIAN_POINT('Ctrl Pts',(374.025320104872,-10.4107983974421,-0.451467111277666));
#35277=CARTESIAN_POINT('Ctrl Pts',(374.020592119474,-10.4087777317335,-0.483858524143309));
#35278=CARTESIAN_POINT('Ctrl Pts',(374.017749679383,-10.4076258131369,-0.50221962942411));
#35279=CARTESIAN_POINT('Ctrl Pts',(374.007992449998,-10.4038641473306,-0.56183331753423));
#35280=CARTESIAN_POINT('Ctrl Pts',(374.000433510625,-10.4012341729069,-0.602974711503038));
#35281=CARTESIAN_POINT('Ctrl Pts',(373.952074777466,-10.3858717522614,-0.840110843280658));
#35282=CARTESIAN_POINT('Ctrl Pts',(373.893889855258,-10.3725864559325,-1.03208036171677));
#35283=CARTESIAN_POINT('Ctrl Pts',(373.738344645398,-10.3447968384968,-1.41334230820427));
#35284=CARTESIAN_POINT('Ctrl Pts',(373.639286716143,-10.330335908604,-1.60095872227118));
#35285=CARTESIAN_POINT('Ctrl Pts',(373.504422093613,-10.3145559849695,-1.80492113770066));
#35286=CARTESIAN_POINT('Ctrl Pts',(373.485882370986,-10.3124567905547,-1.83204879058598));
#35287=CARTESIAN_POINT('Ctrl Pts',(373.460000085102,-10.3096248813643,-1.86870402526228));
#35288=CARTESIAN_POINT('Ctrl Pts',(373.453014987551,-10.3088700582358,-1.87848003614963));
#35289=CARTESIAN_POINT('Ctrl Pts',(373.441200678865,-10.3076094346248,-1.89482081042498));
#35290=CARTESIAN_POINT('Ctrl Pts',(373.436400993078,-10.3071016596251,-1.90140666564402));
#35291=CARTESIAN_POINT('Ctrl Pts',(373.427225254403,-10.3061392992245,-1.91389727620356));
#35292=CARTESIAN_POINT('Ctrl Pts',(373.422853917679,-10.3056843855036,-1.91980536005951));
#35293=CARTESIAN_POINT('Ctrl Pts',(373.412420466632,-10.3046068780036,-1.93380627716237));
#35294=CARTESIAN_POINT('Ctrl Pts',(373.406340358575,-10.3039855212452,-1.9418856920961));
#35295=CARTESIAN_POINT('Ctrl Pts',(373.384736728914,-10.3018002408709,-1.9703137195946));
#35296=CARTESIAN_POINT('Ctrl Pts',(373.369008484605,-10.3002498480299,-1.99050649112826));
#35297=CARTESIAN_POINT('Ctrl Pts',(373.221344187678,-10.2860412327013,-2.17549705016967));
#35298=CARTESIAN_POINT('Ctrl Pts',(373.073736493984,-10.2743315392092,-2.32716795294932));
#35299=CARTESIAN_POINT('Ctrl Pts',(372.73967997459,-10.2498908493973,-2.60897218066535));
#35300=CARTESIAN_POINT('Ctrl Pts',(372.552215875762,-10.2371887553865,-2.73604641797113));
#35301=CARTESIAN_POINT('Ctrl Pts',(372.325154975338,-10.2217948018951,-2.85736247829873));
#35302=CARTESIAN_POINT('Ctrl Pts',(372.297073551525,-10.219892015444,-2.8718393613519));
#35303=CARTESIAN_POINT('Ctrl Pts',(372.253735470561,-10.2169548854607,-2.89338100158729));
#35304=CARTESIAN_POINT('Ctrl Pts',(372.238628322626,-10.2159309391726,-2.90074336707067));
#35305=CARTESIAN_POINT('Ctrl Pts',(372.21100942225,-10.2140584665893,-2.91393692714074));
#35306=CARTESIAN_POINT('Ctrl Pts',(372.198516402964,-10.2132112985569,-2.919806568779));
#35307=CARTESIAN_POINT('Ctrl Pts',(372.171159133501,-10.2113555883724,-2.93244603073415));
#35308=CARTESIAN_POINT('Ctrl Pts',(372.156280414326,-10.2103459586,-2.93918344156425));
#35309=CARTESIAN_POINT('Ctrl Pts',(372.115246014143,-10.2075601374036,-2.95739010904267));
#35310=CARTESIAN_POINT('Ctrl Pts',(372.088988578359,-10.2057760280703,-2.96862501802488));
#35311=CARTESIAN_POINT('Ctrl Pts',(371.940027992579,-10.1956436316819,-3.0300322916562));
#35312=CARTESIAN_POINT('Ctrl Pts',(371.814485154875,-10.1870545093825,-3.07293912366423));
#35313=CARTESIAN_POINT('Ctrl Pts',(371.476374945725,-10.1638304929175,-3.16566433186801));
#35314=CARTESIAN_POINT('Ctrl Pts',(371.260772581709,-10.1488966286129,-3.20184218662922));
#35315=CARTESIAN_POINT('Ctrl Pts',(370.93883539114,-10.1273226578798,-3.22275202845005));
#35316=CARTESIAN_POINT('Ctrl Pts',(370.834195735814,-10.1204322204589,-3.22444709406019));
#35317=CARTESIAN_POINT('Ctrl Pts',(370.712389506187,-10.1126839171305,-3.22048897732294));
#35318=CARTESIAN_POINT('Ctrl Pts',(370.695134128803,-10.1115926996635,-3.21978938696392));
#35319=CARTESIAN_POINT('Ctrl Pts',(370.668601244764,-10.1099255211121,-3.21849995426178));
#35320=CARTESIAN_POINT('Ctrl Pts',(370.659319576147,-10.1093443364125,-3.21800863237166));
#35321=CARTESIAN_POINT('Ctrl Pts',(370.642221066809,-10.1082775802635,-3.21702933213768));
#35322=CARTESIAN_POINT('Ctrl Pts',(370.634403892445,-10.107791392709,-3.21655301676784));
#35323=CARTESIAN_POINT('Ctrl Pts',(370.616667775857,-10.1066916878459,-3.21540741322286));
#35324=CARTESIAN_POINT('Ctrl Pts',(370.60675015163,-10.1060791456074,-3.21472072449741));
#35325=CARTESIAN_POINT('Ctrl Pts',(370.580981869276,-10.1044934584687,-3.21281670163236));
#35326=CARTESIAN_POINT('Ctrl Pts',(370.565136546395,-10.1035241410763,-3.21152794265536));
#35327=CARTESIAN_POINT('Ctrl Pts',(370.456599671647,-10.0969199898325,-3.20189128895898));
#35328=CARTESIAN_POINT('Ctrl Pts',(370.364289072983,-10.0914800973842,-3.18964812211196));
#35329=CARTESIAN_POINT('Ctrl Pts',(370.192049563125,-10.0814507214033,-3.15916216569419));
#35330=CARTESIAN_POINT('Ctrl Pts',(370.112038713102,-10.0768415896112,-3.14183513193206));
#35331=CARTESIAN_POINT('Ctrl Pts',(369.904123323024,-10.0648094668687,-3.08844578453568));
#35332=CARTESIAN_POINT('Ctrl Pts',(369.77764099103,-10.0574298816126,-3.04748954826187));
#35333=CARTESIAN_POINT('Ctrl Pts',(369.563073460735,-10.044368665128,-2.96304133064751));
#35334=CARTESIAN_POINT('Ctrl Pts',(369.473779898286,-10.0387612151918,-2.92311659164266));
#35335=CARTESIAN_POINT('Ctrl Pts',(369.348980086566,-10.0305711989814,-2.8603579670742));
#35336=CARTESIAN_POINT('Ctrl Pts',(369.311889355979,-10.0280909851026,-2.8407898943253));
#35337=CARTESIAN_POINT('Ctrl Pts',(369.246314092647,-10.0236153951195,-2.80454102964509));
#35338=CARTESIAN_POINT('Ctrl Pts',(369.217683754261,-10.0216296074474,-2.78813564939189));
#35339=CARTESIAN_POINT('Ctrl Pts',(369.174610866055,-10.0185910685047,-2.76256810203123));
#35340=CARTESIAN_POINT('Ctrl Pts',(369.159980489497,-10.0175498834542,-2.75372550856372));
#35341=CARTESIAN_POINT('Ctrl Pts',(369.133542900844,-10.0156514934899,-2.73745806241422));
#35342=CARTESIAN_POINT('Ctrl Pts',(369.121712151216,-10.0147957319319,-2.73007212027283));
#35343=CARTESIAN_POINT('Ctrl Pts',(369.096293196338,-10.0129433889968,-2.71397280922609));
#35344=CARTESIAN_POINT('Ctrl Pts',(369.082721815101,-10.0119458686376,-2.70523370917275));
#35345=CARTESIAN_POINT('Ctrl Pts',(369.046028282768,-10.0092252057127,-2.68121355074157));
#35346=CARTESIAN_POINT('Ctrl Pts',(369.023037096694,-10.0074947406822,-2.66573585270437));
#35347=CARTESIAN_POINT('Ctrl Pts',(368.903486427584,-9.99835798773544,-2.5829935325827));
#35348=CARTESIAN_POINT('Ctrl Pts',(368.810475589367,-9.99076416128919,-2.51078125963479));
#35349=CARTESIAN_POINT('Ctrl Pts',(368.548459215239,-9.96789807647326,-2.28332111387894));
#35350=CARTESIAN_POINT('Ctrl Pts',(368.391836290433,-9.952193870532,-2.11494035279609));
#35351=CARTESIAN_POINT('Ctrl Pts',(368.188816641251,-9.92950865905699,-1.84375328090339));
#35352=CARTESIAN_POINT('Ctrl Pts',(368.127707999806,-9.92228321129425,-1.75281801243335));
#35353=CARTESIAN_POINT('Ctrl Pts',(368.06236637864,-9.91421120829735,-1.64399105824542));
#35354=CARTESIAN_POINT('Ctrl Pts',(368.053512260778,-9.91310925728834,-1.62896957172511));
#35355=CARTESIAN_POINT('Ctrl Pts',(368.040108053289,-9.91142920358036,-1.60580079844673));
#35356=CARTESIAN_POINT('Ctrl Pts',(368.035470861427,-9.91084575397493,-1.59770464479745));
#35357=CARTESIAN_POINT('Ctrl Pts',(368.027007174854,-9.90977687864003,-1.58277781552506));
#35358=CARTESIAN_POINT('Ctrl Pts',(368.023170413075,-9.90929081829687,-1.57595334012942));
#35359=CARTESIAN_POINT('Ctrl Pts',(368.014539881358,-9.90819395160339,-1.5604703442929));
#35360=CARTESIAN_POINT('Ctrl Pts',(368.009761105403,-9.90758409848121,-1.55180368940004));
#35361=CARTESIAN_POINT('Ctrl Pts',(367.997481206433,-9.90601004980853,-1.52928854079146));
#35362=CARTESIAN_POINT('Ctrl Pts',(367.99004143927,-9.9050495896514,-1.51540664685358));
#35363=CARTESIAN_POINT('Ctrl Pts',(367.940998404392,-9.89866823344856,-1.42226340956446));
#35364=CARTESIAN_POINT('Ctrl Pts',(367.902607415758,-9.89342755858152,-1.34134543194303));
#35365=CARTESIAN_POINT('Ctrl Pts',(367.835175261897,-9.88351335012752,-1.18244024274981));
#35366=CARTESIAN_POINT('Ctrl Pts',(367.805686641122,-9.87882982640742,-1.10472407921425));
#35367=CARTESIAN_POINT('Ctrl Pts',(367.718492793758,-9.86347216751284,-0.845077957968715));
#35368=CARTESIAN_POINT('Ctrl Pts',(367.67393722504,-9.8529101072069,-0.659176161326178));
#35369=CARTESIAN_POINT('Ctrl Pts',(367.636668234636,-9.83819189763902,-0.406593296607283));
#35370=CARTESIAN_POINT('Ctrl Pts',(367.629169019626,-9.83442860254649,-0.342492924896701));
#35371=CARTESIAN_POINT('Ctrl Pts',(367.619620860445,-9.82788119238462,-0.232302480160832));
#35372=CARTESIAN_POINT('Ctrl Pts',(367.61662796937,-9.82512546604046,-0.186313413736238));
#35373=CARTESIAN_POINT('Ctrl Pts',(367.613772762875,-9.82115898221448,-0.12077984025312));
#35374=CARTESIAN_POINT('Ctrl Pts',(367.613100414752,-9.81997346498977,-0.101275055972246));
#35375=CARTESIAN_POINT('Ctrl Pts',(367.612243568114,-9.81791233101388,-0.0675137868352983));
#35376=CARTESIAN_POINT('Ctrl Pts',(367.611976438764,-9.81703931953154,-0.053259821080117));
#35377=CARTESIAN_POINT('Ctrl Pts',(367.611644812505,-9.81535567478545,-0.0258613429985518));
#35378=CARTESIAN_POINT('Ctrl Pts',(367.611566140869,-9.81454550279893,-0.0127172636289814));
#35379=CARTESIAN_POINT('Ctrl Pts',(367.611570707206,-9.81241346131295,0.0217649042256376));
#35380=CARTESIAN_POINT('Ctrl Pts',(367.611785455238,-9.81108750896086,0.043102053378294));
#35381=CARTESIAN_POINT('Ctrl Pts',(367.613372946402,-9.80612873477627,0.122485262543873));
#35382=CARTESIAN_POINT('Ctrl Pts',(367.616102304005,-9.80245402730413,0.180490194762853));
#35383=CARTESIAN_POINT('Ctrl Pts',(367.626917124544,-9.79308232685239,0.326295110971551));
#35384=CARTESIAN_POINT('Ctrl Pts',(367.637041018937,-9.7873275175316,0.41389202447117));
#35385=CARTESIAN_POINT('Ctrl Pts',(367.672936450188,-9.77203660827862,0.642006614529326));
#35386=CARTESIAN_POINT('Ctrl Pts',(367.704479436494,-9.76237855112307,0.781416477289189));
#35387=CARTESIAN_POINT('Ctrl Pts',(367.792269608571,-9.74153734005061,1.07675327426295));
#35388=CARTESIAN_POINT('Ctrl Pts',(367.851511979887,-9.73038293077823,1.23139540690404));
#35389=CARTESIAN_POINT('Ctrl Pts',(367.93393988401,-9.71802208414474,1.40522408116741));
#35390=CARTESIAN_POINT('Ctrl Pts',(367.945819220213,-9.71630156781658,1.42948341740365));
#35391=CARTESIAN_POINT('Ctrl Pts',(367.962663256538,-9.71394694087683,1.46281380006098));
#35392=CARTESIAN_POINT('Ctrl Pts',(367.967368326692,-9.71329798647084,1.47201384350399));
#35393=CARTESIAN_POINT('Ctrl Pts',(367.975521807922,-9.71218852023634,1.48776933477997));
#35394=CARTESIAN_POINT('Ctrl Pts',(367.97894868406,-9.71172669738386,1.49433574960594));
#35395=CARTESIAN_POINT('Ctrl Pts',(367.986166543092,-9.71076339135411,1.50805077795278));
#35396=CARTESIAN_POINT('Ctrl Pts',(367.989961851224,-9.7102622049316,1.51519700697216));
#35397=CARTESIAN_POINT('Ctrl Pts',(367.999323485461,-9.70903877182838,1.53266500482356));
#35398=CARTESIAN_POINT('Ctrl Pts',(368.004919381531,-9.70831837334509,1.54297095906417));
#35399=CARTESIAN_POINT('Ctrl Pts',(368.025447864189,-9.70571397135917,1.58029100742341));
#35400=CARTESIAN_POINT('Ctrl Pts',(368.040712612498,-9.70384982505603,1.60712171344446));
#35401=CARTESIAN_POINT('Ctrl Pts',(368.080012314441,-9.69921728940689,1.67394601553831));
#35402=CARTESIAN_POINT('Ctrl Pts',(368.104535207033,-9.69647456230415,1.71364564534499));
#35403=CARTESIAN_POINT('Ctrl Pts',(368.310114399419,-9.67452187568904,2.03083484222454));
#35404=CARTESIAN_POINT('Ctrl Pts',(368.532114510248,-9.65685728132207,2.27942790262382));
#35405=CARTESIAN_POINT('Ctrl Pts',(368.84065651892,-9.63352664798685,2.53299306624615));
#35406=CARTESIAN_POINT('Ctrl Pts',(368.894529132123,-9.62949968022464,2.57448210942296));
#35407=CARTESIAN_POINT('Ctrl Pts',(368.968635310251,-9.62399819829661,2.62790654137544));
#35408=CARTESIAN_POINT('Ctrl Pts',(368.987747753885,-9.62258265125986,2.6413714175596));
#35409=CARTESIAN_POINT('Ctrl Pts',(369.019388733511,-9.62024374373543,2.6631514954789));
#35410=CARTESIAN_POINT('Ctrl Pts',(369.031832172095,-9.61932506207504,2.67158921894026));
#35411=CARTESIAN_POINT('Ctrl Pts',(369.056140197593,-9.61753241040407,2.68782502318446));
#35412=CARTESIAN_POINT('Ctrl Pts',(369.067998189696,-9.6166588174323,2.6956323870706));
#35413=CARTESIAN_POINT('Ctrl Pts',(369.09598646403,-9.61459879470184,2.71379604515744));
#35414=CARTESIAN_POINT('Ctrl Pts',(369.112158186814,-9.61340997846805,2.72408719598076));
#35415=CARTESIAN_POINT('Ctrl Pts',(369.165775693384,-9.60947269531497,2.75753933919425));
#35416=CARTESIAN_POINT('Ctrl Pts',(369.203603019968,-9.60670160949175,2.78007643261634));
#35417=CARTESIAN_POINT('Ctrl Pts',(369.294714929813,-9.60003980452121,2.83186049374975));
#35418=CARTESIAN_POINT('Ctrl Pts',(369.348387050004,-9.59612535377562,2.86038806814491));
#35419=CARTESIAN_POINT('Ctrl Pts',(369.562553882867,-9.58054565408234,2.96656634793586));
#35420=CARTESIAN_POINT('Ctrl Pts',(369.72855644991,-9.56853335902953,3.03235530765771));
#35421=CARTESIAN_POINT('Ctrl Pts',(370.06818933598,-9.5445228591354,3.13534287379665));
#35422=CARTESIAN_POINT('Ctrl Pts',(370.241196925875,-9.53256978487021,3.1726246022994));
#35423=CARTESIAN_POINT('Ctrl Pts',(370.443092925915,-9.51948819719132,3.19902879411396));
#35424=CARTESIAN_POINT('Ctrl Pts',(370.469827870093,-9.51777358157234,3.2021850869973));
#35425=CARTESIAN_POINT('Ctrl Pts',(370.506864213815,-9.51542553403473,3.20608767752409));
#35426=CARTESIAN_POINT('Ctrl Pts',(370.517133515464,-9.51477736651232,3.20711992052349));
#35427=CARTESIAN_POINT('Ctrl Pts',(370.534777602471,-9.51366889113543,3.2088078802466));
#35428=CARTESIAN_POINT('Ctrl Pts',(370.542149939316,-9.51320727733466,3.20948754271655));
#35429=CARTESIAN_POINT('Ctrl Pts',(370.55758740504,-9.51224400184884,3.21085710385552));
#35430=CARTESIAN_POINT('Ctrl Pts',(370.565652880191,-9.51174263922369,3.21154203092224));
#35431=CARTESIAN_POINT('Ctrl Pts',(370.585424469277,-9.5105181091752,3.21314604719509));
#35432=CARTESIAN_POINT('Ctrl Pts',(370.597133334978,-9.50979679772263,3.21403157286778));
#35433=CARTESIAN_POINT('Ctrl Pts',(370.639739263711,-9.50718530738156,3.21701970180967));
#35434=CARTESIAN_POINT('Ctrl Pts',(370.67066246517,-9.5053151275566,3.2187410060747));
#35435=CARTESIAN_POINT('Ctrl Pts',(370.748431055638,-9.50066446460427,3.2219461884893));
#35436=CARTESIAN_POINT('Ctrl Pts',(370.795294039223,-9.49790990156003,3.2228545359463));
#35437=CARTESIAN_POINT('Ctrl Pts',(371.178835821806,-9.47563839904368,3.22192094910913));
#35438=CARTESIAN_POINT('Ctrl Pts',(371.513309657422,-9.45770673532695,3.16835561884218));
#35439=CARTESIAN_POINT('Ctrl Pts',(371.89387440878,-9.43426675632815,3.04425632251717));
#35440=CARTESIAN_POINT('Ctrl Pts',(371.953697459722,-9.43049587881588,3.02277110324761));
#35441=CARTESIAN_POINT('Ctrl Pts',(372.034054553671,-9.42529361814119,2.99119855187404));
#35442=CARTESIAN_POINT('Ctrl Pts',(372.055176222941,-9.42391314169579,2.98264005996886));
#35443=CARTESIAN_POINT('Ctrl Pts',(372.088586395174,-9.42170788983338,2.9686879293413));
#35444=CARTESIAN_POINT('Ctrl Pts',(372.100935289884,-9.42088805941205,2.96344020654134));
#35445=CARTESIAN_POINT('Ctrl Pts',(372.1261900843,-9.41920150914475,2.95252136632115));
#35446=CARTESIAN_POINT('Ctrl Pts',(372.139092248708,-9.41833453551171,2.94684238582082));
#35447=CARTESIAN_POINT('Ctrl Pts',(372.168855114058,-9.41632198277008,2.93350826462769));
#35448=CARTESIAN_POINT('Ctrl Pts',(372.185687796228,-9.41517433160365,2.92579214801831));
#35449=CARTESIAN_POINT('Ctrl Pts',(372.238567030593,-9.41153865911797,2.90099858233017));
#35450=CARTESIAN_POINT('Ctrl Pts',(372.274362404469,-9.40903266167922,2.88339729859175));
#35451=CARTESIAN_POINT('Ctrl Pts',(372.309820613642,-9.40650395365004,2.86513684952373));
#35452=CARTESIAN_POINT('',(367.611569056541,-9.56531811886281,0.00278495561203112));
#35453=CARTESIAN_POINT('Ctrl Pts',(372.309820498245,-9.15921048455976,2.86513690895142));
#35454=CARTESIAN_POINT('Ctrl Pts',(372.045257012626,-9.1761807693358,3.00138314611619));
#35455=CARTESIAN_POINT('Ctrl Pts',(371.762917332346,-9.19227741905944,3.10042508082463));
#35456=CARTESIAN_POINT('Ctrl Pts',(371.409521784279,-9.21339959172196,3.17161809370236));
#35457=CARTESIAN_POINT('Ctrl Pts',(371.347933050406,-9.2171080785855,3.18217214439677));
#35458=CARTESIAN_POINT('Ctrl Pts',(371.263654022811,-9.22223771045259,3.19410409845714));
#35459=CARTESIAN_POINT('Ctrl Pts',(371.241196293265,-9.22360982419175,3.19704245094925));
#35460=CARTESIAN_POINT('Ctrl Pts',(371.20540808486,-9.22580545168389,3.20134176463265));
#35461=CARTESIAN_POINT('Ctrl Pts',(371.192096606922,-9.226624105055,3.20285675747336));
#35462=CARTESIAN_POINT('Ctrl Pts',(371.164736113994,-9.22831101875315,3.20579798773435));
#35463=CARTESIAN_POINT('Ctrl Pts',(371.150686415713,-9.22917955072291,3.20721497374243));
#35464=CARTESIAN_POINT('Ctrl Pts',(371.118084588137,-9.23120046862997,3.21028673402436));
#35465=CARTESIAN_POINT('Ctrl Pts',(371.099526664826,-9.23235497512238,3.21187308862051));
#35466=CARTESIAN_POINT('Ctrl Pts',(371.040170063283,-9.23606134972561,3.21642903714309));
#35467=CARTESIAN_POINT('Ctrl Pts',(370.99932947443,-9.23863232352634,3.21878265825869));
#35468=CARTESIAN_POINT('Ctrl Pts',(370.903288161155,-9.24472955145762,3.22248487026863));
#35469=CARTESIAN_POINT('Ctrl Pts',(370.848077003594,-9.24827450458236,3.22319340830129));
#35470=CARTESIAN_POINT('Ctrl Pts',(370.642273076936,-9.26163718980462,3.22054681420285));
#35471=CARTESIAN_POINT('Ctrl Pts',(370.492005027425,-9.27170223664362,3.20805491508853));
#35472=CARTESIAN_POINT('Ctrl Pts',(370.128731790619,-9.29652023958033,3.15203830833367));
#35473=CARTESIAN_POINT('Ctrl Pts',(369.918161207519,-9.31134101637858,3.09739695999033));
#35474=CARTESIAN_POINT('Ctrl Pts',(369.690987179753,-9.32688091622255,3.01322922080392));
#35475=CARTESIAN_POINT('Ctrl Pts',(369.667408632598,-9.32848762481068,3.00417681376603));
#35476=CARTESIAN_POINT('Ctrl Pts',(369.634630697396,-9.33071012809269,2.99114837556744));
#35477=CARTESIAN_POINT('Ctrl Pts',(369.625340435998,-9.33133879928386,2.98740547756661));
#35478=CARTESIAN_POINT('Ctrl Pts',(369.609282630978,-9.33242306560802,2.98084886871542));
#35479=CARTESIAN_POINT('Ctrl Pts',(369.602507019862,-9.33287984087892,2.97805529619938));
#35480=CARTESIAN_POINT('Ctrl Pts',(369.588183845859,-9.33384378875778,2.97209263056451));
#35481=CARTESIAN_POINT('Ctrl Pts',(369.5806387121,-9.33435060094625,2.96891784709778));
#35482=CARTESIAN_POINT('Ctrl Pts',(369.562225366736,-9.3355852448794,2.96108731021022));
#35483=CARTESIAN_POINT('Ctrl Pts',(369.551370404249,-9.33631121212037,2.95640037987552));
#35484=CARTESIAN_POINT('Ctrl Pts',(369.511122356572,-9.33899685227492,2.93875875058399));
#35485=CARTESIAN_POINT('Ctrl Pts',(369.48189657857,-9.34093486285725,2.92542410440424));
#35486=CARTESIAN_POINT('Ctrl Pts',(369.269694971775,-9.35495168008341,2.82474434340459));
#35487=CARTESIAN_POINT('Ctrl Pts',(369.095102702806,-9.36620412274226,2.72073088868787));
#35488=CARTESIAN_POINT('Ctrl Pts',(368.762048351349,-9.38928181707787,2.47706719861769));
#35489=CARTESIAN_POINT('Ctrl Pts',(368.60519808438,-9.40107375287663,2.33691560534751));
#35490=CARTESIAN_POINT('Ctrl Pts',(368.437609907184,-9.41576388976557,2.15483741495324));
#35491=CARTESIAN_POINT('Ctrl Pts',(368.412616446288,-9.41801623037446,2.1267099904393));
#35492=CARTESIAN_POINT('Ctrl Pts',(368.374817993984,-9.42152323709554,2.08264149184215));
#35493=CARTESIAN_POINT('Ctrl Pts',(368.361662146937,-9.42276349489443,2.06700480639254));
#35494=CARTESIAN_POINT('Ctrl Pts',(368.339561175187,-9.42488135398421,2.04022323842938));
#35495=CARTESIAN_POINT('Ctrl Pts',(368.33053974323,-9.42575583124762,2.02914191489885));
#35496=CARTESIAN_POINT('Ctrl Pts',(368.312418926522,-9.42753292676025,2.00657867791763));
#35497=CARTESIAN_POINT('Ctrl Pts',(368.303323552697,-9.42843567636029,1.99509398941074));
#35498=CARTESIAN_POINT('Ctrl Pts',(368.281058585542,-9.43067261123724,1.96658282419045));
#35499=CARTESIAN_POINT('Ctrl Pts',(368.267980818051,-9.43201038196785,1.94948584971037));
#35500=CARTESIAN_POINT('Ctrl Pts',(368.219489336903,-9.43706244657457,1.88475785590913));
#35501=CARTESIAN_POINT('Ctrl Pts',(368.185224204153,-9.44082068097463,1.8362849549399));
#35502=CARTESIAN_POINT('Ctrl Pts',(368.062071945621,-9.45506814848143,1.65144250113473));
#35503=CARTESIAN_POINT('Ctrl Pts',(367.982227781839,-9.46586991942624,1.50936400519982));
#35504=CARTESIAN_POINT('Ctrl Pts',(367.864051718674,-9.48471106711013,1.2559092634263));
#35505=CARTESIAN_POINT('Ctrl Pts',(367.820445302843,-9.4926537294396,1.14732780257992));
#35506=CARTESIAN_POINT('Ctrl Pts',(367.741564502796,-9.50915225145384,0.91512703877353));
#35507=CARTESIAN_POINT('Ctrl Pts',(367.707580597534,-9.51767828594383,0.791266189145504));
#35508=CARTESIAN_POINT('Ctrl Pts',(367.677603031087,-9.52691986021442,0.649269564824457));
#35509=CARTESIAN_POINT('Ctrl Pts',(367.674263381166,-9.52798273049701,0.632815294994851));
#35510=CARTESIAN_POINT('Ctrl Pts',(367.669120366267,-9.52967413850922,0.606419399754992));
#35511=CARTESIAN_POINT('Ctrl Pts',(367.667234947006,-9.53030704156733,0.596494334808006));
#35512=CARTESIAN_POINT('Ctrl Pts',(367.663964748241,-9.53142798766573,0.578826924144435));
#35513=CARTESIAN_POINT('Ctrl Pts',(367.662561602145,-9.53191704814549,0.571088177873209));
#35514=CARTESIAN_POINT('Ctrl Pts',(367.659894291716,-9.53286271346055,0.556064100408563));
#35515=CARTESIAN_POINT('Ctrl Pts',(367.658626870661,-9.53331951156078,0.548779570916097));
#35516=CARTESIAN_POINT('Ctrl Pts',(367.655872944471,-9.53432903539977,0.532622247088352));
#35517=CARTESIAN_POINT('Ctrl Pts',(367.654398493157,-9.53488109326968,0.52374742383042));
#35518=CARTESIAN_POINT('Ctrl Pts',(367.650816443817,-9.53625206580573,0.501613961626277));
#35519=CARTESIAN_POINT('Ctrl Pts',(367.64875447149,-9.5370685638991,0.488347975274731));
#35520=CARTESIAN_POINT('Ctrl Pts',(367.623475330361,-9.54744592060516,0.318734098999937));
#35521=CARTESIAN_POINT('Ctrl Pts',(367.611705674635,-9.55643615325176,0.160879323418296));
#35522=CARTESIAN_POINT('Ctrl Pts',(367.611569056541,-9.56531811886281,0.00278495561203112));
#35523=CARTESIAN_POINT('Ctrl Pts',(367.611569059112,-9.56531795180948,0.00278792907424184));
#35524=CARTESIAN_POINT('Ctrl Pts',(367.611374172123,-9.57797464776861,-0.222494634597293));
#35525=CARTESIAN_POINT('Ctrl Pts',(367.634800609163,-9.59038930068433,-0.44717314711833));
#35526=CARTESIAN_POINT('Ctrl Pts',(367.69778522171,-9.60806751235912,-0.744637333014133));
#35527=CARTESIAN_POINT('Ctrl Pts',(367.716919768297,-9.61271842768905,-0.821066016533812));
#35528=CARTESIAN_POINT('Ctrl Pts',(367.745464853836,-9.61889374241953,-0.919604653320842));
#35529=CARTESIAN_POINT('Ctrl Pts',(367.752349822658,-9.62033628917451,-0.942421658366697));
#35530=CARTESIAN_POINT('Ctrl Pts',(367.764021323441,-9.62270873649172,-0.979605026105658));
#35531=CARTESIAN_POINT('Ctrl Pts',(367.768657233967,-9.62363369382537,-0.994017979332718));
#35532=CARTESIAN_POINT('Ctrl Pts',(367.777827397613,-9.6254306631561,-1.0218533985905));
#35533=CARTESIAN_POINT('Ctrl Pts',(367.782348948311,-9.62630223914439,-1.03527970457614));
#35534=CARTESIAN_POINT('Ctrl Pts',(367.793012022966,-9.6283250692593,-1.06626566159175));
#35535=CARTESIAN_POINT('Ctrl Pts',(367.799217306512,-9.62947841237908,-1.08380268607457));
#35536=CARTESIAN_POINT('Ctrl Pts',(367.819895569708,-9.63324669919461,-1.14067187016413));
#35537=CARTESIAN_POINT('Ctrl Pts',(367.834983546852,-9.63588195686505,-1.17977433081536));
#35538=CARTESIAN_POINT('Ctrl Pts',(367.928309995146,-9.6515501820604,-1.40827034991521));
#35539=CARTESIAN_POINT('Ctrl Pts',(368.023693893456,-9.66516478128069,-1.5901178178407));
#35540=CARTESIAN_POINT('Ctrl Pts',(368.224719601683,-9.68999659920125,-1.89806525664835));
#35541=CARTESIAN_POINT('Ctrl Pts',(368.323984258249,-9.70108602589383,-2.02753141354491));
#35542=CARTESIAN_POINT('Ctrl Pts',(368.463638879596,-9.71490781374781,-2.18361246233849));
#35543=CARTESIAN_POINT('Ctrl Pts',(368.495411016946,-9.71794806548861,-2.21761074822583));
#35544=CARTESIAN_POINT('Ctrl Pts',(368.549180301427,-9.72290801528488,-2.27270574216118));
#35545=CARTESIAN_POINT('Ctrl Pts',(368.570759642753,-9.7248517069936,-2.29419907715357));
#35546=CARTESIAN_POINT('Ctrl Pts',(368.600898333283,-9.72749855066466,-2.32337833674725));
#35547=CARTESIAN_POINT('Ctrl Pts',(368.609198208362,-9.72822054925767,-2.33132842455728));
#35548=CARTESIAN_POINT('Ctrl Pts',(368.623484941243,-9.72945127667924,-2.34486725976424));
#35549=CARTESIAN_POINT('Ctrl Pts',(368.629450846296,-9.72996165005176,-2.35047784858138));
#35550=CARTESIAN_POINT('Ctrl Pts',(368.640793788178,-9.73092518988405,-2.36106404071736));
#35551=CARTESIAN_POINT('Ctrl Pts',(368.64616649649,-9.73137871007436,-2.36604413966812));
#35552=CARTESIAN_POINT('Ctrl Pts',(368.658915646814,-9.7324482530211,-2.37778108051946));
#35553=CARTESIAN_POINT('Ctrl Pts',(368.666306708626,-9.73306308458857,-2.38452202958564));
#35554=CARTESIAN_POINT('Ctrl Pts',(368.692226065064,-9.7352015783609,-2.40794140055877));
#35555=CARTESIAN_POINT('Ctrl Pts',(368.710916919099,-9.73671246115249,-2.42443964176917));
#35556=CARTESIAN_POINT('Ctrl Pts',(368.896608023939,-9.75144086370525,-2.58455249254069));
#35557=CARTESIAN_POINT('Ctrl Pts',(369.077748129916,-9.76361956425793,-2.71092623051227));
#35558=CARTESIAN_POINT('Ctrl Pts',(369.400251270259,-9.78425412023531,-2.88991875753721));
#35559=CARTESIAN_POINT('Ctrl Pts',(369.534936453644,-9.79259969663299,-2.95292751441202));
#35560=CARTESIAN_POINT('Ctrl Pts',(369.724555575888,-9.8043964067138,-3.02614327457104));
#35561=CARTESIAN_POINT('Ctrl Pts',(369.776125144813,-9.80760796278115,-3.04455959784097));
#35562=CARTESIAN_POINT('Ctrl Pts',(369.866750065077,-9.81327506245225,-3.0743425559846));
#35563=CARTESIAN_POINT('Ctrl Pts',(369.905598519424,-9.81571165623632,-3.08630033412424));
#35564=CARTESIAN_POINT('Ctrl Pts',(369.96251776364,-9.81929679522666,-3.10264843581423));
#35565=CARTESIAN_POINT('Ctrl Pts',(369.980417775942,-9.82042639985378,-3.10762245906316));
#35566=CARTESIAN_POINT('Ctrl Pts',(370.011990510846,-9.8224230379357,-3.11610245536534));
#35567=CARTESIAN_POINT('Ctrl Pts',(370.02564524214,-9.82328792667124,-3.11967392020961));
#35568=CARTESIAN_POINT('Ctrl Pts',(370.052320829798,-9.82498040758377,-3.12646415508091));
#35569=CARTESIAN_POINT('Ctrl Pts',(370.065339203983,-9.8258077006709,-3.12969156403486));
#35570=CARTESIAN_POINT('Ctrl Pts',(370.100470566911,-9.82804396550752,-3.13816861563279));
#35571=CARTESIAN_POINT('Ctrl Pts',(370.122619248991,-9.8294578027969,-3.14326568301474));
#35572=CARTESIAN_POINT('Ctrl Pts',(370.20639766189,-9.83482168440393,-3.1616147065844));
#35573=CARTESIAN_POINT('Ctrl Pts',(370.268354463503,-9.83882130925147,-3.17329101536853));
#35574=CARTESIAN_POINT('Ctrl Pts',(370.663833344441,-9.86457327862878,-3.23587245037377));
#35575=CARTESIAN_POINT('Ctrl Pts',(371.003175169231,-9.88797134872904,-3.23594515554636));
#35576=CARTESIAN_POINT('Ctrl Pts',(371.382626258822,-9.91332884128186,-3.17610992980054));
#35577=CARTESIAN_POINT('Ctrl Pts',(371.428783103526,-9.91639373590926,-3.16779543322743));
#35578=CARTESIAN_POINT('Ctrl Pts',(371.505112546398,-9.92141230563556,-3.15231854201093));
#35579=CARTESIAN_POINT('Ctrl Pts',(371.535391762622,-9.92338995150959,-3.14572300899859));
#35580=CARTESIAN_POINT('Ctrl Pts',(371.577015853217,-9.92608599487546,-3.13602539911766));
#35581=CARTESIAN_POINT('Ctrl Pts',(371.588444844284,-9.92682390219903,-3.13329668472403));
#35582=CARTESIAN_POINT('Ctrl Pts',(371.607727217903,-9.92806456578325,-3.12858132873243));
#35583=CARTESIAN_POINT('Ctrl Pts',(371.615588434331,-9.92856916058394,-3.12662748981293));
#35584=CARTESIAN_POINT('Ctrl Pts',(371.630626284116,-9.92953198287824,-3.12282970169105));
#35585=CARTESIAN_POINT('Ctrl Pts',(371.63780401275,-9.92999049594136,-3.12099062109069));
#35586=CARTESIAN_POINT('Ctrl Pts',(371.654973568019,-9.93108490456682,-3.11652827285055));
#35587=CARTESIAN_POINT('Ctrl Pts',(371.664959322165,-9.93171947333414,-3.11388166675038));
#35588=CARTESIAN_POINT('Ctrl Pts',(371.700951407435,-9.93400025499506,-3.10415693222677));
#35589=CARTESIAN_POINT('Ctrl Pts',(371.726882234413,-9.93563133836677,-3.09680043114646));
#35590=CARTESIAN_POINT('Ctrl Pts',(371.913329200562,-9.94729156433648,-3.04136940572132));
#35591=CARTESIAN_POINT('Ctrl Pts',(372.069991842799,-9.95673397126023,-2.98116031299773));
#35592=CARTESIAN_POINT('Ctrl Pts',(372.36225415704,-9.974866370819,-2.84181648196921));
#35593=CARTESIAN_POINT('Ctrl Pts',(372.498157510861,-9.98354246735299,-2.76444311621066));
#35594=CARTESIAN_POINT('Ctrl Pts',(372.726821603085,-9.99927457473014,-2.61126799175011));
#35595=CARTESIAN_POINT('Ctrl Pts',(372.821975521353,-10.0062104834711,-2.53958725327049));
#35596=CARTESIAN_POINT('Ctrl Pts',(372.933639845739,-10.0149801859474,-2.44534219248962));
#35597=CARTESIAN_POINT('Ctrl Pts',(372.954118023159,-10.0166160344453,-2.42761167368367));
#35598=CARTESIAN_POINT('Ctrl Pts',(372.986221582983,-10.019226053939,-2.39909965590004));
#35599=CARTESIAN_POINT('Ctrl Pts',(372.997995369783,-10.020193201105,-2.3884866362171));
#35600=CARTESIAN_POINT('Ctrl Pts',(373.02001097942,-10.0220207526901,-2.36834515925642));
#35601=CARTESIAN_POINT('Ctrl Pts',(373.030270020756,-10.0228803269618,-2.35883600604154));
#35602=CARTESIAN_POINT('Ctrl Pts',(373.053244311182,-10.0248234940531,-2.3372612573991));
#35603=CARTESIAN_POINT('Ctrl Pts',(373.065923603716,-10.0259086865919,-2.32515818087744));
#35604=CARTESIAN_POINT('Ctrl Pts',(373.098187844792,-10.0287034922108,-2.29385319618085));
#35605=CARTESIAN_POINT('Ctrl Pts',(373.117627226727,-10.0304195068655,-2.27450391394032));
#35606=CARTESIAN_POINT('Ctrl Pts',(373.284265463584,-10.0454153790246,-2.10434879572518));
#35607=CARTESIAN_POINT('Ctrl Pts',(373.416564719196,-10.0593409399028,-1.93971627864066));
#35608=CARTESIAN_POINT('Ctrl Pts',(373.651396583044,-10.0882791371823,-1.58048469338463));
#35609=CARTESIAN_POINT('Ctrl Pts',(373.752052765583,-10.1032334677743,-1.38589249067822));
#35610=CARTESIAN_POINT('Ctrl Pts',(373.844460532,-10.1194904834031,-1.15163655282704));
#35611=CARTESIAN_POINT('Ctrl Pts',(373.856195998022,-10.1216179767421,-1.12048131483597));
#35612=CARTESIAN_POINT('Ctrl Pts',(373.871530035646,-10.1244818011271,-1.07777812000613));
#35613=CARTESIAN_POINT('Ctrl Pts',(373.875549048358,-10.1252408620281,-1.06638470808806));
#35614=CARTESIAN_POINT('Ctrl Pts',(373.882177433506,-10.126506833729,-1.04725175619422));
#35615=CARTESIAN_POINT('Ctrl Pts',(373.884821597103,-10.1270157512751,-1.03952449469791));
#35616=CARTESIAN_POINT('Ctrl Pts',(373.889787834812,-10.1279789770894,-1.02482910646506));
#35617=CARTESIAN_POINT('Ctrl Pts',(373.892115501845,-10.1284336228179,-1.01786298119242));
#35618=CARTESIAN_POINT('Ctrl Pts',(373.897580781238,-10.1295088795441,-1.00131881883271));
#35619=CARTESIAN_POINT('Ctrl Pts',(373.900697338943,-10.1301282682982,-0.991733834724223));
#35620=CARTESIAN_POINT('Ctrl Pts',(373.911501526658,-10.1322982459361,-0.957967650593053));
#35621=CARTESIAN_POINT('Ctrl Pts',(373.918948724475,-10.133835556711,-0.933709729210991));
#35622=CARTESIAN_POINT('Ctrl Pts',(373.987230439323,-10.148364916497,-0.701555786713309));
#35623=CARTESIAN_POINT('Ctrl Pts',(374.027253650709,-10.1603562817405,-0.488083311405805));
#35624=CARTESIAN_POINT('Ctrl Pts',(374.058277074835,-10.180902539974,-0.122069923036281));
#35625=CARTESIAN_POINT('Ctrl Pts',(374.060458474449,-10.1893611934321,0.0287453736501252));
#35626=CARTESIAN_POINT('Ctrl Pts',(374.049014956875,-10.2013043954855,0.234284410818763));
#35627=CARTESIAN_POINT('Ctrl Pts',(374.044529051576,-10.2045423556791,0.28932719662586));
#35628=CARTESIAN_POINT('Ctrl Pts',(374.034261754948,-10.2102519365239,0.38490303560071));
#35629=CARTESIAN_POINT('Ctrl Pts',(374.029117919296,-10.2127042034623,0.425492222881452));
#35630=CARTESIAN_POINT('Ctrl Pts',(374.02050981543,-10.2163081856516,0.48440199315364));
#35631=CARTESIAN_POINT('Ctrl Pts',(374.017656946779,-10.2174406721144,0.502808814423645));
#35632=CARTESIAN_POINT('Ctrl Pts',(374.012361021227,-10.2194406145943,0.535124837384966));
#35633=CARTESIAN_POINT('Ctrl Pts',(374.0099857848,-10.220305902641,0.549044759218781));
#35634=CARTESIAN_POINT('Ctrl Pts',(374.005178966445,-10.2219978115404,0.576139606670014));
#35635=CARTESIAN_POINT('Ctrl Pts',(374.002756558398,-10.2228241244243,0.589315881866638));
#35636=CARTESIAN_POINT('Ctrl Pts',(373.996018285707,-10.2250543869519,0.624724611938763));
#35637=CARTESIAN_POINT('Ctrl Pts',(373.991550167995,-10.2264631555314,0.646926992828327));
#35638=CARTESIAN_POINT('Ctrl Pts',(373.973879958686,-10.2317858144228,0.730184416723781));
#35639=CARTESIAN_POINT('Ctrl Pts',(373.959138398811,-10.2357483110284,0.790895179689501));
#35640=CARTESIAN_POINT('Ctrl Pts',(373.853357065961,-10.2615007859608,1.17720564480226));
#35641=CARTESIAN_POINT('Ctrl Pts',(373.713353147188,-10.2849481191647,1.48710594764328));
#35642=CARTESIAN_POINT('Ctrl Pts',(373.50202844593,-10.3103542115884,1.80876727923314));
#35643=CARTESIAN_POINT('Ctrl Pts',(373.47541192508,-10.3134208875347,1.84741479583875));
#35644=CARTESIAN_POINT('Ctrl Pts',(373.429823611049,-10.3184420490098,1.91060942439129));
#35645=CARTESIAN_POINT('Ctrl Pts',(373.411324969121,-10.3204205348764,1.93548779416751));
#35646=CARTESIAN_POINT('Ctrl Pts',(373.385321920382,-10.3231175229761,1.96942476815169));
#35647=CARTESIAN_POINT('Ctrl Pts',(373.378123282078,-10.3238555524564,1.97871413252315));
#35648=CARTESIAN_POINT('Ctrl Pts',(373.365876989178,-10.325096361632,1.99433987151783));
#35649=CARTESIAN_POINT('Ctrl Pts',(373.36085600536,-10.3256009808318,2.00069691678825));
#35650=CARTESIAN_POINT('Ctrl Pts',(373.351196847659,-10.3265638028315,2.01283198111394));
#35651=CARTESIAN_POINT('Ctrl Pts',(373.346562662281,-10.3270222915113,2.01861300867648));
#35652=CARTESIAN_POINT('Ctrl Pts',(373.335420496608,-10.3281165813806,2.03241477382579));
#35653=CARTESIAN_POINT('Ctrl Pts',(373.328893765864,-10.3287510564248,2.04042036561849));
#35654=CARTESIAN_POINT('Ctrl Pts',(373.30520493142,-10.3310310535965,2.06919317853767));
#35655=CARTESIAN_POINT('Ctrl Pts',(373.287820541963,-10.3326614601318,2.08977702812144));
#35656=CARTESIAN_POINT('Ctrl Pts',(373.15952684514,-10.344407321397,2.23787407789459));
#35657=CARTESIAN_POINT('Ctrl Pts',(373.038984139717,-10.3539256374363,2.35672182770263));
#35658=CARTESIAN_POINT('Ctrl Pts',(372.795555062396,-10.3717421407932,2.56162280161342));
#35659=CARTESIAN_POINT('Ctrl Pts',(372.674920444555,-10.380031876609,2.64963073928684));
#35660=CARTESIAN_POINT('Ctrl Pts',(372.470981900944,-10.3937737300137,2.77774310757113));
#35661=CARTESIAN_POINT('Ctrl Pts',(372.391306039511,-10.3990793543797,2.82317307133056));
#35662=CARTESIAN_POINT('Ctrl Pts',(372.30982057914,-10.4044982614434,2.86513686729151));
#35663=CARTESIAN_POINT('Origin',(370.834317853224,2.31077344927308,0.));
#35664=CARTESIAN_POINT('',(372.3098206137,-11.9006401642978,2.86513684949388));
#35665=CARTESIAN_POINT('',(372.309820451737,-11.6561638218248,2.86513693290212));
#35666=CARTESIAN_POINT('',(372.309820613641,2.31077344927308,2.86513684952399));
#35667=CARTESIAN_POINT('',(367.611569193008,-11.0603970329327,-0.00293863513896361));
#35668=CARTESIAN_POINT('Ctrl Pts',(372.3098206137,-11.9006401642978,2.86513684949403));
#35669=CARTESIAN_POINT('Ctrl Pts',(372.320887123176,-11.8998481329448,2.85943776210708));
#35670=CARTESIAN_POINT('Ctrl Pts',(372.331920823068,-11.8990595518313,2.85367445082586));
#35671=CARTESIAN_POINT('Ctrl Pts',(372.352050304904,-11.8976232943015,2.84301116710232));
#35672=CARTESIAN_POINT('Ctrl Pts',(372.361156299895,-11.8969744795422,2.83813119072117));
#35673=CARTESIAN_POINT('Ctrl Pts',(372.376749767643,-11.8958651891777,2.82967775603535));
#35674=CARTESIAN_POINT('Ctrl Pts',(372.383248611172,-11.8954034034494,2.82612560289196));
#35675=CARTESIAN_POINT('Ctrl Pts',(372.396822359976,-11.8944401029819,2.81864554514496));
#35676=CARTESIAN_POINT('Ctrl Pts',(372.403894794462,-11.8939388854061,2.8147133548693));
#35677=CARTESIAN_POINT('Ctrl Pts',(372.421182455932,-11.8927152581753,2.80501619919042));
#35678=CARTESIAN_POINT('Ctrl Pts',(372.431381290609,-11.8919946980927,2.79922195116702));
#35679=CARTESIAN_POINT('Ctrl Pts',(372.468317846365,-11.8893890426104,2.77796965773682));
#35680=CARTESIAN_POINT('Ctrl Pts',(372.494865584004,-11.8875238294583,2.76218261350526));
#35681=CARTESIAN_POINT('Ctrl Pts',(372.560968328264,-11.8828880900452,2.72157598524606));
#35682=CARTESIAN_POINT('Ctrl Pts',(372.600219457421,-11.8801432714929,2.6962732912217));
#35683=CARTESIAN_POINT('Ctrl Pts',(372.914185345415,-11.858135406756,2.48408101525441));
#35684=CARTESIAN_POINT('Ctrl Pts',(373.159046879565,-11.8404246156689,2.25658614530807));
#35685=CARTESIAN_POINT('Ctrl Pts',(373.406444320867,-11.8170756250387,1.94288448731513));
#35686=CARTESIAN_POINT('Ctrl Pts',(373.446399812459,-11.8130933742174,1.88882545267499));
#35687=CARTESIAN_POINT('Ctrl Pts',(373.497878856238,-11.8076439902955,1.81441513298575));
#35688=CARTESIAN_POINT('Ctrl Pts',(373.510915383146,-11.8062343715419,1.79512816001135));
#35689=CARTESIAN_POINT('Ctrl Pts',(373.532013544191,-11.8039027221997,1.7631735337854));
#35690=CARTESIAN_POINT('Ctrl Pts',(373.540197769463,-11.8029853124016,1.7505875637137));
#35691=CARTESIAN_POINT('Ctrl Pts',(373.555955413499,-11.8011932870378,1.72598041924931));
#35692=CARTESIAN_POINT('Ctrl Pts',(373.56353787497,-11.8003190349298,1.71396542548348));
#35693=CARTESIAN_POINT('Ctrl Pts',(373.581195374352,-11.7982545362831,1.68557148020296));
#35694=CARTESIAN_POINT('Ctrl Pts',(373.59120366744,-11.7970618735664,1.66915185427608));
#35695=CARTESIAN_POINT('Ctrl Pts',(373.623824617233,-11.7930984108247,1.61454003267695));
#35696=CARTESIAN_POINT('Ctrl Pts',(373.645794435294,-11.7903045755265,1.57597164213616));
#35697=CARTESIAN_POINT('Ctrl Pts',(373.696249952073,-11.7835778788395,1.48298151272684));
#35698=CARTESIAN_POINT('Ctrl Pts',(373.723989222069,-11.7796206649567,1.42817649355118));
#35699=CARTESIAN_POINT('Ctrl Pts',(373.827562443791,-11.7637645441808,1.20815739692203));
#35700=CARTESIAN_POINT('Ctrl Pts',(373.890920561161,-11.7515047564412,1.03746052311287));
#35701=CARTESIAN_POINT('Ctrl Pts',(373.94951301404,-11.7366911101456,0.826476367141626));
#35702=CARTESIAN_POINT('Ctrl Pts',(373.958854224937,-11.7341727228967,0.790428091315009));
#35703=CARTESIAN_POINT('Ctrl Pts',(374.002145409845,-11.7216896197043,0.61058522475395));
#35704=CARTESIAN_POINT('Ctrl Pts',(374.02680766142,-11.7118127780099,0.46471972060924));
#35705=CARTESIAN_POINT('Ctrl Pts',(374.043205344678,-11.701216983972,0.299171989120469));
#35706=CARTESIAN_POINT('Ctrl Pts',(374.044876944958,-11.7000411585449,0.280665580748561));
#35707=CARTESIAN_POINT('Ctrl Pts',(374.047176649361,-11.698265043123,0.252487260352363));
#35708=CARTESIAN_POINT('Ctrl Pts',(374.04792131143,-11.697658598335,0.242825615839519));
#35709=CARTESIAN_POINT('Ctrl Pts',(374.049188255117,-11.696567067973,0.225359789170082));
#35710=CARTESIAN_POINT('Ctrl Pts',(374.049725711691,-11.6960811634039,0.217556987121091));
#35711=CARTESIAN_POINT('Ctrl Pts',(374.050853697834,-11.6950080265341,0.200262710367463));
#35712=CARTESIAN_POINT('Ctrl Pts',(374.051430626296,-11.6944215550342,0.190770552149279));
#35713=CARTESIAN_POINT('Ctrl Pts',(374.0529944711,-11.6927135537238,0.163012293398545));
#35714=CARTESIAN_POINT('Ctrl Pts',(374.053867914116,-11.6915981309754,0.144739833031209));
#35715=CARTESIAN_POINT('Ctrl Pts',(374.0602777455,-11.6817059299301,-0.0184841254605742));
#35716=CARTESIAN_POINT('Ctrl Pts',(374.056177975124,-11.6734077790748,-0.163666974720797));
#35717=CARTESIAN_POINT('Ctrl Pts',(374.020101455934,-11.6521452406507,-0.539307437473672));
#35718=CARTESIAN_POINT('Ctrl Pts',(373.972967030071,-11.6393917575428,-0.767429847222778));
#35719=CARTESIAN_POINT('Ctrl Pts',(373.876220794709,-11.6211040583421,-1.06764085759085));
#35720=CARTESIAN_POINT('Ctrl Pts',(373.847667164305,-11.6162059588548,-1.14575508753241));
#35721=CARTESIAN_POINT('Ctrl Pts',(373.806587126127,-11.6096961468074,-1.24593950358361));
#35722=CARTESIAN_POINT('Ctrl Pts',(373.79677531661,-11.6081755580457,-1.26909243171847));
#35723=CARTESIAN_POINT('Ctrl Pts',(373.780511556818,-11.6057077318139,-1.30625341323168));
#35724=CARTESIAN_POINT('Ctrl Pts',(373.774228121332,-11.6047662456154,-1.32033439749536));
#35725=CARTESIAN_POINT('Ctrl Pts',(373.762022319352,-11.6029596010847,-1.34716807228741));
#35726=CARTESIAN_POINT('Ctrl Pts',(373.756117055158,-11.6020950468478,-1.35992818545921));
#35727=CARTESIAN_POINT('Ctrl Pts',(373.742354477998,-11.6001015105034,-1.38916294770131));
#35728=CARTESIAN_POINT('Ctrl Pts',(373.734440383379,-11.5989705825393,-1.40561018579794));
#35729=CARTESIAN_POINT('Ctrl Pts',(373.709214757367,-11.59541285945,-1.45691456002696));
#35730=CARTESIAN_POINT('Ctrl Pts',(373.691411772917,-11.5929690394266,-1.4915248458353));
#35731=CARTESIAN_POINT('Ctrl Pts',(373.598925939798,-11.5805931954734,-1.66358943624273));
#35732=CARTESIAN_POINT('Ctrl Pts',(373.514941732477,-11.5703344507448,-1.79578151136795));
#35733=CARTESIAN_POINT('Ctrl Pts',(373.327868312766,-11.5493287222662,-2.04770533943167));
#35734=CARTESIAN_POINT('Ctrl Pts',(373.224901291494,-11.5386075605444,-2.16702551988096));
#35735=CARTESIAN_POINT('Ctrl Pts',(373.026757717973,-11.5197721560197,-2.36525402913432));
#35736=CARTESIAN_POINT('Ctrl Pts',(372.934970722332,-11.5116206078163,-2.44713777501089));
#35737=CARTESIAN_POINT('Ctrl Pts',(372.825647998361,-11.5027313277034,-2.53396932714878));
#35738=CARTESIAN_POINT('Ctrl Pts',(372.812493815498,-11.5016744889197,-2.54425159674552));
#35739=CARTESIAN_POINT('Ctrl Pts',(372.791277347711,-11.4999910379849,-2.5605719142001));
#35740=CARTESIAN_POINT('Ctrl Pts',(372.783265826697,-11.4993601195465,-2.56667504642992));
#35741=CARTESIAN_POINT('Ctrl Pts',(372.768953868342,-11.4982416866483,-2.57747216764089));
#35742=CARTESIAN_POINT('Ctrl Pts',(372.76266472158,-11.4977531676548,-2.58218079265951));
#35743=CARTESIAN_POINT('Ctrl Pts',(372.749069224202,-11.4967035164074,-2.59228223947809));
#35744=CARTESIAN_POINT('Ctrl Pts',(372.741757275658,-11.4961429219943,-2.59766719890255));
#35745=CARTESIAN_POINT('Ctrl Pts',(372.72127863592,-11.4945834996618,-2.61261581279615));
#35746=CARTESIAN_POINT('Ctrl Pts',(372.708061914113,-11.4935892623801,-2.62211090543475));
#35747=CARTESIAN_POINT('Ctrl Pts',(372.628035154467,-11.4876385322912,-2.678689250818));
#35748=CARTESIAN_POINT('Ctrl Pts',(372.559519852168,-11.4828324101999,-2.72332119126683));
#35749=CARTESIAN_POINT('Ctrl Pts',(372.35055285699,-11.4687818229412,-2.84838974560999));
#35750=CARTESIAN_POINT('Ctrl Pts',(372.20566245711,-11.4598111685699,-2.92090960257575));
#35751=CARTESIAN_POINT('Ctrl Pts',(371.860945564956,-11.4389578149869,-3.06211560251359));
#35752=CARTESIAN_POINT('Ctrl Pts',(371.658624094335,-11.4270405695998,-3.1226622874181));
#35753=CARTESIAN_POINT('Ctrl Pts',(371.424947018585,-11.4127908146274,-3.16828445764703));
#35754=CARTESIAN_POINT('Ctrl Pts',(371.397973471801,-11.4111396169713,-3.17319420921733));
#35755=CARTESIAN_POINT('Ctrl Pts',(371.353667378644,-11.4084155461436,-3.18067611145235));
#35756=CARTESIAN_POINT('Ctrl Pts',(371.336370354483,-11.4073491303045,-3.18345217062455));
#35757=CARTESIAN_POINT('Ctrl Pts',(371.305232742327,-11.4054237546951,-3.18818947317329));
#35758=CARTESIAN_POINT('Ctrl Pts',(371.291400310104,-11.4045664388484,-3.19020196343595));
#35759=CARTESIAN_POINT('Ctrl Pts',(371.26186872399,-11.4027316697443,-3.19430252658275));
#35760=CARTESIAN_POINT('Ctrl Pts',(371.246166440934,-11.4017534315306,-3.19636498305872));
#35761=CARTESIAN_POINT('Ctrl Pts',(371.203598242637,-11.3990939492932,-3.20163733486297));
#35762=CARTESIAN_POINT('Ctrl Pts',(371.176706537124,-11.3974057606356,-3.20462471241331));
#35763=CARTESIAN_POINT('Ctrl Pts',(371.031574679082,-11.3882489311397,-3.21889969261471));
#35764=CARTESIAN_POINT('Ctrl Pts',(370.912829598672,-11.3805881815316,-3.22398134024731));
#35765=CARTESIAN_POINT('Ctrl Pts',(370.638620772259,-11.3625202194038,-3.22055794130342));
#35766=CARTESIAN_POINT('Ctrl Pts',(370.483510330732,-11.3520138328805,-3.20736933985001));
#35767=CARTESIAN_POINT('Ctrl Pts',(370.163412571277,-11.3300897111804,-3.15665037287258));
#35768=CARTESIAN_POINT('Ctrl Pts',(369.999167052317,-11.3187035207236,-3.11722462139496));
#35769=CARTESIAN_POINT('Ctrl Pts',(369.813131730597,-11.3061365401617,-3.05679930265338));
#35770=CARTESIAN_POINT('Ctrl Pts',(369.787618201556,-11.3044208368281,-3.04815731598887));
#35771=CARTESIAN_POINT('Ctrl Pts',(369.752479921424,-11.3020715751282,-3.03576198318334));
#35772=CARTESIAN_POINT('Ctrl Pts',(369.742761165726,-11.3014232612559,-3.03228101171567));
#35773=CARTESIAN_POINT('Ctrl Pts',(369.726100755185,-11.300314601618,-3.02622326451399));
#35774=CARTESIAN_POINT('Ctrl Pts',(369.719151016771,-11.299852948962,-3.02366918041048));
#35775=CARTESIAN_POINT('Ctrl Pts',(369.704622644207,-11.2988896679432,-3.01827298435493));
#35776=CARTESIAN_POINT('Ctrl Pts',(369.697045830819,-11.298388338211,-3.01542624220812));
#35777=CARTESIAN_POINT('Ctrl Pts',(369.679570214041,-11.2972342754912,-3.00878510915621));
#35778=CARTESIAN_POINT('Ctrl Pts',(369.669679147295,-11.2965827447286,-3.00497032185768));
#35779=CARTESIAN_POINT('Ctrl Pts',(369.634663329396,-11.2942815221975,-2.99126655706561));
#35780=CARTESIAN_POINT('Ctrl Pts',(369.609643450908,-11.2926469224985,-2.9811104154166));
#35781=CARTESIAN_POINT('Ctrl Pts',(369.548396883766,-11.2886625801397,-2.95534777651579));
#35782=CARTESIAN_POINT('Ctrl Pts',(369.512322698067,-11.2863306303508,-2.93938808335048));
#35783=CARTESIAN_POINT('Ctrl Pts',(369.366423591752,-11.2769246545106,-2.87161084084019));
#35784=CARTESIAN_POINT('Ctrl Pts',(369.25926915961,-11.2700736231069,-2.81426513984629));
#35785=CARTESIAN_POINT('Ctrl Pts',(368.967409907263,-11.2509103219685,-2.63616685057348));
#35786=CARTESIAN_POINT('Ctrl Pts',(368.791513593849,-11.2387123209317,-2.50233180527531));
#35787=CARTESIAN_POINT('Ctrl Pts',(368.580386531614,-11.2218178870088,-2.30448640455306));
#35788=CARTESIAN_POINT('Ctrl Pts',(368.531641807648,-11.2177385087443,-2.25578057619202));
#35789=CARTESIAN_POINT('Ctrl Pts',(368.468395623869,-11.2121740366731,-2.18839739198008));
#35790=CARTESIAN_POINT('Ctrl Pts',(368.452482296116,-11.2107496139405,-2.17106666746102));
#35791=CARTESIAN_POINT('Ctrl Pts',(368.426692322339,-11.2083998349384,-2.14235474921373));
#35792=CARTESIAN_POINT('Ctrl Pts',(368.416703036576,-11.207479244875,-2.13107558633624));
#35793=CARTESIAN_POINT('Ctrl Pts',(368.397464716824,-11.205685617414,-2.10904374256293));
#35794=CARTESIAN_POINT('Ctrl Pts',(368.388206839009,-11.2048129772168,-2.09829921897255));
#35795=CARTESIAN_POINT('Ctrl Pts',(368.366661843566,-11.202759490021,-2.07295812923782));
#35796=CARTESIAN_POINT('Ctrl Pts',(368.354432932613,-11.2015762998832,-2.05831298470395));
#35797=CARTESIAN_POINT('Ctrl Pts',(368.316242556199,-11.1978244522742,-2.01174241837882));
#35798=CARTESIAN_POINT('Ctrl Pts',(368.290762923699,-11.1952366614314,-1.97942891472614));
#35799=CARTESIAN_POINT('Ctrl Pts',(368.177530232997,-11.1833366662052,-1.83002886782835));
#35800=CARTESIAN_POINT('Ctrl Pts',(368.097205825692,-11.1737464961292,-1.70755205000281));
#35801=CARTESIAN_POINT('Ctrl Pts',(367.963736059794,-11.1555461206006,-1.47028586089492));
#35802=CARTESIAN_POINT('Ctrl Pts',(367.908475908128,-11.1470029753757,-1.35699200572998));
#35803=CARTESIAN_POINT('Ctrl Pts',(367.798590787857,-11.127718229268,-1.09357728486061));
#35804=CARTESIAN_POINT('Ctrl Pts',(367.748194884252,-11.1170197416778,-0.942022589411725));
#35805=CARTESIAN_POINT('Ctrl Pts',(367.704679507146,-11.1056746809298,-0.769303276358909));
#35806=CARTESIAN_POINT('Ctrl Pts',(367.700290341204,-11.1044973053141,-0.751222537038615));
#35807=CARTESIAN_POINT('Ctrl Pts',(367.693852416808,-11.1027193262758,-0.723663184199534));
#35808=CARTESIAN_POINT('Ctrl Pts',(367.691689530151,-11.1021125491315,-0.714212006525329));
#35809=CARTESIAN_POINT('Ctrl Pts',(367.687858906583,-11.1010206783313,-0.69711895270795));
#35810=CARTESIAN_POINT('Ctrl Pts',(367.686176319008,-11.1005347630543,-0.68948068941004));
#35811=CARTESIAN_POINT('Ctrl Pts',(367.68251060642,-11.0994619111551,-0.672546637401109));
#35812=CARTESIAN_POINT('Ctrl Pts',(367.680540790178,-11.0988757328808,-0.663248175635086));
#35813=CARTESIAN_POINT('Ctrl Pts',(367.67653338447,-11.0976624428529,-0.643909744087673));
#35814=CARTESIAN_POINT('Ctrl Pts',(367.674502469142,-11.0970357018055,-0.633868483641668));
#35815=CARTESIAN_POINT('Ctrl Pts',(367.669329469642,-11.0954072472061,-0.607649308772214));
#35816=CARTESIAN_POINT('Ctrl Pts',(367.666263493032,-11.0944095047552,-0.591456461788419));
#35817=CARTESIAN_POINT('Ctrl Pts',(367.629067436936,-11.081868259145,-0.386414294620745));
#35818=CARTESIAN_POINT('Ctrl Pts',(367.611744217969,-11.0711319694304,-0.194885383249188));
#35819=CARTESIAN_POINT('Ctrl Pts',(367.611569193008,-11.0603970329327,-0.00293863513896361));
#35820=CARTESIAN_POINT('Ctrl Pts',(367.611569193971,-11.0603970919897,-0.00293969111161769));
#35821=CARTESIAN_POINT('Ctrl Pts',(367.61139238361,-11.0495565454987,0.19089542073948));
#35822=CARTESIAN_POINT('Ctrl Pts',(367.628702684857,-11.0387500880331,0.384342450413428));
#35823=CARTESIAN_POINT('Ctrl Pts',(367.674481422554,-11.0237740215398,0.636777309751511));
#35824=CARTESIAN_POINT('Ctrl Pts',(367.687472116422,-11.0200658030643,0.698149526749735));
#35825=CARTESIAN_POINT('Ctrl Pts',(367.708609147836,-11.0146797500261,0.785361562531312));
#35826=CARTESIAN_POINT('Ctrl Pts',(367.71530365185,-11.0130478202635,0.811540534408275));
#35827=CARTESIAN_POINT('Ctrl Pts',(367.726440646869,-11.010443069287,0.852916995845585));
#35828=CARTESIAN_POINT('Ctrl Pts',(367.730667394687,-11.0094772301302,0.868171612544893));
#35829=CARTESIAN_POINT('Ctrl Pts',(367.738838150592,-11.0076515433216,0.896837995507693));
#35830=CARTESIAN_POINT('Ctrl Pts',(367.742757388951,-11.0067925194552,0.91025648340098));
#35831=CARTESIAN_POINT('Ctrl Pts',(367.75178797674,-11.0048497865332,0.940443742714512));
#35832=CARTESIAN_POINT('Ctrl Pts',(367.756949066781,-11.0037644731157,0.957197056729903));
#35833=CARTESIAN_POINT('Ctrl Pts',(367.770543532753,-11.00096776888,1.00007914114168));
#35834=CARTESIAN_POINT('Ctrl Pts',(367.779174461213,-10.9992499550086,1.02614334020761));
#35835=CARTESIAN_POINT('Ctrl Pts',(367.847834951257,-10.986006866201,1.22493961651566));
#35836=CARTESIAN_POINT('Ctrl Pts',(367.922125588808,-10.9740045664149,1.39236271946672));
#35837=CARTESIAN_POINT('Ctrl Pts',(368.073191078554,-10.9529566154958,1.66715199469731));
#35838=CARTESIAN_POINT('Ctrl Pts',(368.143102233134,-10.9440689366667,1.77780037995044));
#35839=CARTESIAN_POINT('Ctrl Pts',(368.29810935476,-10.9262037967182,1.99294499057722));
#35840=CARTESIAN_POINT('Ctrl Pts',(368.383433898668,-10.9172484529346,2.09698808581342));
#35841=CARTESIAN_POINT('Ctrl Pts',(368.488355152492,-10.9074264869318,2.20974206344318));
#35842=CARTESIAN_POINT('Ctrl Pts',(368.501824946052,-10.9061861812607,2.2239554541784));
#35843=CARTESIAN_POINT('Ctrl Pts',(368.522335268448,-10.9043296249808,2.24520670310338));
#35844=CARTESIAN_POINT('Ctrl Pts',(368.529279949688,-10.9037064416096,2.25233587225381));
#35845=CARTESIAN_POINT('Ctrl Pts',(368.541748857501,-10.9025974003231,2.26501794889453));
#35846=CARTESIAN_POINT('Ctrl Pts',(368.547260398606,-10.9021105920982,2.27058298952859));
#35847=CARTESIAN_POINT('Ctrl Pts',(368.559350582887,-10.9010501735651,2.2827018434581));
#35848=CARTESIAN_POINT('Ctrl Pts',(368.565937280082,-10.9004772095513,2.28924733649943));
#35849=CARTESIAN_POINT('Ctrl Pts',(368.584482823347,-10.8988769031982,2.30751823227752));
#35850=CARTESIAN_POINT('Ctrl Pts',(368.596505109759,-10.8978544357002,2.3191792096998));
#35851=CARTESIAN_POINT('Ctrl Pts',(368.666709483167,-10.8919657590337,2.3862194815426));
#35852=CARTESIAN_POINT('Ctrl Pts',(368.726859763971,-10.8872433303529,2.43950653240532));
#35853=CARTESIAN_POINT('Ctrl Pts',(368.995567621563,-10.8671800252795,2.66018888019764));
#35854=CARTESIAN_POINT('Ctrl Pts',(369.222511785332,-10.8527112689899,2.80351683829633));
#35855=CARTESIAN_POINT('Ctrl Pts',(369.565485473205,-10.8309983570869,2.96455935818278));
#35856=CARTESIAN_POINT('Ctrl Pts',(369.668786693791,-10.8244895539486,3.00667276212425));
#35857=CARTESIAN_POINT('Ctrl Pts',(369.799610433895,-10.8161748668473,3.05225006557322));
#35858=CARTESIAN_POINT('Ctrl Pts',(369.825276327981,-10.8145405105438,3.06083077594337));
#35859=CARTESIAN_POINT('Ctrl Pts',(369.866129765756,-10.8119327753655,3.07391936151035));
#35860=CARTESIAN_POINT('Ctrl Pts',(369.881248072983,-10.810966406475,3.07864034823302));
#35861=CARTESIAN_POINT('Ctrl Pts',(369.909773248725,-10.8091402713797,3.08731764152384));
#35862=CARTESIAN_POINT('Ctrl Pts',(369.923172294087,-10.8082813335659,3.09129854683643));
#35863=CARTESIAN_POINT('Ctrl Pts',(369.953419994172,-10.8063395395976,3.1000715085185));
#35864=CARTESIAN_POINT('Ctrl Pts',(369.97028256979,-10.8052550854951,3.10481358628746));
#35865=CARTESIAN_POINT('Ctrl Pts',(370.013629467184,-10.8024620750477,3.11662308945992));
#35866=CARTESIAN_POINT('Ctrl Pts',(370.040166396249,-10.8007471242499,3.12349040298824));
#35867=CARTESIAN_POINT('Ctrl Pts',(370.272554216889,-10.7856815322223,3.18047563367261));
#35868=CARTESIAN_POINT('Ctrl Pts',(370.482758211437,-10.7716777243932,3.2105108608682));
#35869=CARTESIAN_POINT('Ctrl Pts',(370.86446198308,-10.7459125953276,3.2271041092211));
#35870=CARTESIAN_POINT('Ctrl Pts',(371.034893406283,-10.7343042700751,3.22100636779373));
#35871=CARTESIAN_POINT('Ctrl Pts',(371.2525783519,-10.7198199754348,3.19586643870176));
#35872=CARTESIAN_POINT('Ctrl Pts',(371.300977282873,-10.7166230298801,3.18915876247364));
#35873=CARTESIAN_POINT('Ctrl Pts',(371.380728253609,-10.7114132060564,3.17625137989719));
#35874=CARTESIAN_POINT('Ctrl Pts',(371.412172987592,-10.7093741132156,3.17068143740342));
#35875=CARTESIAN_POINT('Ctrl Pts',(371.455199716385,-10.7066094260425,3.16239853231012));
#35876=CARTESIAN_POINT('Ctrl Pts',(371.466856047054,-10.7058630251494,3.16008769006207));
#35877=CARTESIAN_POINT('Ctrl Pts',(371.486457966996,-10.7046124879783,3.15608884648769));
#35878=CARTESIAN_POINT('Ctrl Pts',(371.494410366497,-10.7041064442171,3.15443519725787));
#35879=CARTESIAN_POINT('Ctrl Pts',(371.509570937284,-10.7031442918299,3.15122281323952));
#35880=CARTESIAN_POINT('Ctrl Pts',(371.516780110177,-10.702687875336,3.14966938211372));
#35881=CARTESIAN_POINT('Ctrl Pts',(371.533957201878,-10.701602889661,3.14590632144601));
#35882=CARTESIAN_POINT('Ctrl Pts',(371.543920148239,-10.7009755982443,3.14367402746045));
#35883=CARTESIAN_POINT('Ctrl Pts',(371.579390749205,-10.6987489264585,3.13554928041131));
#35884=CARTESIAN_POINT('Ctrl Pts',(371.604837782224,-10.6971637531869,3.12939323965));
#35885=CARTESIAN_POINT('Ctrl Pts',(371.82526351139,-10.6835172774205,3.07321689997358));
#35886=CARTESIAN_POINT('Ctrl Pts',(372.015259989424,-10.6723133849633,3.00533403589829));
#35887=CARTESIAN_POINT('Ctrl Pts',(372.235435482354,-10.6587270039936,2.90253706113548));
#35888=CARTESIAN_POINT('Ctrl Pts',(372.272816132784,-10.6563989826335,2.88419360677096));
#35889=CARTESIAN_POINT('Ctrl Pts',(372.309820694103,-10.6540649855006,2.86513680808753));
#35890=CARTESIAN_POINT('Ctrl Pts',(372.30982057914,-10.4044982614434,2.86513686729151));
#35891=CARTESIAN_POINT('Ctrl Pts',(372.28102533937,-10.406413188689,2.87996598601847));
#35892=CARTESIAN_POINT('Ctrl Pts',(372.252004110942,-10.4083420726229,2.89436226250651));
#35893=CARTESIAN_POINT('Ctrl Pts',(372.198048404882,-10.4119295058265,2.92012102184648));
#35894=CARTESIAN_POINT('Ctrl Pts',(372.173181478393,-10.4135833605025,2.93160569018576));
#35895=CARTESIAN_POINT('Ctrl Pts',(372.133637366772,-10.4162155226362,2.94926087715187));
#35896=CARTESIAN_POINT('Ctrl Pts',(372.119055315084,-10.417186597351,2.955642156904));
#35897=CARTESIAN_POINT('Ctrl Pts',(372.091578405281,-10.4190175116088,2.96742462465725));
#35898=CARTESIAN_POINT('Ctrl Pts',(372.078694469542,-10.4198764870069,2.97285045466003));
#35899=CARTESIAN_POINT('Ctrl Pts',(372.049668400213,-10.4218128815473,2.98485249518078));
#35900=CARTESIAN_POINT('Ctrl Pts',(372.033507494459,-10.4228918539382,2.9913818805526));
#35901=CARTESIAN_POINT('Ctrl Pts',(371.992084008194,-10.4256599629665,3.00772831957247));
#35902=CARTESIAN_POINT('Ctrl Pts',(371.966749496577,-10.4273552960831,3.01735821787974));
#35903=CARTESIAN_POINT('Ctrl Pts',(371.789892933096,-10.4392091415508,3.08204208973065));
#35904=CARTESIAN_POINT('Ctrl Pts',(371.634569949385,-10.4497332820341,3.12597027064345));
#35905=CARTESIAN_POINT('Ctrl Pts',(371.266400149232,-10.4748291166729,3.20085121771368));
#35906=CARTESIAN_POINT('Ctrl Pts',(371.052432698529,-10.4895434691031,3.22250926574736));
#35907=CARTESIAN_POINT('Ctrl Pts',(370.758583385094,-10.5090195668122,3.22283627695545));
#35908=CARTESIAN_POINT('Ctrl Pts',(370.679278897745,-10.5141972422438,3.21999604533427));
#35909=CARTESIAN_POINT('Ctrl Pts',(370.584044771735,-10.5202596899877,3.21305801654526));
#35910=CARTESIAN_POINT('Ctrl Pts',(370.567944634089,-10.5212792188829,3.21176334221661));
#35911=CARTESIAN_POINT('Ctrl Pts',(370.542830986558,-10.5228604110062,3.20955371097847));
#35912=CARTESIAN_POINT('Ctrl Pts',(370.533810704415,-10.5234265041432,3.20872171983508));
#35913=CARTESIAN_POINT('Ctrl Pts',(370.516962999273,-10.5244802437164,3.20709609357777));
#35914=CARTESIAN_POINT('Ctrl Pts',(370.509135030264,-10.5249683777756,3.2063118360434));
#35915=CARTESIAN_POINT('Ctrl Pts',(370.491240475586,-10.5260809722575,3.20445283318289));
#35916=CARTESIAN_POINT('Ctrl Pts',(370.481176022159,-10.5267043777651,3.20335931496087));
#35917=CARTESIAN_POINT('Ctrl Pts',(370.454362532064,-10.5283593651757,3.20031808273724));
#35918=CARTESIAN_POINT('Ctrl Pts',(370.437623097078,-10.5293864421138,3.19828628719821));
#35919=CARTESIAN_POINT('Ctrl Pts',(370.26173407472,-10.5401212579035,3.17553507806191));
#35920=CARTESIAN_POINT('Ctrl Pts',(370.104306100148,-10.5492422760347,3.14308315349049));
#35921=CARTESIAN_POINT('Ctrl Pts',(369.759038104664,-10.569406645226,3.0445525463515));
#35922=CARTESIAN_POINT('Ctrl Pts',(369.573592062951,-10.5803691433512,2.97255686567412));
#35923=CARTESIAN_POINT('Ctrl Pts',(369.306805288342,-10.5975400906141,2.83949758377183));
#35924=CARTESIAN_POINT('Ctrl Pts',(369.219777102473,-10.603380610344,2.79093111637788));
#35925=CARTESIAN_POINT('Ctrl Pts',(369.113285565928,-10.6109113536359,2.72485359507424));
#35926=CARTESIAN_POINT('Ctrl Pts',(369.091591814171,-10.6124662448358,2.71103027333172));
#35927=CARTESIAN_POINT('Ctrl Pts',(369.057050737254,-10.61497669521,2.68843468599537));
#35928=CARTESIAN_POINT('Ctrl Pts',(369.044097134028,-10.6159261376987,2.6798263424437));
#35929=CARTESIAN_POINT('Ctrl Pts',(369.019568811645,-10.6177394518686,2.66326878668728));
#35930=CARTESIAN_POINT('Ctrl Pts',(369.007982712556,-10.6186026511869,2.65533701403667));
#35931=CARTESIAN_POINT('Ctrl Pts',(368.981639039998,-10.6205808288341,2.63704831616705));
#35932=CARTESIAN_POINT('Ctrl Pts',(368.966915905387,-10.6216976434386,2.62664282894199));
#35933=CARTESIAN_POINT('Ctrl Pts',(368.921684068266,-10.6251640730828,2.59410297654295));
#35934=CARTESIAN_POINT('Ctrl Pts',(368.891476657028,-10.627529478509,2.57155714326813));
#35935=CARTESIAN_POINT('Ctrl Pts',(368.643987088356,-10.6473405501515,2.37998895583847));
#35936=CARTESIAN_POINT('Ctrl Pts',(368.448825304466,-10.6659167818329,2.18432209240417));
#35937=CARTESIAN_POINT('Ctrl Pts',(368.182734410084,-10.6953929415021,1.83878406913836));
#35938=CARTESIAN_POINT('Ctrl Pts',(368.094214589393,-10.7062024377311,1.7040736705516));
#35939=CARTESIAN_POINT('Ctrl Pts',(368.006338889797,-10.717758251913,1.54565827992494));
#35940=CARTESIAN_POINT('Ctrl Pts',(367.996718606948,-10.71903621659,1.52792509682853));
#35941=CARTESIAN_POINT('Ctrl Pts',(367.982628619844,-10.7209261590427,1.50136071305961));
#35942=CARTESIAN_POINT('Ctrl Pts',(367.978032252252,-10.7215456791031,1.49259775099669));
#35943=CARTESIAN_POINT('Ctrl Pts',(367.970215609066,-10.722604241189,1.47752700510939));
#35944=CARTESIAN_POINT('Ctrl Pts',(367.966975691584,-10.7230445018471,1.47122963783327));
#35945=CARTESIAN_POINT('Ctrl Pts',(367.959649466246,-10.7240434402104,1.45687366019148));
#35946=CARTESIAN_POINT('Ctrl Pts',(367.955576274191,-10.7246012959304,1.4488085182886));
#35947=CARTESIAN_POINT('Ctrl Pts',(367.94455071852,-10.7261184258169,1.42674724114561));
#35948=CARTESIAN_POINT('Ctrl Pts',(367.937666050786,-10.7270736035622,1.41271728981498));
#35949=CARTESIAN_POINT('Ctrl Pts',(367.903410899324,-10.7318691125973,1.34160695398074));
#35950=CARTESIAN_POINT('Ctrl Pts',(367.877622474084,-10.7356210420017,1.28377506192694));
#35951=CARTESIAN_POINT('Ctrl Pts',(367.830834886233,-10.7427918739453,1.16994802340883));
#35952=CARTESIAN_POINT('Ctrl Pts',(367.809657659782,-10.7462162281929,1.11405549531615));
#35953=CARTESIAN_POINT('Ctrl Pts',(367.734890425714,-10.7591479296147,0.898840962485617));
#35954=CARTESIAN_POINT('Ctrl Pts',(367.692237923036,-10.7684238651686,0.736004002226138));
#35955=CARTESIAN_POINT('Ctrl Pts',(367.642916121727,-10.7841294534494,0.461825549680339));
#35956=CARTESIAN_POINT('Ctrl Pts',(367.628959831884,-10.7904316810727,0.352143527385429));
#35957=CARTESIAN_POINT('Ctrl Pts',(367.617249825942,-10.7995486151241,0.196618990034791));
#35958=CARTESIAN_POINT('Ctrl Pts',(367.614795757088,-10.8022319064359,0.151204847244372));
#35959=CARTESIAN_POINT('Ctrl Pts',(367.612149228961,-10.8070414867095,0.0705990553209585));
#35960=CARTESIAN_POINT('Ctrl Pts',(367.611570633997,-10.8091559366688,0.035427173120199));
#35961=CARTESIAN_POINT('Ctrl Pts',(367.611566481463,-10.8123516288331,-0.0172867449321208));
#35962=CARTESIAN_POINT('Ctrl Pts',(367.611708303411,-10.8134193811027,-0.0348268039943945));
#35963=CARTESIAN_POINT('Ctrl Pts',(367.612220607262,-10.8153467853,-0.0663521158392946));
#35964=CARTESIAN_POINT('Ctrl Pts',(367.612538983666,-10.8162047865025,-0.0803378592582764));
#35965=CARTESIAN_POINT('Ctrl Pts',(367.613412090387,-10.8180406103638,-0.110157325405297));
#35966=CARTESIAN_POINT('Ctrl Pts',(367.61399254239,-10.8190192161161,-0.125989870620044));
#35967=CARTESIAN_POINT('Ctrl Pts',(367.615880063823,-10.8216786785127,-0.168841613204498));
#35968=CARTESIAN_POINT('Ctrl Pts',(367.61741059473,-10.8233664721422,-0.195849210292671));
#35969=CARTESIAN_POINT('Ctrl Pts',(367.627472276449,-10.8325035074752,-0.341018811442123));
#35970=CARTESIAN_POINT('Ctrl Pts',(367.642173112825,-10.8401438017132,-0.458648746005031));
#35971=CARTESIAN_POINT('Ctrl Pts',(367.690907019629,-10.8581322282262,-0.727316490725006));
#35972=CARTESIAN_POINT('Ctrl Pts',(367.729410405031,-10.8685775664986,-0.877247943545817));
#35973=CARTESIAN_POINT('Ctrl Pts',(367.832467983323,-10.8905231015617,-1.18484255702983));
#35974=CARTESIAN_POINT('Ctrl Pts',(367.89906327074,-10.9019924697251,-1.34135972040181));
#35975=CARTESIAN_POINT('Ctrl Pts',(367.990162180432,-10.9146356714281,-1.5157908435751));
#35976=CARTESIAN_POINT('Ctrl Pts',(368.002933371595,-10.9163517407998,-1.53951466373764));
#35977=CARTESIAN_POINT('Ctrl Pts',(368.021010630988,-10.9187017228962,-1.5721090036773));
#35978=CARTESIAN_POINT('Ctrl Pts',(368.026063699478,-10.9193503947947,-1.58111759869966));
#35979=CARTESIAN_POINT('Ctrl Pts',(368.03481570302,-10.9204597220778,-1.59654632501731));
#35980=CARTESIAN_POINT('Ctrl Pts',(368.038493591263,-10.9209216854215,-1.6029782143781));
#35981=CARTESIAN_POINT('Ctrl Pts',(368.046239040571,-10.9218856966206,-1.61641570084551));
#35982=CARTESIAN_POINT('Ctrl Pts',(368.050310878784,-10.9223874449018,-1.623418723424));
#35983=CARTESIAN_POINT('Ctrl Pts',(368.060354410511,-10.9236129591553,-1.64054335079539));
#35984=CARTESIAN_POINT('Ctrl Pts',(368.066355219001,-10.9243348658934,-1.65064791304022));
#35985=CARTESIAN_POINT('Ctrl Pts',(368.088385403696,-10.9269488073206,-1.68728583305302));
#35986=CARTESIAN_POINT('Ctrl Pts',(368.104742679193,-10.9288208034593,-1.71362132061252));
#35987=CARTESIAN_POINT('Ctrl Pts',(368.146805424064,-10.9334763800723,-1.77921212436636));
#35988=CARTESIAN_POINT('Ctrl Pts',(368.17299347815,-10.9362339810375,-1.81815066666817));
#35989=CARTESIAN_POINT('Ctrl Pts',(368.394713608224,-10.9585824686333,-2.13276115063203));
#35990=CARTESIAN_POINT('Ctrl Pts',(368.631646856875,-10.976578691745,-2.37668251492858));
#35991=CARTESIAN_POINT('Ctrl Pts',(368.952189429709,-11.0000449202257,-2.61679446924443));
#35992=CARTESIAN_POINT('Ctrl Pts',(369.003267431008,-11.0037533154348,-2.65278613555255));
#35993=CARTESIAN_POINT('Ctrl Pts',(369.074242249901,-11.0088828397131,-2.69977117527084));
#35994=CARTESIAN_POINT('Ctrl Pts',(369.093258645705,-11.0102549402371,-2.71207362068144));
#35995=CARTESIAN_POINT('Ctrl Pts',(369.123727524093,-11.012450551874,-2.73133260126661));
#35996=CARTESIAN_POINT('Ctrl Pts',(369.135096669497,-11.0132692027341,-2.73842005782962));
#35997=CARTESIAN_POINT('Ctrl Pts',(369.158539135722,-11.0149561152051,-2.75283175216709));
#35998=CARTESIAN_POINT('Ctrl Pts',(369.170617048954,-11.0158246484833,-2.76014792892698));
#35999=CARTESIAN_POINT('Ctrl Pts',(369.198736451597,-11.0178455761679,-2.7769295918656));
#36000=CARTESIAN_POINT('Ctrl Pts',(369.214812571435,-11.019000091194,-2.78633578350582));
#36001=CARTESIAN_POINT('Ctrl Pts',(369.266454175674,-11.0227065213142,-2.81595355662285));
#36002=CARTESIAN_POINT('Ctrl Pts',(369.302322178669,-11.0252775429032,-2.83562690607293));
#36003=CARTESIAN_POINT('Ctrl Pts',(369.387457581168,-11.0313749040399,-2.88023629930319));
#36004=CARTESIAN_POINT('Ctrl Pts',(369.437009425748,-11.0349199436871,-2.90459883016439));
#36005=CARTESIAN_POINT('Ctrl Pts',(369.623992074772,-11.0482831158258,-2.99063810855335));
#36006=CARTESIAN_POINT('Ctrl Pts',(369.765055682297,-11.0583485828385,-3.04392421484232));
#36007=CARTESIAN_POINT('Ctrl Pts',(370.116882147649,-11.0831472667146,-3.14934221342488));
#36008=CARTESIAN_POINT('Ctrl Pts',(370.330207794822,-11.097947759704,-3.1904477860507));
#36009=CARTESIAN_POINT('Ctrl Pts',(370.571324604508,-11.1134791106813,-3.2121014515382));
#36010=CARTESIAN_POINT('Ctrl Pts',(370.596619444875,-11.1150933923199,-3.2140722990005));
#36011=CARTESIAN_POINT('Ctrl Pts',(370.631991974651,-11.1173273567192,-3.21640845802767));
#36012=CARTESIAN_POINT('Ctrl Pts',(370.642051355567,-11.1179600126692,-3.21702544755913));
#36013=CARTESIAN_POINT('Ctrl Pts',(370.659446323678,-11.1190492512129,-3.2180104803428));
#36014=CARTESIAN_POINT('Ctrl Pts',(370.66678051127,-11.119507039215,-3.21840065017561));
#36015=CARTESIAN_POINT('Ctrl Pts',(370.6822731821,-11.1204708826753,-3.21917173882222));
#36016=CARTESIAN_POINT('Ctrl Pts',(370.690431896567,-11.1209765901982,-3.21954672275972));
#36017=CARTESIAN_POINT('Ctrl Pts',(370.710663386302,-11.1222261711082,-3.22039952675435));
#36018=CARTESIAN_POINT('Ctrl Pts',(370.722737733258,-11.1229680133612,-3.22084048451602));
#36019=CARTESIAN_POINT('Ctrl Pts',(370.768093832273,-11.1257409055048,-3.22224153541367));
#36020=CARTESIAN_POINT('Ctrl Pts',(370.801388592911,-11.1277485908794,-3.22275379062642));
#36021=CARTESIAN_POINT('Ctrl Pts',(371.053288027091,-11.1427678276117,-3.22272495494509));
#36022=CARTESIAN_POINT('Ctrl Pts',(371.271347816626,-11.1548266277656,-3.20045827703818));
#36023=CARTESIAN_POINT('Ctrl Pts',(371.691754190141,-11.1788566222239,-3.11372354671763));
#36024=CARTESIAN_POINT('Ctrl Pts',(371.893317763489,-11.1907681165754,-3.05106124510824));
#36025=CARTESIAN_POINT('Ctrl Pts',(372.11258790595,-11.2050120749109,-2.95852929458606));
#36026=CARTESIAN_POINT('Ctrl Pts',(372.13772112052,-11.2066640256381,-2.9475430052081));
#36027=CARTESIAN_POINT('Ctrl Pts',(372.178681100618,-11.2093894991024,-2.92901216929298));
#36028=CARTESIAN_POINT('Ctrl Pts',(372.19459226322,-11.2104565597733,-2.92165677988419));
#36029=CARTESIAN_POINT('Ctrl Pts',(372.223091359081,-11.2123832121548,-2.90819899352922));
#36030=CARTESIAN_POINT('Ctrl Pts',(372.235701145268,-11.2132411586356,-2.90214370691042));
#36031=CARTESIAN_POINT('Ctrl Pts',(372.262514703988,-11.215077405873,-2.88905219164578));
#36032=CARTESIAN_POINT('Ctrl Pts',(372.276706744185,-11.2160564936493,-2.88199290135788));
#36033=CARTESIAN_POINT('Ctrl Pts',(372.315007313719,-11.2187186302899,-2.86258797360678));
#36034=CARTESIAN_POINT('Ctrl Pts',(372.339012797886,-11.2204086399349,-2.85004284820731));
#36035=CARTESIAN_POINT('Ctrl Pts',(372.467646289397,-11.2295833657861,-2.78074159869951));
#36036=CARTESIAN_POINT('Ctrl Pts',(372.569215616735,-11.2372610351857,-2.71853078414517));
#36037=CARTESIAN_POINT('Ctrl Pts',(372.795519823749,-11.2553899161026,-2.56206526432011));
#36038=CARTESIAN_POINT('Ctrl Pts',(372.917306582943,-11.2659416592702,-2.46407035035053));
#36039=CARTESIAN_POINT('Ctrl Pts',(373.154163118018,-11.2878434324473,-2.2433341237176));
#36040=CARTESIAN_POINT('Ctrl Pts',(373.267726844679,-11.2991614802583,-2.11961349159814));
#36041=CARTESIAN_POINT('Ctrl Pts',(373.387772417076,-11.3116670670705,-1.96639604197878));
#36042=CARTESIAN_POINT('Ctrl Pts',(373.404124610886,-11.3133834141312,-1.94497736285598));
#36043=CARTESIAN_POINT('Ctrl Pts',(373.426371468753,-11.3157337062222,-1.91506718222495));
#36044=CARTESIAN_POINT('Ctrl Pts',(373.432496306388,-11.3163824155087,-1.9067493255678));
#36045=CARTESIAN_POINT('Ctrl Pts',(373.442945645317,-11.3174917898624,-1.89241472767484));
#36046=CARTESIAN_POINT('Ctrl Pts',(373.447289539021,-11.3179537631312,-1.88641231734846));
#36047=CARTESIAN_POINT('Ctrl Pts',(373.456339208495,-11.3189177757352,-1.87381621129467));
#36048=CARTESIAN_POINT('Ctrl Pts',(373.461040877175,-11.319419515606,-1.86721968135541));
#36049=CARTESIAN_POINT('Ctrl Pts',(373.472501969401,-11.3206449775615,-1.85101059412344));
#36050=CARTESIAN_POINT('Ctrl Pts',(373.479233869248,-11.3213668407829,-1.84137854025664));
#36051=CARTESIAN_POINT('Ctrl Pts',(373.503529137048,-11.3239804439054,-1.80620854839717));
#36052=CARTESIAN_POINT('Ctrl Pts',(373.520777168093,-11.3258521520454,-1.78045351212091));
#36053=CARTESIAN_POINT('Ctrl Pts',(373.563188088894,-11.3305068627522,-1.71510499426295));
#36054=CARTESIAN_POINT('Ctrl Pts',(373.587863686439,-11.3332638981738,-1.67520258007805));
#36055=CARTESIAN_POINT('Ctrl Pts',(373.782962925474,-11.3555965803475,-1.34374543995809));
#36056=CARTESIAN_POINT('Ctrl Pts',(373.907466825137,-11.3735795501286,-1.02759680397341));
#36057=CARTESIAN_POINT('Ctrl Pts',(373.994180076412,-11.3970400834009,-0.636646258040273));
#36058=CARTESIAN_POINT('Ctrl Pts',(374.005965632103,-11.4007609858015,-0.575062882965707));
#36059=CARTESIAN_POINT('Ctrl Pts',(374.019558633886,-11.405905190604,-0.490788212587248));
#36060=CARTESIAN_POINT('Ctrl Pts',(374.022933437463,-11.4072790926738,-0.468361522806853));
#36061=CARTESIAN_POINT('Ctrl Pts',(374.027925671493,-11.4094768659157,-0.432627220025935));
#36062=CARTESIAN_POINT('Ctrl Pts',(374.029697295778,-11.4102958592154,-0.419341648307175));
#36063=CARTESIAN_POINT('Ctrl Pts',(374.03316479133,-11.4119829400325,-0.392039738432337));
#36064=CARTESIAN_POINT('Ctrl Pts',(374.034851532109,-11.412851295845,-0.378022552482008));
#36065=CARTESIAN_POINT('Ctrl Pts',(374.038547708966,-11.4148708950449,-0.345506624511931));
#36066=CARTESIAN_POINT('Ctrl Pts',(374.040489128683,-11.4160242502487,-0.327000802996365));
#36067=CARTESIAN_POINT('Ctrl Pts',(374.046176038974,-11.4197231400437,-0.267861261491525));
#36068=CARTESIAN_POINT('Ctrl Pts',(374.049309976814,-11.4222876719901,-0.227174075804159));
#36069=CARTESIAN_POINT('Ctrl Pts',(374.054854204941,-11.4283669500942,-0.131498492328237));
#36070=CARTESIAN_POINT('Ctrl Pts',(374.056629964147,-11.4319002466529,-0.0764874524782389));
#36071=CARTESIAN_POINT('Ctrl Pts',(374.057993990782,-11.4451974516397,0.128346304726189));
#36072=CARTESIAN_POINT('Ctrl Pts',(374.048544694044,-11.4552060229506,0.278025119399729));
#36073=CARTESIAN_POINT('Ctrl Pts',(373.99988267551,-11.480030968619,0.642503451707805));
#36074=CARTESIAN_POINT('Ctrl Pts',(373.949204069565,-11.4949206420902,0.855049036034128));
#36075=CARTESIAN_POINT('Ctrl Pts',(373.869127262658,-11.5105263255276,1.08475319314395));
#36076=CARTESIAN_POINT('Ctrl Pts',(373.86051776058,-11.5121360803272,1.10854492660686));
#36077=CARTESIAN_POINT('Ctrl Pts',(373.848092134179,-11.5143648403111,1.1416582131315));
#36078=CARTESIAN_POINT('Ctrl Pts',(373.844511408485,-11.5149967420305,1.15106631362049));
#36079=CARTESIAN_POINT('Ctrl Pts',(373.838243064212,-11.5160850385809,1.16730663774686));
#36080=CARTESIAN_POINT('Ctrl Pts',(373.835576096994,-11.5165426340296,1.17414667588696));
#36081=CARTESIAN_POINT('Ctrl Pts',(373.829891605292,-11.517506492469,1.18857991662423));
#36082=CARTESIAN_POINT('Ctrl Pts',(373.826868534533,-11.5180124051761,1.19617086765528));
#36083=CARTESIAN_POINT('Ctrl Pts',(373.819297508777,-11.5192632072153,1.21497341476285));
#36084=CARTESIAN_POINT('Ctrl Pts',(373.814715172117,-11.5200060566222,1.22617118502375));
#36085=CARTESIAN_POINT('Ctrl Pts',(373.797240506955,-11.5227871959108,1.26819693300365));
#36086=CARTESIAN_POINT('Ctrl Pts',(373.783931555685,-11.524801941274,1.29885076850193));
#36087=CARTESIAN_POINT('Ctrl Pts',(373.679165325883,-11.539944573511,1.53023371099417));
#36088=CARTESIAN_POINT('Ctrl Pts',(373.567781924503,-11.5521033828109,1.7213283579283));
#36089=CARTESIAN_POINT('Ctrl Pts',(373.314860167131,-11.5761289845239,2.06796652793123));
#36090=CARTESIAN_POINT('Ctrl Pts',(373.17595323639,-11.5879277187175,2.22402874121356));
#36091=CARTESIAN_POINT('Ctrl Pts',(373.002826645283,-11.6020438502495,2.38420628766738));
#36092=CARTESIAN_POINT('Ctrl Pts',(372.98245533906,-11.6036958966408,2.40257679907413));
#36093=CARTESIAN_POINT('Ctrl Pts',(372.948685645018,-11.606421495981,2.43225691221069));
#36094=CARTESIAN_POINT('Ctrl Pts',(372.935424824993,-11.6074885858325,2.44372140807376));
#36095=CARTESIAN_POINT('Ctrl Pts',(372.911415035386,-11.609415269923,2.46413890306841));
#36096=CARTESIAN_POINT('Ctrl Pts',(372.900699983294,-11.6102732187006,2.4731312380325));
#36097=CARTESIAN_POINT('Ctrl Pts',(372.877719350153,-11.6121094480167,2.4921635425335));
#36098=CARTESIAN_POINT('Ctrl Pts',(372.865437597991,-11.6130885154087,2.50218332031478));
#36099=CARTESIAN_POINT('Ctrl Pts',(372.831970815276,-11.6157505389467,2.52907764773245));
#36100=CARTESIAN_POINT('Ctrl Pts',(372.81064653442,-11.6174404548668,2.54577610504094));
#36101=CARTESIAN_POINT('Ctrl Pts',(372.694500863901,-11.6266135816091,2.63438780729107));
#36102=CARTESIAN_POINT('Ctrl Pts',(372.595972237138,-11.6342896647715,2.70126785832075));
#36103=CARTESIAN_POINT('Ctrl Pts',(372.433707983684,-11.6467627568836,2.79875201198031));
#36104=CARTESIAN_POINT('Ctrl Pts',(372.372287377688,-11.6514471413943,2.83296740183991));
#36105=CARTESIAN_POINT('Ctrl Pts',(372.309820451737,-11.6561638218248,2.86513693290211));
#36106=CARTESIAN_POINT('Origin',(370.834317853224,2.31077344927308,0.));
#36107=CARTESIAN_POINT('',(372.309820665215,-13.1553703139997,2.86513682296437));
#36108=CARTESIAN_POINT('',(372.309820613641,-12.9102404761535,2.86513684952405));
#36109=CARTESIAN_POINT('',(372.309820613641,2.31077344927308,2.86513684952399));
#36110=CARTESIAN_POINT('Ctrl Pts',(372.309820665215,-13.1553703139997,2.86513682296442));
#36111=CARTESIAN_POINT('Ctrl Pts',(372.49600560238,-13.1414843015589,2.76925435196471));
#36112=CARTESIAN_POINT('Ctrl Pts',(372.672435253176,-13.1271546951046,2.65543345258058));
#36113=CARTESIAN_POINT('Ctrl Pts',(372.894767161932,-13.1081534012158,2.47914895204465));
#36114=CARTESIAN_POINT('Ctrl Pts',(372.951341412221,-13.1032293604608,2.43101697135416));
#36115=CARTESIAN_POINT('Ctrl Pts',(373.027551591667,-13.0965228666838,2.36149912705992));
#36116=CARTESIAN_POINT('Ctrl Pts',(373.048635621919,-13.0946592891503,2.34174065592088));
#36117=CARTESIAN_POINT('Ctrl Pts',(373.084909869162,-13.0914429942513,2.30681892568052));
#36118=CARTESIAN_POINT('Ctrl Pts',(373.100219392852,-13.0900823296938,2.29178276637832));
#36119=CARTESIAN_POINT('Ctrl Pts',(373.122541249142,-13.0880951848621,2.2694171226996));
#36120=CARTESIAN_POINT('Ctrl Pts',(373.129670634175,-13.0874600133889,2.26220600387378));
#36121=CARTESIAN_POINT('Ctrl Pts',(373.142256411684,-13.0863380366953,2.24935518440584));
#36122=CARTESIAN_POINT('Ctrl Pts',(373.147726371234,-13.0858501880285,2.24372907646196));
#36123=CARTESIAN_POINT('Ctrl Pts',(373.15952889113,-13.0847971095648,2.23150058891496));
#36124=CARTESIAN_POINT('Ctrl Pts',(373.165853908903,-13.0842324536888,2.22489120521256));
#36125=CARTESIAN_POINT('Ctrl Pts',(373.183259646226,-13.0826774275886,2.20654718790194));
#36126=CARTESIAN_POINT('Ctrl Pts',(373.194280664324,-13.081691503186,2.19475593047308));
#36127=CARTESIAN_POINT('Ctrl Pts',(373.252951194433,-13.0764325984922,2.13103207236588));
#36128=CARTESIAN_POINT('Ctrl Pts',(373.298979645796,-13.0722697667568,2.07762575252782));
#36129=CARTESIAN_POINT('Ctrl Pts',(373.365787890776,-13.0660944131815,1.99476051905157));
#36130=CARTESIAN_POINT('Ctrl Pts',(373.387883495148,-13.0640281801022,1.96639587342609));
#36131=CARTESIAN_POINT('Ctrl Pts',(373.452816296596,-13.057863806368,1.88009939258955));
#36132=CARTESIAN_POINT('Ctrl Pts',(373.494190992327,-13.0538095070511,1.8210939934438));
#36133=CARTESIAN_POINT('Ctrl Pts',(373.636179186345,-13.0392449640128,1.60342553247583));
#36134=CARTESIAN_POINT('Ctrl Pts',(373.724848251512,-13.028837132229,1.43743888227736));
#36135=CARTESIAN_POINT('Ctrl Pts',(373.823667322106,-13.0143155777988,1.20582013899002));
#36136=CARTESIAN_POINT('Ctrl Pts',(373.847019103417,-13.0105823528121,1.1462298657046));
#36137=CARTESIAN_POINT('Ctrl Pts',(373.884011757468,-13.0040825702657,1.04287182608386));
#36138=CARTESIAN_POINT('Ctrl Pts',(373.898521522852,-13.0013438329883,0.999434895927137));
#36139=CARTESIAN_POINT('Ctrl Pts',(373.917873567437,-12.9973975829333,0.937112969718748));
#36140=CARTESIAN_POINT('Ctrl Pts',(373.923478072031,-12.9962149525484,0.918469203347576));
#36141=CARTESIAN_POINT('Ctrl Pts',(373.93289122067,-12.9941572153639,0.886094609553033));
#36142=CARTESIAN_POINT('Ctrl Pts',(373.936778391633,-12.9932846898834,0.872387051638313));
#36143=CARTESIAN_POINT('Ctrl Pts',(373.94455310719,-12.9914916149991,0.844261342964246));
#36144=CARTESIAN_POINT('Ctrl Pts',(373.948431586621,-12.9905707958538,0.829841065349289));
#36145=CARTESIAN_POINT('Ctrl Pts',(373.958005227728,-12.9882291675783,0.793233539173976));
#36146=CARTESIAN_POINT('Ctrl Pts',(373.963564239652,-12.9868040065122,0.771011848701875));
#36147=CARTESIAN_POINT('Ctrl Pts',(373.983846500876,-12.9813430771181,0.686100264265635));
#36148=CARTESIAN_POINT('Ctrl Pts',(373.996925697725,-12.9772553735,0.623036873719591));
#36149=CARTESIAN_POINT('Ctrl Pts',(374.066407095776,-12.9515024318494,0.22899033315953));
#36150=CARTESIAN_POINT('Ctrl Pts',(374.072674931922,-12.9282184664451,-0.108634208726018));
#36151=CARTESIAN_POINT('Ctrl Pts',(374.020330143661,-12.9029742150544,-0.487479006504268));
#36152=CARTESIAN_POINT('Ctrl Pts',(374.012910844455,-12.8999138603393,-0.53372009315687));
#36153=CARTESIAN_POINT('Ctrl Pts',(373.998918243087,-12.8949021965163,-0.610229278273118));
#36154=CARTESIAN_POINT('Ctrl Pts',(373.992911910017,-12.8929269841979,-0.640592810210678));
#36155=CARTESIAN_POINT('Ctrl Pts',(373.984025152851,-12.8902340107996,-0.682348369296394));
#36156=CARTESIAN_POINT('Ctrl Pts',(373.981518698094,-12.8894967866087,-0.693817139071653));
#36157=CARTESIAN_POINT('Ctrl Pts',(373.977178331509,-12.8882572051641,-0.713169745346141));
#36158=CARTESIAN_POINT('Ctrl Pts',(373.975377299232,-12.8877530130654,-0.721060769536663));
#36159=CARTESIAN_POINT('Ctrl Pts',(373.971871807403,-12.8867909251843,-0.736157298244396));
#36160=CARTESIAN_POINT('Ctrl Pts',(373.970172225456,-12.8863327444806,-0.74336380185075));
#36161=CARTESIAN_POINT('Ctrl Pts',(373.966043589247,-12.8852391061759,-0.760603736481957));
#36162=CARTESIAN_POINT('Ctrl Pts',(373.963591115057,-12.8846049736435,-0.770631552123071));
#36163=CARTESIAN_POINT('Ctrl Pts',(373.954565874849,-12.8823256257672,-0.806780865854768));
#36164=CARTESIAN_POINT('Ctrl Pts',(373.947713673173,-12.8806955225009,-0.832832310758043));
#36165=CARTESIAN_POINT('Ctrl Pts',(373.895621635161,-12.8689769024962,-1.02124638395038));
#36166=CARTESIAN_POINT('Ctrl Pts',(373.838027299363,-12.8594823205243,-1.17994426072656));
#36167=CARTESIAN_POINT('Ctrl Pts',(373.703923084344,-12.8413328960078,-1.4750162691959));
#36168=CARTESIAN_POINT('Ctrl Pts',(373.629407457263,-12.8326913540337,-1.61176274286099));
#36169=CARTESIAN_POINT('Ctrl Pts',(373.481078512035,-12.817009528736,-1.84252224867932));
#36170=CARTESIAN_POINT('Ctrl Pts',(373.411373283167,-12.810087863881,-1.93881691050339));
#36171=CARTESIAN_POINT('Ctrl Pts',(373.319464814596,-12.8013350095954,-2.05204636485041));
#36172=CARTESIAN_POINT('Ctrl Pts',(373.302148799156,-12.7997008761898,-2.07283864728086));
#36173=CARTESIAN_POINT('Ctrl Pts',(373.274285831344,-12.7970934151326,-2.10545117578254));
#36174=CARTESIAN_POINT('Ctrl Pts',(373.263909773589,-12.7961270948983,-2.11741622605177));
#36175=CARTESIAN_POINT('Ctrl Pts',(373.24421064373,-12.7943010010314,-2.13979664612373));
#36176=CARTESIAN_POINT('Ctrl Pts',(373.234907151148,-12.793442055366,-2.15022881606107));
#36177=CARTESIAN_POINT('Ctrl Pts',(373.213791822752,-12.7915001754068,-2.17359795454437));
#36178=CARTESIAN_POINT('Ctrl Pts',(373.201941850476,-12.7904156425777,-2.18649972053431));
#36179=CARTESIAN_POINT('Ctrl Pts',(373.171278751713,-12.7876222937791,-2.21934289676662));
#36180=CARTESIAN_POINT('Ctrl Pts',(373.152315586551,-12.7859070807398,-2.2391417034649));
#36181=CARTESIAN_POINT('Ctrl Pts',(372.985240095778,-12.7708972330847,-2.40918257738566));
#36182=CARTESIAN_POINT('Ctrl Pts',(372.822984839879,-12.7569553114394,-2.54475965031107));
#36183=CARTESIAN_POINT('Ctrl Pts',(372.513919452844,-12.7317395819529,-2.7552936770313));
#36184=CARTESIAN_POINT('Ctrl Pts',(372.372384972132,-12.7206281929807,-2.83673342572432));
#36185=CARTESIAN_POINT('Ctrl Pts',(372.152806263446,-12.704487753263,-2.94179588980917));
#36186=CARTESIAN_POINT('Ctrl Pts',(372.07904120381,-12.6992404018993,-2.97375870496275));
#36187=CARTESIAN_POINT('Ctrl Pts',(371.989057330074,-12.6931087321774,-3.0088131774361));
#36188=CARTESIAN_POINT('Ctrl Pts',(371.973917989345,-12.69208610397,-3.01457982998576));
#36189=CARTESIAN_POINT('Ctrl Pts',(371.950240299646,-12.6905014323673,-3.02339491734955));
#36190=CARTESIAN_POINT('Ctrl Pts',(371.941731724599,-12.6899349241486,-3.02652180810113));
#36191=CARTESIAN_POINT('Ctrl Pts',(371.925821833805,-12.6888812685009,-3.03229259610586));
#36192=CARTESIAN_POINT('Ctrl Pts',(371.918424091957,-12.6883936269904,-3.03494530308634));
#36193=CARTESIAN_POINT('Ctrl Pts',(371.901501468835,-12.6872832571903,-3.04094370278729));
#36194=CARTESIAN_POINT('Ctrl Pts',(371.891970516232,-12.6866615723428,-3.04427172305381));
#36195=CARTESIAN_POINT('Ctrl Pts',(371.866558674392,-12.6850134059558,-3.05301128848853));
#36196=CARTESIAN_POINT('Ctrl Pts',(371.850650664581,-12.6839913747568,-3.05834378125594));
#36197=CARTESIAN_POINT('Ctrl Pts',(371.712967360517,-12.6752236784987,-3.10330339317272));
#36198=CARTESIAN_POINT('Ctrl Pts',(371.588957205672,-12.6678493895597,-3.13576849423365));
#36199=CARTESIAN_POINT('Ctrl Pts',(371.278963947459,-12.6499635312317,-3.19745909801766));
#36200=CARTESIAN_POINT('Ctrl Pts',(371.091741179984,-12.6396157762381,-3.21794809066764));
#36201=CARTESIAN_POINT('Ctrl Pts',(370.765592500594,-12.621087838473,-3.2249812385774));
#36202=CARTESIAN_POINT('Ctrl Pts',(370.627353731725,-12.6130833855475,-3.21906607256498));
#36203=CARTESIAN_POINT('Ctrl Pts',(370.461961725342,-12.6031087283913,-3.20129033845343));
#36204=CARTESIAN_POINT('Ctrl Pts',(370.434033038417,-12.6014109518887,-3.19791821473489));
#36205=CARTESIAN_POINT('Ctrl Pts',(370.390224773501,-12.5987252452508,-3.19204592029569));
#36206=CARTESIAN_POINT('Ctrl Pts',(370.374313243102,-12.5977450718917,-3.18979177451796));
#36207=CARTESIAN_POINT('Ctrl Pts',(370.344619874513,-12.5959068454444,-3.18535839831712));
#36208=CARTESIAN_POINT('Ctrl Pts',(370.330833990999,-12.5950497389054,-3.18320847995466));
#36209=CARTESIAN_POINT('Ctrl Pts',(370.300098115071,-12.5931304293834,-3.17821054052797));
#36210=CARTESIAN_POINT('Ctrl Pts',(370.283156166674,-12.5920667838938,-3.17531632211955));
#36211=CARTESIAN_POINT('Ctrl Pts',(370.240322393274,-12.5893628130667,-3.16764583495307));
#36212=CARTESIAN_POINT('Ctrl Pts',(370.214464834338,-12.5877167652188,-3.16268760882752));
#36213=CARTESIAN_POINT('Ctrl Pts',(370.051546648608,-12.5772564992531,-3.12937314545875));
#36214=CARTESIAN_POINT('Ctrl Pts',(369.916412330756,-12.5681702555884,-3.09243389223329));
#36215=CARTESIAN_POINT('Ctrl Pts',(369.583963781493,-12.5448222477043,-2.97784397960769));
#36216=CARTESIAN_POINT('Ctrl Pts',(369.391107927493,-12.5303276186846,-2.88930380136953));
#36217=CARTESIAN_POINT('Ctrl Pts',(369.14824784654,-12.5115261759108,-2.7473857954625));
#36218=CARTESIAN_POINT('Ctrl Pts',(369.089310847549,-12.5069209284005,-2.71033439234708));
#36219=CARTESIAN_POINT('Ctrl Pts',(369.008679829616,-12.5006049074782,-2.65592338612546));
#36220=CARTESIAN_POINT('Ctrl Pts',(368.985942566465,-12.4988220880429,-2.64015002104584));
#36221=CARTESIAN_POINT('Ctrl Pts',(368.946515867076,-12.495731411226,-2.61203976714881));
#36222=CARTESIAN_POINT('Ctrl Pts',(368.929737438446,-12.4944163893038,-2.5998310675668));
#36223=CARTESIAN_POINT('Ctrl Pts',(368.905045965816,-12.4924829630885,-2.58149716618719));
#36224=CARTESIAN_POINT('Ctrl Pts',(368.89704202107,-12.4918565094882,-2.57549606697923));
#36225=CARTESIAN_POINT('Ctrl Pts',(368.882818598311,-12.4907439688227,-2.56472798190366));
#36226=CARTESIAN_POINT('Ctrl Pts',(368.876588441152,-12.4902569059786,-2.55997549136882));
#36227=CARTESIAN_POINT('Ctrl Pts',(368.863044269302,-12.4891986214843,-2.54956535851149));
#36228=CARTESIAN_POINT('Ctrl Pts',(368.855737248165,-12.4886280256751,-2.54389894733636));
#36229=CARTESIAN_POINT('Ctrl Pts',(368.835401336629,-12.4870406669556,-2.52798833272601));
#36230=CARTESIAN_POINT('Ctrl Pts',(368.822426721905,-12.4860286543729,-2.51767479098975));
#36231=CARTESIAN_POINT('Ctrl Pts',(368.749398197081,-12.4803330125717,-2.45869923673588));
#36232=CARTESIAN_POINT('Ctrl Pts',(368.691025727176,-12.4757823392948,-2.40798521776679));
#36233=CARTESIAN_POINT('Ctrl Pts',(368.617937024324,-12.4700023173779,-2.33971986210335));
#36234=CARTESIAN_POINT('Ctrl Pts',(368.601509019523,-12.4686975160501,-2.32404771006862));
#36235=CARTESIAN_POINT('Ctrl Pts',(368.387635965418,-12.4516145941784,-2.11565378029722));
#36236=CARTESIAN_POINT('Ctrl Pts',(368.215568602294,-12.4366757671791,-1.89852767511086));
#36237=CARTESIAN_POINT('Ctrl Pts',(368.027834970809,-12.4156045582098,-1.5866720369017));
#36238=CARTESIAN_POINT('Ctrl Pts',(367.985527311873,-12.4104208200727,-1.50939217932632));
#36239=CARTESIAN_POINT('Ctrl Pts',(367.935463443943,-12.4036372741364,-1.40832246913053));
#36240=CARTESIAN_POINT('Ctrl Pts',(367.924742839065,-12.4021414851364,-1.38603832856428));
#36241=CARTESIAN_POINT('Ctrl Pts',(367.907794249931,-12.3997041350919,-1.3497452021626));
#36242=CARTESIAN_POINT('Ctrl Pts',(367.901407792238,-12.398768064484,-1.3358110168862));
#36243=CARTESIAN_POINT('Ctrl Pts',(367.88934342893,-12.3969651508468,-1.30898496169207));
#36244=CARTESIAN_POINT('Ctrl Pts',(367.883650158951,-12.396098860356,-1.29610035786242));
#36245=CARTESIAN_POINT('Ctrl Pts',(367.870821192278,-12.3941106708024,-1.26654410012409));
#36246=CARTESIAN_POINT('Ctrl Pts',(367.863741427568,-12.3929868987645,-1.24984882877824));
#36247=CARTESIAN_POINT('Ctrl Pts',(367.841749054565,-12.3894096700996,-1.19674455220788));
#36248=CARTESIAN_POINT('Ctrl Pts',(367.827362544945,-12.3869386465185,-1.16012287795443));
#36249=CARTESIAN_POINT('Ctrl Pts',(367.722896263078,-12.367944326494,-0.87918954374385));
#36250=CARTESIAN_POINT('Ctrl Pts',(367.662070667211,-12.3504266921635,-0.625073285691753));
#36251=CARTESIAN_POINT('Ctrl Pts',(367.618497233372,-12.324509842423,-0.24437346261009));
#36252=CARTESIAN_POINT('Ctrl Pts',(367.61151703475,-12.3162197348941,-0.12156920414431));
#36253=CARTESIAN_POINT('Ctrl Pts',(367.611592421954,-12.3043134011387,0.0597676870176285));
#36254=CARTESIAN_POINT('Ctrl Pts',(367.613205645872,-12.3005296732742,0.118188417210321));
#36255=CARTESIAN_POINT('Ctrl Pts',(367.617249032242,-12.2958479450795,0.191891186069334));
#36256=CARTESIAN_POINT('Ctrl Pts',(367.618201283009,-12.2948780331451,0.20723960753836));
#36257=CARTESIAN_POINT('Ctrl Pts',(367.619877027616,-12.2933570223259,0.231444776764523));
#36258=CARTESIAN_POINT('Ctrl Pts',(367.620527338041,-12.2928020077697,0.240306127718133));
#36259=CARTESIAN_POINT('Ctrl Pts',(367.621824768854,-12.2917576693635,0.257037140878664));
#36260=CARTESIAN_POINT('Ctrl Pts',(367.622464156501,-12.2912679501679,0.26490704208438));
#36261=CARTESIAN_POINT('Ctrl Pts',(367.624027475232,-12.290126170531,0.28331089402103));
#36262=CARTESIAN_POINT('Ctrl Pts',(367.624974333418,-12.2894753935578,0.293842734986465));
#36263=CARTESIAN_POINT('Ctrl Pts',(367.62822097301,-12.2873687020081,0.32806536820198));
#36264=CARTESIAN_POINT('Ctrl Pts',(367.630731433243,-12.2859240044538,0.351736004271204));
#36265=CARTESIAN_POINT('Ctrl Pts',(367.645721739493,-12.2781794625601,0.479557165374106));
#36266=CARTESIAN_POINT('Ctrl Pts',(367.663019712849,-12.2721100077012,0.583088893248654));
#36267=CARTESIAN_POINT('Ctrl Pts',(367.7365527273,-12.2524553506403,0.92082721406705));
#36268=CARTESIAN_POINT('Ctrl Pts',(367.813959929309,-12.2393206129761,1.14957147026003));
#36269=CARTESIAN_POINT('Ctrl Pts',(367.959725240114,-12.2195757517179,1.46061424285653));
#36270=CARTESIAN_POINT('Ctrl Pts',(368.007751609373,-12.213562601036,1.55151437941975));
#36271=CARTESIAN_POINT('Ctrl Pts',(368.073780734393,-12.2057745076088,1.66321439620616));
#36272=CARTESIAN_POINT('Ctrl Pts',(368.087818793883,-12.2041429980597,1.68629480276344));
#36273=CARTESIAN_POINT('Ctrl Pts',(368.110539366544,-12.2015387638579,1.72261395507653));
#36274=CARTESIAN_POINT('Ctrl Pts',(368.119032324797,-12.2005730164447,1.73597020938261));
#36275=CARTESIAN_POINT('Ctrl Pts',(368.134452153272,-12.1988330377429,1.7598298365244));
#36276=CARTESIAN_POINT('Ctrl Pts',(368.141342838454,-12.1980601661762,1.77035629578006));
#36277=CARTESIAN_POINT('Ctrl Pts',(368.157617870291,-12.1962454310831,1.79490373371024));
#36278=CARTESIAN_POINT('Ctrl Pts',(368.167050966097,-12.1952017482351,1.80889180092038));
#36279=CARTESIAN_POINT('Ctrl Pts',(368.194641813012,-12.1921719933352,1.84912038979499));
#36280=CARTESIAN_POINT('Ctrl Pts',(368.213079607661,-12.1901753392797,1.87516552752499));
#36281=CARTESIAN_POINT('Ctrl Pts',(368.359693232522,-12.1745070924586,2.07588278465164));
#36282=CARTESIAN_POINT('Ctrl Pts',(368.504778611106,-12.1601556614552,2.23747002720002));
#36283=CARTESIAN_POINT('Ctrl Pts',(368.828014960294,-12.1306539401921,2.53169747694085));
#36284=CARTESIAN_POINT('Ctrl Pts',(369.005900956564,-12.1155792608168,2.66301497277864));
#36285=CARTESIAN_POINT('Ctrl Pts',(369.217446443184,-12.0998220248413,2.78791598369941));
#36286=CARTESIAN_POINT('Ctrl Pts',(369.239228844746,-12.0982237706409,2.80043565073749));
#36287=CARTESIAN_POINT('Ctrl Pts',(369.269911650619,-12.096008511827,2.8175967480308));
#36288=CARTESIAN_POINT('Ctrl Pts',(369.278690073995,-12.0953788020518,2.82245290837999));
#36289=CARTESIAN_POINT('Ctrl Pts',(369.29392100273,-12.0942934636862,2.83078590207893));
#36290=CARTESIAN_POINT('Ctrl Pts',(369.3003628979,-12.0938366471131,2.83428182755363));
#36291=CARTESIAN_POINT('Ctrl Pts',(369.314012692121,-12.0928734833343,2.84162920958441));
#36292=CARTESIAN_POINT('Ctrl Pts',(369.321223421529,-12.0923674911335,2.84547528385905));
#36293=CARTESIAN_POINT('Ctrl Pts',(369.33917019943,-12.0911149122453,2.85496026455033));
#36294=CARTESIAN_POINT('Ctrl Pts',(369.349923718276,-12.0903703819586,2.86056614707844));
#36295=CARTESIAN_POINT('Ctrl Pts',(369.390639428174,-12.0875730138946,2.88150009958209));
#36296=CARTESIAN_POINT('Ctrl Pts',(369.420810608834,-12.085544087922,2.89641980602257));
#36297=CARTESIAN_POINT('Ctrl Pts',(369.654217698994,-12.0701412091494,3.00732391770185));
#36298=CARTESIAN_POINT('Ctrl Pts',(369.866784059059,-12.0577713433233,3.08229423175975));
#36299=CARTESIAN_POINT('Ctrl Pts',(370.283962469053,-12.0337453157742,3.18196243918804));
#36300=CARTESIAN_POINT('Ctrl Pts',(370.486508898001,-12.0221767290818,3.21041894804239));
#36301=CARTESIAN_POINT('Ctrl Pts',(370.717710435035,-12.0083247464554,3.22075598967847));
#36302=CARTESIAN_POINT('Ctrl Pts',(370.745062459255,-12.0066765496578,3.22162999741955));
#36303=CARTESIAN_POINT('Ctrl Pts',(370.789921452465,-12.0039564275453,3.22249171871243));
#36304=CARTESIAN_POINT('Ctrl Pts',(370.807423398502,-12.0028909272542,3.22268530686467));
#36305=CARTESIAN_POINT('Ctrl Pts',(370.838902455543,-12.000966546165,3.22277704670787));
#36306=CARTESIAN_POINT('Ctrl Pts',(370.852879061455,-12.000109302022,3.22272685519326));
#36307=CARTESIAN_POINT('Ctrl Pts',(370.882701207031,-11.9982739688793,3.22242575556139));
#36308=CARTESIAN_POINT('Ctrl Pts',(370.898546060121,-11.9972950897108,3.22214888267738));
#36309=CARTESIAN_POINT('Ctrl Pts',(370.941482826763,-11.9946320509501,3.2210817769527));
#36310=CARTESIAN_POINT('Ctrl Pts',(370.968567385448,-11.9929409150576,3.22006663539389));
#36311=CARTESIAN_POINT('Ctrl Pts',(371.115012571724,-11.9837336904496,3.21272699963873));
#36312=CARTESIAN_POINT('Ctrl Pts',(371.233950718978,-11.9760229413001,3.20010813209078));
#36313=CARTESIAN_POINT('Ctrl Pts',(371.507379194614,-11.9577658650598,3.1556170684407));
#36314=CARTESIAN_POINT('Ctrl Pts',(371.660781586098,-11.9471158236094,3.11895517610208));
#36315=CARTESIAN_POINT('Ctrl Pts',(371.968762483035,-11.9252552637023,3.02102654134208));
#36316=CARTESIAN_POINT('Ctrl Pts',(372.122557955454,-11.9140773479105,2.95871827768179));
#36317=CARTESIAN_POINT('Ctrl Pts',(372.283911797408,-11.9024959660093,2.87836872897477));
#36318=CARTESIAN_POINT('Ctrl Pts',(372.296888607273,-11.9015657094817,2.87179663999732));
#36319=CARTESIAN_POINT('Ctrl Pts',(372.3098206137,-11.9006401642978,2.86513684949403));
#36320=CARTESIAN_POINT('',(367.611569135124,-12.0643987628337,-0.00293017485288484));
#36321=CARTESIAN_POINT('Ctrl Pts',(372.309820451737,-11.6561638218248,2.86513693290211));
#36322=CARTESIAN_POINT('Ctrl Pts',(372.233646148644,-11.6619155030425,2.90436555784629));
#36323=CARTESIAN_POINT('Ctrl Pts',(372.155915978518,-11.667715600594,2.94055195391155));
#36324=CARTESIAN_POINT('Ctrl Pts',(371.922021774511,-11.684863447988,3.03828260009214));
#36325=CARTESIAN_POINT('Ctrl Pts',(371.762401954571,-11.6961879915007,3.09078170024604));
#36326=CARTESIAN_POINT('Ctrl Pts',(371.573233095442,-11.7086994482014,3.1370125642238));
#36327=CARTESIAN_POINT('Ctrl Pts',(371.546978798975,-11.7104157468404,3.1430809804797));
#36328=CARTESIAN_POINT('Ctrl Pts',(371.510558203509,-11.7127659848792,3.15101939771138));
#36329=CARTESIAN_POINT('Ctrl Pts',(371.500455218983,-11.7134146876485,3.15317066979705));
#36330=CARTESIAN_POINT('Ctrl Pts',(371.483087832725,-11.7145240537977,3.15678158454162));
#36331=CARTESIAN_POINT('Ctrl Pts',(371.475828493191,-11.7149860253362,3.158264802108));
#36332=CARTESIAN_POINT('Ctrl Pts',(371.460621876423,-11.7159500376946,3.16131720207498));
#36333=CARTESIAN_POINT('Ctrl Pts',(371.452673710002,-11.7164517790309,3.16288147387551));
#36334=CARTESIAN_POINT('Ctrl Pts',(371.43318116481,-11.7176772501,3.1666414996639));
#36335=CARTESIAN_POINT('Ctrl Pts',(371.421630369145,-11.7183991209048,3.16880413909285));
#36336=CARTESIAN_POINT('Ctrl Pts',(371.379571462711,-11.7210127829815,3.17644089381874));
#36337=CARTESIAN_POINT('Ctrl Pts',(371.348995547353,-11.7228845413085,3.18153819449621));
#36338=CARTESIAN_POINT('Ctrl Pts',(371.271972149776,-11.7275394029052,3.19323923066429));
#36339=CARTESIAN_POINT('Ctrl Pts',(371.225444078168,-11.7302965368757,3.19927160134797));
#36340=CARTESIAN_POINT('Ctrl Pts',(370.842986406272,-11.7526319702875,3.24038819394931));
#36341=CARTESIAN_POINT('Ctrl Pts',(370.503579009262,-11.7706172470013,3.2234830302667));
#36342=CARTESIAN_POINT('Ctrl Pts',(370.111641754296,-11.7940787705607,3.1413026390152));
#36343=CARTESIAN_POINT('Ctrl Pts',(370.050713090677,-11.7977974952003,3.1266604894858));
#36344=CARTESIAN_POINT('Ctrl Pts',(369.968370410376,-11.802939143971,3.10431420570989));
#36345=CARTESIAN_POINT('Ctrl Pts',(369.946551859236,-11.8043127326096,3.09814511622357));
#36346=CARTESIAN_POINT('Ctrl Pts',(369.911943237407,-11.8065101297563,3.08796409458348));
#36347=CARTESIAN_POINT('Ctrl Pts',(369.899109710719,-11.8073290634588,3.0841016362982));
#36348=CARTESIAN_POINT('Ctrl Pts',(369.872806684709,-11.8090161148345,3.0760060428892));
#36349=CARTESIAN_POINT('Ctrl Pts',(369.859340182432,-11.8098845013897,3.07176422181933));
#36350=CARTESIAN_POINT('Ctrl Pts',(369.828188527615,-11.8119043310831,3.06172626058127));
#36351=CARTESIAN_POINT('Ctrl Pts',(369.81052497947,-11.8130578875643,3.05586518729984));
#36352=CARTESIAN_POINT('Ctrl Pts',(369.755242552884,-11.8166947886424,3.03698841249678));
#36353=CARTESIAN_POINT('Ctrl Pts',(369.717814615654,-11.8191959671586,3.02342891666998));
#36354=CARTESIAN_POINT('Ctrl Pts',(369.630340167541,-11.8251360263154,2.98989268230858));
#36355=CARTESIAN_POINT('Ctrl Pts',(369.580525720259,-11.828592884644,2.96934761609316));
#36356=CARTESIAN_POINT('Ctrl Pts',(369.39899606385,-11.8414663844915,2.88909657554114));
#36357=CARTESIAN_POINT('Ctrl Pts',(369.270838623976,-11.8511109151109,2.82179952828718));
#36358=CARTESIAN_POINT('Ctrl Pts',(368.980461504223,-11.8740980524893,2.64345002079298));
#36359=CARTESIAN_POINT('Ctrl Pts',(368.822999134951,-11.8874964287456,2.52571083767808));
#36360=CARTESIAN_POINT('Ctrl Pts',(368.641845763597,-11.9034050575931,2.36250935539747));
#36361=CARTESIAN_POINT('Ctrl Pts',(368.60718137038,-11.906472889388,2.32986007244789));
#36362=CARTESIAN_POINT('Ctrl Pts',(368.56304485247,-11.9103958185939,2.28640365458869));
#36363=CARTESIAN_POINT('Ctrl Pts',(368.552905395979,-11.911298220028,2.2762864348408));
#36364=CARTESIAN_POINT('Ctrl Pts',(368.536746912794,-11.9127377203612,2.25994696046144));
#36365=CARTESIAN_POINT('Ctrl Pts',(368.530685052261,-11.9132780727926,2.25376760401024));
#36366=CARTESIAN_POINT('Ctrl Pts',(368.519083410428,-11.914312727692,2.24184537901794));
#36367=CARTESIAN_POINT('Ctrl Pts',(368.513540003973,-11.9148072990716,2.23610630427298));
#36368=CARTESIAN_POINT('Ctrl Pts',(368.500343216698,-11.9159853164569,2.22234176887064));
#36369=CARTESIAN_POINT('Ctrl Pts',(368.492709753879,-11.916667237063,2.2142971930392));
#36370=CARTESIAN_POINT('Ctrl Pts',(368.467462117026,-11.9189250638317,2.1874132328381));
#36371=CARTESIAN_POINT('Ctrl Pts',(368.450032075139,-11.9204876738813,2.16840128916409));
#36372=CARTESIAN_POINT('Ctrl Pts',(368.344532698208,-11.92998502054,2.05051673010516));
#36373=CARTESIAN_POINT('Ctrl Pts',(368.262388059105,-11.9375535760171,1.94649269399025));
#36374=CARTESIAN_POINT('Ctrl Pts',(368.112532472945,-11.9523636394316,1.73060591633995));
#36375=CARTESIAN_POINT('Ctrl Pts',(368.044761239028,-11.9595961258843,1.619100688336));
#36376=CARTESIAN_POINT('Ctrl Pts',(367.901745689382,-11.9768335638925,1.34802020291204));
#36377=CARTESIAN_POINT('Ctrl Pts',(367.832479999995,-11.9869029856521,1.18578920271957));
#36378=CARTESIAN_POINT('Ctrl Pts',(367.768152498204,-11.9990827204937,0.992722890854623));
#36379=CARTESIAN_POINT('Ctrl Pts',(367.759821191599,-12.0007333857915,0.966612088844642));
#36380=CARTESIAN_POINT('Ctrl Pts',(367.746711062784,-12.0034571678305,0.923638947765207));
#36381=CARTESIAN_POINT('Ctrl Pts',(367.741734867764,-12.00452383636,0.906837944387569));
#36382=CARTESIAN_POINT('Ctrl Pts',(367.733033131896,-12.0064500627239,0.8765536477412));
#36383=CARTESIAN_POINT('Ctrl Pts',(367.729257873778,-12.0073079784438,0.863085009950679));
#36384=CARTESIAN_POINT('Ctrl Pts',(367.721390677083,-12.0091444670223,0.834298114550317));
#36385=CARTESIAN_POINT('Ctrl Pts',(367.717323875372,-12.0101238291342,0.818973427886168));
#36386=CARTESIAN_POINT('Ctrl Pts',(367.709256713097,-12.0121297367344,0.787643690997719));
#36387=CARTESIAN_POINT('Ctrl Pts',(367.705265841131,-12.0131565561216,0.771636703934783));
#36388=CARTESIAN_POINT('Ctrl Pts',(367.695555025851,-12.0157445624619,0.731373066669527));
#36389=CARTESIAN_POINT('Ctrl Pts',(367.689993305191,-12.017310747722,0.707079719589981));
#36390=CARTESIAN_POINT('Ctrl Pts',(367.635871250697,-12.0334580580604,0.457399293725478));
#36391=CARTESIAN_POINT('Ctrl Pts',(367.61135968054,-12.04881759431,0.227531725336061));
#36392=CARTESIAN_POINT('Ctrl Pts',(367.611569184861,-12.0643988168543,-0.00292968685778758));
#36393=CARTESIAN_POINT('Ctrl Pts',(367.611569185299,-12.064398849448,-0.00293016895121727));
#36394=CARTESIAN_POINT('Ctrl Pts',(367.6117542083,-12.0781570872375,-0.206427864357887));
#36395=CARTESIAN_POINT('Ctrl Pts',(367.631213200604,-12.092003793772,-0.409474255385796));
#36396=CARTESIAN_POINT('Ctrl Pts',(367.672822275905,-12.1060932782021,-0.625568631365891));
#36397=CARTESIAN_POINT('Ctrl Pts',(367.676070129401,-12.1071450578305,-0.64176455055575));
#36398=CARTESIAN_POINT('Ctrl Pts',(367.681537530109,-12.1088400013017,-0.667981371427391));
#36399=CARTESIAN_POINT('Ctrl Pts',(367.683680630376,-12.109487045387,-0.678017680393728));
#36400=CARTESIAN_POINT('Ctrl Pts',(367.68790391966,-12.1107292439422,-0.697343194677214));
#36401=CARTESIAN_POINT('Ctrl Pts',(367.689977393266,-12.111324754986,-0.706633745173765));
#36402=CARTESIAN_POINT('Ctrl Pts',(367.693830803858,-12.1124056494757,-0.723546764713816));
#36403=CARTESIAN_POINT('Ctrl Pts',(367.695597352845,-12.112891762404,-0.731171971110376));
#36404=CARTESIAN_POINT('Ctrl Pts',(367.699614361482,-12.1139764411908,-0.748228297610602));
#36405=CARTESIAN_POINT('Ctrl Pts',(367.70187960662,-12.1145741554716,-0.757655728814642));
#36406=CARTESIAN_POINT('Ctrl Pts',(367.708611379465,-12.1163108716069,-0.785125511946817));
#36407=CARTESIAN_POINT('Ctrl Pts',(367.713191571816,-12.117443600389,-0.803139964331464));
#36408=CARTESIAN_POINT('Ctrl Pts',(367.754821781399,-12.127331997432,-0.961139879758404));
#36409=CARTESIAN_POINT('Ctrl Pts',(367.801116540184,-12.1356130786958,-1.09853822829092));
#36410=CARTESIAN_POINT('Ctrl Pts',(367.868425382003,-12.145529286286,-1.26117858748274));
#36411=CARTESIAN_POINT('Ctrl Pts',(367.880764969715,-12.1472793310625,-1.28981199337713));
#36412=CARTESIAN_POINT('Ctrl Pts',(367.966316636863,-12.1589980429197,-1.48066199187576));
#36413=CARTESIAN_POINT('Ctrl Pts',(368.052438422537,-12.1688667573075,-1.63674510195214));
#36414=CARTESIAN_POINT('Ctrl Pts',(368.208491808732,-12.1850669192214,-1.87134434351492));
#36415=CARTESIAN_POINT('Ctrl Pts',(368.270118424236,-12.1911442262168,-1.9549348308105));
#36416=CARTESIAN_POINT('Ctrl Pts',(368.351519434048,-12.1988865545592,-2.05486243783097));
#36417=CARTESIAN_POINT('Ctrl Pts',(368.367599090316,-12.2004031621987,-2.07413743980714));
#36418=CARTESIAN_POINT('Ctrl Pts',(368.394207442995,-12.2028933404432,-2.10528632118395));
#36419=CARTESIAN_POINT('Ctrl Pts',(368.404601764913,-12.2038614007074,-2.11727396063826));
#36420=CARTESIAN_POINT('Ctrl Pts',(368.424324378021,-12.2056897281283,-2.13968330065915));
#36421=CARTESIAN_POINT('Ctrl Pts',(368.433632846758,-12.2065491572045,-2.15012201225571));
#36422=CARTESIAN_POINT('Ctrl Pts',(368.45474420808,-12.2084907209646,-2.17348873104953));
#36423=CARTESIAN_POINT('Ctrl Pts',(368.466585007136,-12.2095744443927,-2.18638174774153));
#36424=CARTESIAN_POINT('Ctrl Pts',(368.497193880956,-12.2123629382171,-2.21917037543752));
#36425=CARTESIAN_POINT('Ctrl Pts',(368.516110963808,-12.2140740614256,-2.23892437584725));
#36426=CARTESIAN_POINT('Ctrl Pts',(368.684843314623,-12.2292336658742,-2.4106905148894));
#36427=CARTESIAN_POINT('Ctrl Pts',(368.849137322963,-12.2433458292923,-2.54768477596626));
#36428=CARTESIAN_POINT('Ctrl Pts',(369.204638274566,-12.2723160136977,-2.7887245465417));
#36429=CARTESIAN_POINT('Ctrl Pts',(369.395304238252,-12.2871010895774,-2.8917279797209));
#36430=CARTESIAN_POINT('Ctrl Pts',(369.625263340919,-12.3031817715121,-2.98753910223039));
#36431=CARTESIAN_POINT('Ctrl Pts',(369.655864929045,-12.3052870289112,-2.99974192270293));
#36432=CARTESIAN_POINT('Ctrl Pts',(369.69800522219,-12.3081337649691,-3.01580152624724));
#36433=CARTESIAN_POINT('Ctrl Pts',(369.709385456639,-12.3088973701244,-3.02006495879653));
#36434=CARTESIAN_POINT('Ctrl Pts',(369.728467547946,-12.3101688013097,-3.02709094761138));
#36435=CARTESIAN_POINT('Ctrl Pts',(369.736156211174,-12.3106786705317,-3.02988869681788));
#36436=CARTESIAN_POINT('Ctrl Pts',(369.75075519135,-12.3116420927194,-3.03513809899712));
#36437=CARTESIAN_POINT('Ctrl Pts',(369.757663337707,-12.3120959938415,-3.03759549297509));
#36438=CARTESIAN_POINT('Ctrl Pts',(369.774040176534,-12.3131674787552,-3.04335824206276));
#36439=CARTESIAN_POINT('Ctrl Pts',(369.783516094295,-12.31378386081,-3.04664303961672));
#36440=CARTESIAN_POINT('Ctrl Pts',(369.816741636835,-12.3159330244633,-3.0579871141462));
#36441=CARTESIAN_POINT('Ctrl Pts',(369.840570550915,-12.3174528587969,-3.06581358423771));
#36442=CARTESIAN_POINT('Ctrl Pts',(370.072634868581,-12.3320681881517,-3.13904370386693));
#36443=CARTESIAN_POINT('Ctrl Pts',(370.286944776711,-12.3441449553992,-3.18342043523946));
#36444=CARTESIAN_POINT('Ctrl Pts',(370.653116228036,-12.3647362895077,-3.22113628653369));
#36445=CARTESIAN_POINT('Ctrl Pts',(370.802993564648,-12.3731487806624,-3.22607614518034));
#36446=CARTESIAN_POINT('Ctrl Pts',(371.007654082844,-12.3850322006007,-3.21855562424913));
#36447=CARTESIAN_POINT('Ctrl Pts',(371.062582810677,-12.388259416517,-3.215126806208));
#36448=CARTESIAN_POINT('Ctrl Pts',(371.158040213895,-12.393951715271,-3.20670957445177));
#36449=CARTESIAN_POINT('Ctrl Pts',(371.19861248608,-12.3963976093135,-3.20235408048675));
#36450=CARTESIAN_POINT('Ctrl Pts',(371.257549385472,-12.3999939307747,-3.19489261949645));
#36451=CARTESIAN_POINT('Ctrl Pts',(371.275988067461,-12.4011252468538,-3.1923958368837));
#36452=CARTESIAN_POINT('Ctrl Pts',(371.308377461968,-12.4031238466458,-3.18772401181968));
#36453=CARTESIAN_POINT('Ctrl Pts',(371.322337549143,-12.4039889718342,-3.1856166835572));
#36454=CARTESIAN_POINT('Ctrl Pts',(371.349522925206,-12.4056811102607,-3.18133005924607));
#36455=CARTESIAN_POINT('Ctrl Pts',(371.362749369204,-12.406507819128,-3.17915984755733));
#36456=CARTESIAN_POINT('Ctrl Pts',(371.398318854658,-12.4087405074716,-3.17309546078506));
#36457=CARTESIAN_POINT('Ctrl Pts',(371.420634641974,-12.4101513246997,-3.1690478875971));
#36458=CARTESIAN_POINT('Ctrl Pts',(371.504473746837,-12.4154906214598,-3.15292554294454));
#36459=CARTESIAN_POINT('Ctrl Pts',(371.565679742452,-12.4194680992977,-3.13929248548913));
#36460=CARTESIAN_POINT('Ctrl Pts',(371.953872177133,-12.4452203610336,-3.04085792280429));
#36461=CARTESIAN_POINT('Ctrl Pts',(372.266119793206,-12.4686478013374,-2.90690209656326));
#36462=CARTESIAN_POINT('Ctrl Pts',(372.591529587359,-12.4940342692912,-2.70194833360715));
#36463=CARTESIAN_POINT('Ctrl Pts',(372.630672175652,-12.4971002273867,-2.67608472801488));
#36464=CARTESIAN_POINT('Ctrl Pts',(372.694717727381,-12.5021203444426,-2.63172766390991));
#36465=CARTESIAN_POINT('Ctrl Pts',(372.719942623918,-12.5040984918251,-2.61371336953807));
#36466=CARTESIAN_POINT('Ctrl Pts',(372.754368096213,-12.5067950992395,-2.58837066788114));
#36467=CARTESIAN_POINT('Ctrl Pts',(372.763793431962,-12.5075330795006,-2.58135229115478));
#36468=CARTESIAN_POINT('Ctrl Pts',(372.779650836886,-12.5087738300136,-2.56940902975383));
#36469=CARTESIAN_POINT('Ctrl Pts',(372.78610305614,-12.5092784393818,-2.56451120221236));
#36470=CARTESIAN_POINT('Ctrl Pts',(372.798421472808,-12.5102412614971,-2.5550869712785));
#36471=CARTESIAN_POINT('Ctrl Pts',(372.804290600115,-12.5106997599992,-2.55056461168414));
#36472=CARTESIAN_POINT('Ctrl Pts',(372.818304515359,-12.5117940977031,-2.53968919023706));
#36473=CARTESIAN_POINT('Ctrl Pts',(372.826434517592,-12.5124286105004,-2.53331708651532));
#36474=CARTESIAN_POINT('Ctrl Pts',(372.855661222793,-12.5147089234502,-2.5101821831586));
#36475=CARTESIAN_POINT('Ctrl Pts',(372.876578790837,-12.5163396024031,-2.49319353053628));
#36476=CARTESIAN_POINT('Ctrl Pts',(373.026031480407,-12.5280010398704,-2.3686691103941));
#36477=CARTESIAN_POINT('Ctrl Pts',(373.146234265238,-12.5374448404194,-2.25150131218711));
#36478=CARTESIAN_POINT('Ctrl Pts',(373.359786753583,-12.5555779962044,-2.00811191026386));
#36479=CARTESIAN_POINT('Ctrl Pts',(373.454114890907,-12.5642534711891,-1.88339267682397));
#36480=CARTESIAN_POINT('Ctrl Pts',(373.603757577794,-12.579984688018,-1.65242051387925));
#36481=CARTESIAN_POINT('Ctrl Pts',(373.662896443344,-12.5869203555053,-1.54900889517241));
#36482=CARTESIAN_POINT('Ctrl Pts',(373.728300777583,-12.5956897856033,-1.41834907046158));
#36483=CARTESIAN_POINT('Ctrl Pts',(373.740119215168,-12.5973256182555,-1.39397619388687));
#36484=CARTESIAN_POINT('Ctrl Pts',(373.758364430698,-12.5999356182627,-1.35510901111668));
#36485=CARTESIAN_POINT('Ctrl Pts',(373.764994052675,-12.6009027619704,-1.34071093796499));
#36486=CARTESIAN_POINT('Ctrl Pts',(373.777273736883,-12.6027303106228,-1.31351585537812));
#36487=CARTESIAN_POINT('Ctrl Pts',(373.782947237534,-12.6035898854513,-1.30072978734645));
#36488=CARTESIAN_POINT('Ctrl Pts',(373.795542200142,-12.6055330586501,-1.27183929074661));
#36489=CARTESIAN_POINT('Ctrl Pts',(373.802415830859,-12.6066182567808,-1.25571461327399));
#36490=CARTESIAN_POINT('Ctrl Pts',(373.819706714671,-12.6094130864331,-1.21421710840575));
#36491=CARTESIAN_POINT('Ctrl Pts',(373.829932049533,-12.6111291197151,-1.18876631537478));
#36492=CARTESIAN_POINT('Ctrl Pts',(373.915959652653,-12.626136811526,-0.966483301202008));
#36493=CARTESIAN_POINT('Ctrl Pts',(373.972580178387,-12.6400754043301,-0.762814937114291));
#36494=CARTESIAN_POINT('Ctrl Pts',(374.036838934751,-12.6652303425127,-0.39533131920048));
#36495=CARTESIAN_POINT('Ctrl Pts',(374.052676132839,-12.6762831120727,-0.233666969480691));
#36496=CARTESIAN_POINT('Ctrl Pts',(374.058074828667,-12.6924245341085,0.00962796764017243));
#36497=CARTESIAN_POINT('Ctrl Pts',(374.056810661789,-12.6977248817109,0.0907975905886753));
#36498=CARTESIAN_POINT('Ctrl Pts',(374.051616806316,-12.7039100781261,0.188066680497945));
#36499=CARTESIAN_POINT('Ctrl Pts',(374.05062759326,-12.7049359339655,0.204287326461232));
#36500=CARTESIAN_POINT('Ctrl Pts',(374.048894465196,-12.7065247547634,0.229558732048791));
#36501=CARTESIAN_POINT('Ctrl Pts',(374.048234935932,-12.7070922173073,0.238614743759082));
#36502=CARTESIAN_POINT('Ctrl Pts',(374.046932802362,-12.7081471202061,0.255508492960422));
#36503=CARTESIAN_POINT('Ctrl Pts',(374.046299790357,-12.7086350597758,0.263346612889715));
#36504=CARTESIAN_POINT('Ctrl Pts',(374.044788954213,-12.7097454826759,0.281237800384297));
#36505=CARTESIAN_POINT('Ctrl Pts',(374.043892598549,-12.710366926586,0.291289119642901));
#36506=CARTESIAN_POINT('Ctrl Pts',(374.041382843648,-12.7120132079993,0.318013015696647));
#36507=CARTESIAN_POINT('Ctrl Pts',(374.039686624672,-12.7130336151994,0.334677751157605));
#36508=CARTESIAN_POINT('Ctrl Pts',(374.024654089963,-12.7213812569281,0.471749781399621));
#36509=CARTESIAN_POINT('Ctrl Pts',(374.004666643777,-12.7283768241564,0.591344543833876));
#36510=CARTESIAN_POINT('Ctrl Pts',(373.965984771626,-12.7383401045756,0.762727125022461));
#36511=CARTESIAN_POINT('Ctrl Pts',(373.952632546719,-12.7414049217965,0.815600427294968));
#36512=CARTESIAN_POINT('Ctrl Pts',(373.93375679263,-12.7453315351225,0.883084127791017));
#36513=CARTESIAN_POINT('Ctrl Pts',(373.92946020549,-12.7462019627148,0.898027358878514));
#36514=CARTESIAN_POINT('Ctrl Pts',(373.874828557825,-12.7569926517417,1.08298178415095));
#36515=CARTESIAN_POINT('Ctrl Pts',(373.810655724516,-12.766856655951,1.24858446194856));
#36516=CARTESIAN_POINT('Ctrl Pts',(373.706715849474,-12.7806063867538,1.46257310957854));
#36517=CARTESIAN_POINT('Ctrl Pts',(373.678706258615,-12.7841487937767,1.51632592820138));
#36518=CARTESIAN_POINT('Ctrl Pts',(373.627802713589,-12.7903457274994,1.60763513833001));
#36519=CARTESIAN_POINT('Ctrl Pts',(373.605624456292,-12.7929759012183,1.64557219087209));
#36520=CARTESIAN_POINT('Ctrl Pts',(373.57267127624,-12.7967931184625,1.69938379028608));
#36521=CARTESIAN_POINT('Ctrl Pts',(373.562518899433,-12.797957510414,1.71563509026561));
#36522=CARTESIAN_POINT('Ctrl Pts',(373.544589298647,-12.7999943867305,1.74377407530293));
#36523=CARTESIAN_POINT('Ctrl Pts',(373.536877209764,-12.8008644435524,1.75570277887974));
#36524=CARTESIAN_POINT('Ctrl Pts',(373.520830289611,-12.8026626389804,1.78016715392233));
#36525=CARTESIAN_POINT('Ctrl Pts',(373.512485994002,-12.8035911178598,1.79269617175429));
#36526=CARTESIAN_POINT('Ctrl Pts',(373.490929217907,-12.80597339085,1.82457739949695));
#36527=CARTESIAN_POINT('Ctrl Pts',(373.477593070142,-12.8074318367744,1.84384454626085));
#36528=CARTESIAN_POINT('Ctrl Pts',(373.424554595977,-12.8131741134941,1.91871280885195));
#36529=CARTESIAN_POINT('Ctrl Pts',(373.383300777297,-12.8175169728635,1.97318781334541));
#36530=CARTESIAN_POINT('Ctrl Pts',(373.13224641922,-12.8432692579326,2.28367874991006));
#36531=CARTESIAN_POINT('Ctrl Pts',(372.885797985714,-12.8662196272001,2.50739310013837));
#36532=CARTESIAN_POINT('Ctrl Pts',(372.570733274303,-12.8911352031827,2.71535533576008));
#36533=CARTESIAN_POINT('Ctrl Pts',(372.531250598471,-12.8941833496627,2.7402030604942));
#36534=CARTESIAN_POINT('Ctrl Pts',(372.464767604646,-12.8991775411935,2.7800546391492));
#36535=CARTESIAN_POINT('Ctrl Pts',(372.438066932157,-12.9011472798606,2.79554274580632));
#36536=CARTESIAN_POINT('Ctrl Pts',(372.400915074615,-12.9038344276492,2.81638568832534));
#36537=CARTESIAN_POINT('Ctrl Pts',(372.390651938227,-12.9045711830227,2.82207006031603));
#36538=CARTESIAN_POINT('Ctrl Pts',(372.373253644609,-12.9058104740178,2.83158255195063));
#36539=CARTESIAN_POINT('Ctrl Pts',(372.36613474309,-12.9063148390825,2.83544002573733));
#36540=CARTESIAN_POINT('Ctrl Pts',(372.352470004893,-12.9072776657621,2.84277796611814));
#36541=CARTESIAN_POINT('Ctrl Pts',(372.345926618902,-12.9077364100132,2.84626271844423));
#36542=CARTESIAN_POINT('Ctrl Pts',(372.330223581879,-12.9088319435341,2.8545561183552));
#36543=CARTESIAN_POINT('Ctrl Pts',(372.32105262085,-12.90946739984,2.85934333709121));
#36544=CARTESIAN_POINT('Ctrl Pts',(372.311179410827,-12.9101470130225,2.86443678343236));
#36545=CARTESIAN_POINT('Ctrl Pts',(372.310500074469,-12.9101937516832,2.86478693732804));
#36546=CARTESIAN_POINT('Ctrl Pts',(372.309820613641,-12.9102404761534,2.86513684952402));
#36547=CARTESIAN_POINT('Origin',(370.834317853224,2.31077344927308,0.));
#36548=CARTESIAN_POINT('',(372.309820634558,-14.4057934188676,2.86513683875239));
#36549=CARTESIAN_POINT('',(372.309820586043,-14.1558998485283,2.86513686373655));
#36550=CARTESIAN_POINT('',(372.309820613641,2.31077344927308,2.86513684952399));
#36551=CARTESIAN_POINT('',(367.61156856641,-13.562992962766,0.00214402399713387));
#36552=CARTESIAN_POINT('Ctrl Pts',(372.309820634558,-14.4057934188676,2.86513683875233));
#36553=CARTESIAN_POINT('Ctrl Pts',(372.382959820302,-14.4010303765177,2.82747124787015));
#36554=CARTESIAN_POINT('Ctrl Pts',(372.454634639736,-14.3961920686039,2.78701651963437));
#36555=CARTESIAN_POINT('Ctrl Pts',(372.547881285588,-14.3896216220975,2.7295713953753));
#36556=CARTESIAN_POINT('Ctrl Pts',(372.570891775765,-14.3879770929918,2.71498997819747));
#36557=CARTESIAN_POINT('Ctrl Pts',(372.607147668188,-14.3853475157019,2.6913656551277));
#36558=CARTESIAN_POINT('Ctrl Pts',(372.620515499913,-14.3843695256475,2.68251236620994));
#36559=CARTESIAN_POINT('Ctrl Pts',(372.645394096121,-14.3825332607743,2.66576727580749));
#36560=CARTESIAN_POINT('Ctrl Pts',(372.656920780774,-14.3816759140363,2.65789971314251));
#36561=CARTESIAN_POINT('Ctrl Pts',(372.682568802527,-14.3797532865835,2.64014830757586));
#36562=CARTESIAN_POINT('Ctrl Pts',(372.696662596199,-14.3786865401734,2.63022559820126));
#36563=CARTESIAN_POINT('Ctrl Pts',(372.738069216955,-14.3755216678856,2.60057369039509));
#36564=CARTESIAN_POINT('Ctrl Pts',(372.765152344579,-14.3734114553449,2.58052917105951));
#36565=CARTESIAN_POINT('Ctrl Pts',(372.826121092228,-14.3685669504248,2.5339083607561));
#36566=CARTESIAN_POINT('Ctrl Pts',(372.859797725736,-14.3658227592624,2.50707054699286));
#36567=CARTESIAN_POINT('Ctrl Pts',(372.971201364079,-14.3565101106993,2.4145800614553));
#36568=CARTESIAN_POINT('Ctrl Pts',(373.046349533906,-14.3498296651165,2.34592852847286));
#36569=CARTESIAN_POINT('Ctrl Pts',(373.275874905621,-14.328156722674,2.11539791273994));
#36570=CARTESIAN_POINT('Ctrl Pts',(373.416703716113,-14.3128072206561,1.94097560180862));
#36571=CARTESIAN_POINT('Ctrl Pts',(373.581504569827,-14.292720980829,1.68682431361183));
#36572=CARTESIAN_POINT('Ctrl Pts',(373.622197794874,-14.2875390088689,1.61868426949237));
#36573=CARTESIAN_POINT('Ctrl Pts',(373.668361004254,-14.2814359224326,1.53446915732441));
#36574=CARTESIAN_POINT('Ctrl Pts',(373.676270727446,-14.2803814665871,1.51976974082362));
#36575=CARTESIAN_POINT('Ctrl Pts',(373.688396570875,-14.2787519441865,1.4968093486478));
#36576=CARTESIAN_POINT('Ctrl Pts',(373.692691714588,-14.2781721257322,1.48859075184633));
#36577=CARTESIAN_POINT('Ctrl Pts',(373.700549684036,-14.2771066364563,1.47339540480515));
#36578=CARTESIAN_POINT('Ctrl Pts',(373.704122539358,-14.2766203607312,1.46642421981053));
#36579=CARTESIAN_POINT('Ctrl Pts',(373.712184429058,-14.2755188925491,1.45055193239317));
#36580=CARTESIAN_POINT('Ctrl Pts',(373.716657602832,-14.2749046886393,1.44164299009492));
#36581=CARTESIAN_POINT('Ctrl Pts',(373.730234105623,-14.2730306562572,1.41428771774177));
#36582=CARTESIAN_POINT('Ctrl Pts',(373.739202426687,-14.2717788741983,1.39577446395072));
#36583=CARTESIAN_POINT('Ctrl Pts',(373.759686696425,-14.2688839102828,1.35243613433621));
#36584=CARTESIAN_POINT('Ctrl Pts',(373.771065085396,-14.267248104756,1.32754742374431));
#36585=CARTESIAN_POINT('Ctrl Pts',(373.809789460465,-14.2615708282221,1.23990780177785));
#36586=CARTESIAN_POINT('Ctrl Pts',(373.835453580168,-14.2576057437109,1.17643025079055));
#36587=CARTESIAN_POINT('Ctrl Pts',(373.909704284815,-14.2453073855096,0.974492976662644));
#36588=CARTESIAN_POINT('Ctrl Pts',(373.950872306543,-14.2371700212011,0.833504716140744));
#36589=CARTESIAN_POINT('Ctrl Pts',(374.026064586071,-14.2175044293184,0.490554448711123));
#36590=CARTESIAN_POINT('Ctrl Pts',(374.050740718488,-14.2059223217358,0.287227620574676));
#36591=CARTESIAN_POINT('Ctrl Pts',(374.056708562384,-14.1920461094147,0.0554353521423061));
#36592=CARTESIAN_POINT('Ctrl Pts',(374.057064441013,-14.1903887291902,0.0279163228751384));
#36593=CARTESIAN_POINT('Ctrl Pts',(374.05706998929,-14.1876565241123,-0.0171532497813603));
#36594=CARTESIAN_POINT('Ctrl Pts',(374.056928793026,-14.186588223383,-0.0347026831279217));
#36595=CARTESIAN_POINT('Ctrl Pts',(374.056417596576,-14.1846607970022,-0.0662289496220695));
#36596=CARTESIAN_POINT('Ctrl Pts',(374.056099964636,-14.1838033302386,-0.0802062760947148));
#36597=CARTESIAN_POINT('Ctrl Pts',(374.055229179271,-14.1819697064445,-0.109990704766894));
#36598=CARTESIAN_POINT('Ctrl Pts',(374.054650587014,-14.1809927751095,-0.125796640763847));
#36599=CARTESIAN_POINT('Ctrl Pts',(374.052771048867,-14.1783405416755,-0.168533511177363));
#36600=CARTESIAN_POINT('Ctrl Pts',(374.051248469167,-14.1766583592929,-0.195452956420964));
#36601=CARTESIAN_POINT('Ctrl Pts',(374.041297529638,-14.1676028854456,-0.339338927783878));
#36602=CARTESIAN_POINT('Ctrl Pts',(374.026828302817,-14.1600425603066,-0.455786220552487));
#36603=CARTESIAN_POINT('Ctrl Pts',(373.960066060415,-14.1352374836005,-0.826516142479432));
#36604=CARTESIAN_POINT('Ctrl Pts',(373.883425862925,-14.1173738428641,-1.07533706582195));
#36605=CARTESIAN_POINT('Ctrl Pts',(373.74421844654,-14.0946748731369,-1.38758679756752));
#36606=CARTESIAN_POINT('Ctrl Pts',(373.707756374582,-14.0892815335187,-1.46159915732633));
#36607=CARTESIAN_POINT('Ctrl Pts',(373.661168151996,-14.083060811931,-1.54766651114144));
#36608=CARTESIAN_POINT('Ctrl Pts',(373.653747723095,-14.0820882694192,-1.56114364229234));
#36609=CARTESIAN_POINT('Ctrl Pts',(373.641449574097,-14.0805065921476,-1.58310607155174));
#36610=CARTESIAN_POINT('Ctrl Pts',(373.636629304403,-14.0798940137871,-1.59162302968303));
#36611=CARTESIAN_POINT('Ctrl Pts',(373.627885568865,-14.078796150606,-1.60690951693122));
#36612=CARTESIAN_POINT('Ctrl Pts',(373.623976198221,-14.0783099984584,-1.61368680335597));
#36613=CARTESIAN_POINT('Ctrl Pts',(373.615304157931,-14.0772418968173,-1.62859495365853));
#36614=CARTESIAN_POINT('Ctrl Pts',(373.610530498217,-14.0766606641023,-1.63671918944388));
#36615=CARTESIAN_POINT('Ctrl Pts',(373.596597463081,-14.0749831783583,-1.6601953155702));
#36616=CARTESIAN_POINT('Ctrl Pts',(373.587345733388,-14.0738927043682,-1.675492361436));
#36617=CARTESIAN_POINT('Ctrl Pts',(373.512470932783,-14.0652451293225,-1.79699748838582));
#36618=CARTESIAN_POINT('Ctrl Pts',(373.440846147328,-14.0580419709269,-1.89940027668488));
#36619=CARTESIAN_POINT('Ctrl Pts',(373.174275389007,-14.0336708237858,-2.23693585166541));
#36620=CARTESIAN_POINT('Ctrl Pts',(372.952046215584,-14.0171031812076,-2.44836893354479));
#36621=CARTESIAN_POINT('Ctrl Pts',(372.667994101945,-13.9964396180221,-2.65059181889527));
#36622=CARTESIAN_POINT('Ctrl Pts',(372.632092139148,-13.9938398088349,-2.67507250791494));
#36623=CARTESIAN_POINT('Ctrl Pts',(372.580937561458,-13.990146398229,-2.70845864449811));
#36624=CARTESIAN_POINT('Ctrl Pts',(372.566089017181,-13.9890755924274,-2.71797668325954));
#36625=CARTESIAN_POINT('Ctrl Pts',(372.540092179425,-13.9872026588786,-2.73434135571468));
#36626=CARTESIAN_POINT('Ctrl Pts',(372.528978839859,-13.9864025788897,-2.74124293595799));
#36627=CARTESIAN_POINT('Ctrl Pts',(372.505623705291,-13.9847222212517,-2.75555058330692));
#36628=CARTESIAN_POINT('Ctrl Pts',(372.493374018661,-13.9838414729973,-2.76294315861555));
#36629=CARTESIAN_POINT('Ctrl Pts',(372.464052347579,-13.9817344556938,-2.78037321881766));
#36630=CARTESIAN_POINT('Ctrl Pts',(372.44693642711,-13.9805054869996,-2.79033529617702));
#36631=CARTESIAN_POINT('Ctrl Pts',(372.388169695081,-13.9762884892279,-2.82381833715494));
#36632=CARTESIAN_POINT('Ctrl Pts',(372.346089189989,-13.9732731852639,-2.84656856216098));
#36633=CARTESIAN_POINT('Ctrl Pts',(372.108282807119,-13.9562485296687,-2.96837475240721));
#36634=CARTESIAN_POINT('Ctrl Pts',(371.903377006328,-13.9415795104655,-3.0481663906488));
#36635=CARTESIAN_POINT('Ctrl Pts',(371.507306265598,-13.9137899329238,-3.15751708262114));
#36636=CARTESIAN_POINT('Ctrl Pts',(371.318422412028,-13.9007788168646,-3.19194031028099));
#36637=CARTESIAN_POINT('Ctrl Pts',(371.101158331279,-13.886766863588,-3.21179357663753));
#36638=CARTESIAN_POINT('Ctrl Pts',(371.074700769921,-13.8850769066204,-3.21388207289667));
#36639=CARTESIAN_POINT('Ctrl Pts',(371.037975892387,-13.8827565610804,-3.21632497745265));
#36640=CARTESIAN_POINT('Ctrl Pts',(371.027728962352,-13.8821118829606,-3.21695743009893));
#36641=CARTESIAN_POINT('Ctrl Pts',(371.010101777729,-13.8810077974023,-3.21796087212121));
#36642=CARTESIAN_POINT('Ctrl Pts',(371.002723021314,-13.880547106484,-3.21835545963772));
#36643=CARTESIAN_POINT('Ctrl Pts',(370.987245095855,-13.8795839425694,-3.21912978291905));
#36644=CARTESIAN_POINT('Ctrl Pts',(370.979145755956,-13.8790817789292,-3.21950433783194));
#36645=CARTESIAN_POINT('Ctrl Pts',(370.959245408341,-13.8778522930659,-3.22034938328103));
#36646=CARTESIAN_POINT('Ctrl Pts',(370.947442917026,-13.8771268619889,-3.2207855834317));
#36647=CARTESIAN_POINT('Ctrl Pts',(370.904221940353,-13.8744831850842,-3.22214508232847));
#36648=CARTESIAN_POINT('Ctrl Pts',(370.872791682018,-13.8725855892519,-3.22267364858954));
#36649=CARTESIAN_POINT('Ctrl Pts',(370.793540387236,-13.8678522942749,-3.22284676010578));
#36650=CARTESIAN_POINT('Ctrl Pts',(370.74572452772,-13.8650437088517,-3.22188698149173));
#36651=CARTESIAN_POINT('Ctrl Pts',(370.526308521112,-13.8523017492764,-3.2125939503536));
#36652=CARTESIAN_POINT('Ctrl Pts',(370.355515650009,-13.8427820520571,-3.19161188295868));
#36653=CARTESIAN_POINT('Ctrl Pts',(369.979506076188,-13.821297895616,-3.11454065240209));
#36654=CARTESIAN_POINT('Ctrl Pts',(369.776548204138,-13.8093120954196,-3.05158548845113));
#36655=CARTESIAN_POINT('Ctrl Pts',(369.555993682115,-13.7949844123601,-2.95850579948095));
#36656=CARTESIAN_POINT('Ctrl Pts',(369.530871718826,-13.7933331753907,-2.94752393661939));
#36657=CARTESIAN_POINT('Ctrl Pts',(369.489932466155,-13.7906090528347,-2.92900194496375));
#36658=CARTESIAN_POINT('Ctrl Pts',(369.474030832833,-13.7895426250041,-2.9216508459907));
#36659=CARTESIAN_POINT('Ctrl Pts',(369.44555046054,-13.7876172363621,-2.90820186354971));
#36660=CARTESIAN_POINT('Ctrl Pts',(369.432949883728,-13.7867599195693,-2.90215105645311));
#36661=CARTESIAN_POINT('Ctrl Pts',(369.420163116282,-13.7858842630214,-2.89590814871538));
#36662=CARTESIAN_POINT('Ctrl Pts',(369.419937021312,-13.7858687778962,-2.8957977291467));
#36663=CARTESIAN_POINT('Ctrl Pts',(369.419423412503,-13.7858335969847,-2.89554681994938));
#36664=CARTESIAN_POINT('Ctrl Pts',(369.419135906786,-13.7858139006363,-2.89540631403934));
#36665=CARTESIAN_POINT('Ctrl Pts',(369.418580457975,-13.7857758424659,-2.89513476010358));
#36666=CARTESIAN_POINT('Ctrl Pts',(369.418312512383,-13.7857574808575,-2.8950037178176));
#36667=CARTESIAN_POINT('Ctrl Pts',(369.417794824369,-13.7857220001333,-2.89475044667677));
#36668=CARTESIAN_POINT('Ctrl Pts',(369.417545079384,-13.7857048811757,-2.8946282226075));
#36669=CARTESIAN_POINT('Ctrl Pts',(369.417062527004,-13.7856717999805,-2.89439198623828));
#36670=CARTESIAN_POINT('Ctrl Pts',(369.416829717291,-13.7856558378738,-2.89427797804366));
#36671=CARTESIAN_POINT('Ctrl Pts',(369.416379857303,-13.7856249904511,-2.89405761183954));
#36672=CARTESIAN_POINT('Ctrl Pts',(369.416162805518,-13.7856101052832,-2.8939512576389));
#36673=CARTESIAN_POINT('Ctrl Pts',(369.415743367183,-13.7855813374358,-2.8937456766034));
#36674=CARTESIAN_POINT('Ctrl Pts',(369.415540979105,-13.7855674548697,-2.89364645296755));
#36675=CARTESIAN_POINT('Ctrl Pts',(369.415149851497,-13.7855406231272,-2.89345464619168));
#36676=CARTESIAN_POINT('Ctrl Pts',(369.414961110401,-13.7855276740329,-2.89336206571109));
#36677=CARTESIAN_POINT('Ctrl Pts',(369.414596331939,-13.7855026449676,-2.89318309184767));
#36678=CARTESIAN_POINT('Ctrl Pts',(369.414420293248,-13.7854905650704,-2.89309670079112));
#36679=CARTESIAN_POINT('Ctrl Pts',(369.414080041353,-13.785467214616,-2.89292968350416));
#36680=CARTESIAN_POINT('Ctrl Pts',(369.413915827316,-13.7854559441447,-2.89284905945031));
#36681=CARTESIAN_POINT('Ctrl Pts',(369.399052406199,-13.784435738794,-2.88555000502674));
#36682=CARTESIAN_POINT('Ctrl Pts',(369.384408646909,-13.7834229104053,-2.87821976446236));
#36683=CARTESIAN_POINT('Ctrl Pts',(369.34280321651,-13.7805229127941,-2.85699520808018));
#36684=CARTESIAN_POINT('Ctrl Pts',(369.31598153105,-13.7786263393954,-2.84283172950432));
#36685=CARTESIAN_POINT('Ctrl Pts',(369.255929342394,-13.7743173716255,-2.81002824712919));
#36686=CARTESIAN_POINT('Ctrl Pts',(369.22282190765,-13.7718976156395,-2.79117352762084));
#36687=CARTESIAN_POINT('Ctrl Pts',(369.117096494607,-13.7640249521677,-2.72845469854341));
#36688=CARTESIAN_POINT('Ctrl Pts',(369.045878288009,-13.7584949218541,-2.68231172756911));
#36689=CARTESIAN_POINT('Ctrl Pts',(368.857022539799,-13.7432162600115,-2.54908296526954));
#36690=CARTESIAN_POINT('Ctrl Pts',(368.743365791275,-13.7333248526963,-2.45671222381672));
#36691=CARTESIAN_POINT('Ctrl Pts',(368.514004177493,-13.7121100277976,-2.24282479034526));
#36692=CARTESIAN_POINT('Ctrl Pts',(368.400686537784,-13.700815447,-2.1193319262361));
#36693=CARTESIAN_POINT('Ctrl Pts',(368.28084874251,-13.6883314452662,-1.96637712221873));
#36694=CARTESIAN_POINT('Ctrl Pts',(368.26449802244,-13.686615246178,-1.9449600596472));
#36695=CARTESIAN_POINT('Ctrl Pts',(368.24225575235,-13.6842654312969,-1.9150556691456));
#36696=CARTESIAN_POINT('Ctrl Pts',(368.23613403124,-13.6836170509212,-1.90674198168176));
#36697=CARTESIAN_POINT('Ctrl Pts',(368.225690641883,-13.6825083075489,-1.89241550917802));
#36698=CARTESIAN_POINT('Ctrl Pts',(368.221349594436,-13.6820466372323,-1.88641704517071));
#36699=CARTESIAN_POINT('Ctrl Pts',(368.212306754553,-13.6810833536757,-1.87383053335703));
#36700=CARTESIAN_POINT('Ctrl Pts',(368.207609054231,-13.6805820388714,-1.86723966227124));
#36701=CARTESIAN_POINT('Ctrl Pts',(368.196159401585,-13.6793578062898,-1.85104708879848));
#36702=CARTESIAN_POINT('Ctrl Pts',(368.189434897602,-13.6786367423717,-1.84142594254094));
#36703=CARTESIAN_POINT('Ctrl Pts',(368.165176832569,-13.6760271754919,-1.80631145923769));
#36704=CARTESIAN_POINT('Ctrl Pts',(368.147957447199,-13.6741586330463,-1.78060180987894));
#36705=CARTESIAN_POINT('Ctrl Pts',(368.10562582034,-13.6695128915414,-1.7153857478109));
#36706=CARTESIAN_POINT('Ctrl Pts',(368.08099844256,-13.6667615424212,-1.67557188147986));
#36707=CARTESIAN_POINT('Ctrl Pts',(367.916574611333,-13.6479437582438,-1.39633547379169));
#36708=CARTESIAN_POINT('Ctrl Pts',(367.807309376793,-13.632985027028,-1.14027317804745));
#36709=CARTESIAN_POINT('Ctrl Pts',(367.70632921381,-13.6116528487885,-0.781596973584567));
#36710=CARTESIAN_POINT('Ctrl Pts',(367.684579531842,-13.6061090129003,-0.688732860389243));
#36711=CARTESIAN_POINT('Ctrl Pts',(367.659866652626,-13.5981460572751,-0.557190128808284));
#36712=CARTESIAN_POINT('Ctrl Pts',(367.653434067656,-13.5958345392764,-0.519210378170908));
#36713=CARTESIAN_POINT('Ctrl Pts',(367.644999344619,-13.5924124102355,-0.463344773650182));
#36714=CARTESIAN_POINT('Ctrl Pts',(367.642463658908,-13.5913186208338,-0.445542041214505));
#36715=CARTESIAN_POINT('Ctrl Pts',(367.638210461133,-13.5893609195195,-0.413778831887916));
#36716=CARTESIAN_POINT('Ctrl Pts',(367.636435090719,-13.5884988552767,-0.39982647593943));
#36717=CARTESIAN_POINT('Ctrl Pts',(367.633186368712,-13.5868301723381,-0.372888159366781));
#36718=CARTESIAN_POINT('Ctrl Pts',(367.631700565209,-13.5860239643604,-0.359903958032274));
#36719=CARTESIAN_POINT('Ctrl Pts',(367.628665579648,-13.5842792491737,-0.331873251813965));
#36720=CARTESIAN_POINT('Ctrl Pts',(367.627143276899,-13.5833399153545,-0.316824208058947));
#36721=CARTESIAN_POINT('Ctrl Pts',(367.623706862157,-13.5810526565072,-0.280285705166007));
#36722=CARTESIAN_POINT('Ctrl Pts',(367.62190251251,-13.5797013341269,-0.25878689084371));
#36723=CARTESIAN_POINT('Ctrl Pts',(367.614432138253,-13.5733140782682,-0.157595806312809));
#36724=CARTESIAN_POINT('Ctrl Pts',(367.611515424219,-13.5681940848949,-0.0777356595354613));
#36725=CARTESIAN_POINT('Ctrl Pts',(367.61156856641,-13.562992962766,0.00214402399713387));
#36726=CARTESIAN_POINT('Ctrl Pts',(367.611568563846,-13.5629932138988,0.00214016705816293));
#36727=CARTESIAN_POINT('Ctrl Pts',(367.611619927406,-13.557957112477,0.0794854733120579));
#36728=CARTESIAN_POINT('Ctrl Pts',(367.614455661285,-13.5528481869056,0.156800545342477));
#36729=CARTESIAN_POINT('Ctrl Pts',(367.639344176801,-13.5299673258588,0.498765407849578));
#36730=CARTESIAN_POINT('Ctrl Pts',(367.69127196486,-13.5116185112246,0.760187110722052));
#36731=CARTESIAN_POINT('Ctrl Pts',(367.782882992887,-13.4927122912455,1.03708523160422));
#36732=CARTESIAN_POINT('Ctrl Pts',(367.791393124169,-13.4910309177668,1.061795493531));
#36733=CARTESIAN_POINT('Ctrl Pts',(367.806892903958,-13.4880989852698,1.10508350503192));
#36734=CARTESIAN_POINT('Ctrl Pts',(367.813755260639,-13.4868421895369,1.12370505323839));
#36735=CARTESIAN_POINT('Ctrl Pts',(367.824271867526,-13.4849775772108,1.15145007036586));
#36736=CARTESIAN_POINT('Ctrl Pts',(367.827796399084,-13.4843624979651,1.16062175248465));
#36737=CARTESIAN_POINT('Ctrl Pts',(367.833929114425,-13.4833091288076,1.17636514898691));
#36738=CARTESIAN_POINT('Ctrl Pts',(367.836517029087,-13.4828696516199,1.18294453364756));
#36739=CARTESIAN_POINT('Ctrl Pts',(367.842475177597,-13.4818692528679,1.19794710675121));
#36740=CARTESIAN_POINT('Ctrl Pts',(367.845859337157,-13.4813091751001,1.20636460854323));
#36741=CARTESIAN_POINT('Ctrl Pts',(367.855237110171,-13.4797789420895,1.22940853161697));
#36742=CARTESIAN_POINT('Ctrl Pts',(367.86130294611,-13.478813005324,1.24400554526578));
#36743=CARTESIAN_POINT('Ctrl Pts',(367.893149447667,-13.4738597185039,1.3190784108256));
#36744=CARTESIAN_POINT('Ctrl Pts',(367.92067064821,-13.4699678988689,1.37880409079837));
#36745=CARTESIAN_POINT('Ctrl Pts',(368.076266780615,-13.4496749719134,1.69097209189934));
#36746=CARTESIAN_POINT('Ctrl Pts',(368.235359057283,-13.4344264362882,1.92657030279664));
#36747=CARTESIAN_POINT('Ctrl Pts',(368.472693005957,-13.4139335943455,2.19417633649147));
#36748=CARTESIAN_POINT('Ctrl Pts',(368.524107252617,-13.4096068135094,2.2482454517249));
#36749=CARTESIAN_POINT('Ctrl Pts',(368.602244660278,-13.4031480404878,2.32490499330277));
#36750=CARTESIAN_POINT('Ctrl Pts',(368.627534854404,-13.4010745231461,2.34892371680636));
#36751=CARTESIAN_POINT('Ctrl Pts',(368.673948398402,-13.3972952285242,2.39159256691016));
#36752=CARTESIAN_POINT('Ctrl Pts',(368.694936188115,-13.395595555034,2.41038528086994));
#36753=CARTESIAN_POINT('Ctrl Pts',(368.728078139256,-13.3929244134895,2.4392871076154));
#36754=CARTESIAN_POINT('Ctrl Pts',(368.740065195887,-13.3919608522778,2.44958631597652));
#36755=CARTESIAN_POINT('Ctrl Pts',(368.761725899739,-13.3902239997095,2.46792185968114));
#36756=CARTESIAN_POINT('Ctrl Pts',(368.771371809608,-13.389452058033,2.47599057453288));
#36757=CARTESIAN_POINT('Ctrl Pts',(368.793558802275,-13.3876797765275,2.49433013514207));
#36758=CARTESIAN_POINT('Ctrl Pts',(368.80613056884,-13.3866779330902,2.50456316574871));
#36759=CARTESIAN_POINT('Ctrl Pts',(368.840639518646,-13.383934055128,2.53222217638655));
#36760=CARTESIAN_POINT('Ctrl Pts',(368.862727185813,-13.3821844883585,2.54945731733406));
#36761=CARTESIAN_POINT('Ctrl Pts',(368.982607180709,-13.372721866308,2.64051081783952));
#36762=CARTESIAN_POINT('Ctrl Pts',(369.084313404639,-13.3648046876333,2.70898652628737));
#36763=CARTESIAN_POINT('Ctrl Pts',(369.386402610686,-13.3416147704767,2.88825159746158));
#36764=CARTESIAN_POINT('Ctrl Pts',(369.595012725193,-13.3259379015153,2.98371646321091));
#36765=CARTESIAN_POINT('Ctrl Pts',(369.911412793433,-13.3036251017204,3.0895575315269));
#36766=CARTESIAN_POINT('Ctrl Pts',(370.012460965395,-13.2967134845157,3.11796011900538));
#36767=CARTESIAN_POINT('Ctrl Pts',(370.131567631651,-13.2889446623812,3.14524375545559));
#36768=CARTESIAN_POINT('Ctrl Pts',(370.148442398851,-13.2878527382977,3.14896666336384));
#36769=CARTESIAN_POINT('Ctrl Pts',(370.174441044922,-13.2861847118285,3.15448356965894));
#36770=CARTESIAN_POINT('Ctrl Pts',(370.18354381022,-13.2856033777491,3.15637404998738));
#36771=CARTESIAN_POINT('Ctrl Pts',(370.200329550209,-13.2845364825549,3.15978444327086));
#36772=CARTESIAN_POINT('Ctrl Pts',(370.208009871634,-13.2840503041112,3.16131574043263));
#36773=CARTESIAN_POINT('Ctrl Pts',(370.225449333487,-13.282950789669,3.16472675845341));
#36774=CARTESIAN_POINT('Ctrl Pts',(370.235211628193,-13.2823384272811,3.16658934300879));
#36775=CARTESIAN_POINT('Ctrl Pts',(370.260601800901,-13.2807535193165,3.17131200857584));
#36776=CARTESIAN_POINT('Ctrl Pts',(370.276242698395,-13.2797847950483,3.17410177992173));
#36777=CARTESIAN_POINT('Ctrl Pts',(370.383404182243,-13.2731957956341,3.19239890952743));
#36778=CARTESIAN_POINT('Ctrl Pts',(370.475545808282,-13.2677694422553,3.20406302671581));
#36779=CARTESIAN_POINT('Ctrl Pts',(370.649829625188,-13.2577409588413,3.21851085224441));
#36780=CARTESIAN_POINT('Ctrl Pts',(370.731820691672,-13.253120069872,3.22216439074434));
#36781=CARTESIAN_POINT('Ctrl Pts',(370.946559975826,-13.2410832183528,3.22352726875965));
#36782=CARTESIAN_POINT('Ctrl Pts',(371.07918011889,-13.2337104991944,3.21617290162159));
#36783=CARTESIAN_POINT('Ctrl Pts',(371.308176168338,-13.220650542556,3.18922506027394));
#36784=CARTESIAN_POINT('Ctrl Pts',(371.404808141843,-13.2150369429599,3.17336365952173));
#36785=CARTESIAN_POINT('Ctrl Pts',(371.541622956355,-13.206838688433,3.1444551470027));
#36786=CARTESIAN_POINT('Ctrl Pts',(371.582507278427,-13.2043566270811,3.13497863405927));
#36787=CARTESIAN_POINT('Ctrl Pts',(371.655205642414,-13.1998779904951,3.11662491904643));
#36788=CARTESIAN_POINT('Ctrl Pts',(371.687090636013,-13.1978910230441,3.10805181873635));
#36789=CARTESIAN_POINT('Ctrl Pts',(371.735279867953,-13.1948510444987,3.09429755986037));
#36790=CARTESIAN_POINT('Ctrl Pts',(371.751684446398,-13.1938096166597,3.08947381557511));
#36791=CARTESIAN_POINT('Ctrl Pts',(371.781398649639,-13.1919109715576,3.08047886756549));
#36792=CARTESIAN_POINT('Ctrl Pts',(371.79472113775,-13.1910551995858,3.07635134694511));
#36793=CARTESIAN_POINT('Ctrl Pts',(371.823400530402,-13.1892030475853,3.06726155900706));
#36794=CARTESIAN_POINT('Ctrl Pts',(371.838747738697,-13.1882057301692,3.06227017156905));
#36795=CARTESIAN_POINT('Ctrl Pts',(371.880334357556,-13.1854861558645,3.04839865894157));
#36796=CARTESIAN_POINT('Ctrl Pts',(371.906497336331,-13.1837565862836,3.03929531144641));
#36797=CARTESIAN_POINT('Ctrl Pts',(372.042965976973,-13.1746346813086,2.98983000534895));
#36798=CARTESIAN_POINT('Ctrl Pts',(372.151109583158,-13.1670555444702,2.94380158585669));
#36799=CARTESIAN_POINT('Ctrl Pts',(372.274353687302,-13.1580053499999,2.88319451772756));
#36800=CARTESIAN_POINT('Ctrl Pts',(372.292131192624,-13.1566896271526,2.87424663801461));
#36801=CARTESIAN_POINT('Ctrl Pts',(372.309820665215,-13.1553703139997,2.86513682296442));
#36802=CARTESIAN_POINT('Ctrl Pts',(372.309820613641,-12.9102404761534,2.86513684952402));
#36803=CARTESIAN_POINT('Ctrl Pts',(372.286441448171,-12.9118481907954,2.87717677117527));
#36804=CARTESIAN_POINT('Ctrl Pts',(372.262914918194,-12.913439105659,2.8889305350896));
#36805=CARTESIAN_POINT('Ctrl Pts',(372.091259356577,-12.9248716141687,2.9720791210119));
#36806=CARTESIAN_POINT('Ctrl Pts',(371.937984292497,-12.93414837264,3.03234062545723));
#36807=CARTESIAN_POINT('Ctrl Pts',(371.631953577968,-12.9520831075474,3.12636035604413));
#36808=CARTESIAN_POINT('Ctrl Pts',(371.480029325723,-12.9607269411464,3.16123498556991));
#36809=CARTESIAN_POINT('Ctrl Pts',(371.205434394874,-12.9765912106468,3.20364146885486));
#36810=CARTESIAN_POINT('Ctrl Pts',(371.083732505223,-12.9837023403462,3.21540566941334));
#36811=CARTESIAN_POINT('Ctrl Pts',(370.934409147797,-12.9926698366404,3.2213108124567));
#36812=CARTESIAN_POINT('Ctrl Pts',(370.907141152546,-12.9943169823515,3.22204256883709));
#36813=CARTESIAN_POINT('Ctrl Pts',(370.863976761459,-12.9969408946726,3.22265270955231));
#36814=CARTESIAN_POINT('Ctrl Pts',(370.848084532995,-12.9979105066855,3.22275978031297));
#36815=CARTESIAN_POINT('Ctrl Pts',(370.818209505811,-12.999740160901,3.22274007710108));
#36816=CARTESIAN_POINT('Ctrl Pts',(370.80422701618,-13.0005993515836,3.22263985191666));
#36817=CARTESIAN_POINT('Ctrl Pts',(370.77278116585,-13.0025382309515,3.22220978039875));
#36818=CARTESIAN_POINT('Ctrl Pts',(370.755319050345,-13.0036194899701,3.22182895304918));
#36819=CARTESIAN_POINT('Ctrl Pts',(370.71065148109,-13.0063974048413,3.22049145652653));
#36820=CARTESIAN_POINT('Ctrl Pts',(370.683453910574,-13.0081003321547,3.21933201004996));
#36821=CARTESIAN_POINT('Ctrl Pts',(370.491005328473,-13.0202342218608,3.2086838016476));
#36822=CARTESIAN_POINT('Ctrl Pts',(370.326711147957,-13.0310516420342,3.1868222384294));
#36823=CARTESIAN_POINT('Ctrl Pts',(369.958765212766,-13.0562041397443,3.10868275352858));
#36824=CARTESIAN_POINT('Ctrl Pts',(369.75748295412,-13.0706473433724,3.04481935190261));
#36825=CARTESIAN_POINT('Ctrl Pts',(369.491545499704,-13.0898216482894,2.93074635264705));
#36826=CARTESIAN_POINT('Ctrl Pts',(369.420369690378,-13.0949577700784,2.89707862443679));
#36827=CARTESIAN_POINT('Ctrl Pts',(369.336185061289,-13.1009785614437,2.85341470315282));
#36828=CARTESIAN_POINT('Ctrl Pts',(369.321933237326,-13.1019958994197,2.84588652780748));
#36829=CARTESIAN_POINT('Ctrl Pts',(369.299767029154,-13.1035744491439,2.83396422894176));
#36830=CARTESIAN_POINT('Ctrl Pts',(369.2918138888,-13.104140067464,2.82964326497738));
#36831=CARTESIAN_POINT('Ctrl Pts',(369.276980814297,-13.1051934064889,2.82150329148875));
#36832=CARTESIAN_POINT('Ctrl Pts',(369.270096712352,-13.1056816107886,2.81769261997482));
#36833=CARTESIAN_POINT('Ctrl Pts',(369.254377410618,-13.1067949705037,2.80891588984633));
#36834=CARTESIAN_POINT('Ctrl Pts',(369.245551626509,-13.107419065559,2.80393333760559));
#36835=CARTESIAN_POINT('Ctrl Pts',(369.222071217853,-13.109077117009,2.79053113013592));
#36836=CARTESIAN_POINT('Ctrl Pts',(369.207458853609,-13.110106542019,2.78203756709756));
#36837=CARTESIAN_POINT('Ctrl Pts',(369.05425721264,-13.1208811750762,2.69136793071538));
#36838=CARTESIAN_POINT('Ctrl Pts',(368.92193049366,-13.1300352627029,2.59901242594719));
#36839=CARTESIAN_POINT('Ctrl Pts',(368.643651016654,-13.1502022446611,2.37198062945402));
#36840=CARTESIAN_POINT('Ctrl Pts',(368.502113231917,-13.1611368512133,2.23296483055141));
#36841=CARTESIAN_POINT('Ctrl Pts',(368.309966137865,-13.1782697287666,2.00590670831466));
#36842=CARTESIAN_POINT('Ctrl Pts',(368.249261099568,-13.184102314845,1.92704230999386));
#36843=CARTESIAN_POINT('Ctrl Pts',(368.177579646931,-13.1916240614231,1.82442341090055));
#36844=CARTESIAN_POINT('Ctrl Pts',(368.163108733336,-13.1931782950302,1.80316955900734));
#36845=CARTESIAN_POINT('Ctrl Pts',(368.140296556113,-13.1956879367448,1.76878733534828));
#36846=CARTESIAN_POINT('Ctrl Pts',(368.131793138716,-13.1966372353208,1.75576750772298));
#36847=CARTESIAN_POINT('Ctrl Pts',(368.115791465747,-13.1984504407747,1.7308752149771));
#36848=CARTESIAN_POINT('Ctrl Pts',(368.108275906739,-13.1993136766097,1.71901425978035));
#36849=CARTESIAN_POINT('Ctrl Pts',(368.091285776715,-13.2012921730912,1.69180903070548));
#36850=CARTESIAN_POINT('Ctrl Pts',(368.081862072861,-13.2024092721472,1.67643369242913));
#36851=CARTESIAN_POINT('Ctrl Pts',(368.053129705791,-13.2058774746273,1.62865973149475));
#36852=CARTESIAN_POINT('Ctrl Pts',(368.034260918995,-13.2082443917468,1.59600156753857));
#36853=CARTESIAN_POINT('Ctrl Pts',(367.882553599153,-13.2280451782023,1.3224518192703));
#36854=CARTESIAN_POINT('Ctrl Pts',(367.780511068324,-13.2466077894303,1.06583145084524));
#36855=CARTESIAN_POINT('Ctrl Pts',(367.684067631582,-13.2728850866084,0.689197048027816));
#36856=CARTESIAN_POINT('Ctrl Pts',(367.661694710313,-13.2805421359322,0.577524557258675));
#36857=CARTESIAN_POINT('Ctrl Pts',(367.639802412825,-13.2904920994799,0.427350364695475));
#36858=CARTESIAN_POINT('Ctrl Pts',(367.634992214044,-13.292957093208,0.389708792662808));
#36859=CARTESIAN_POINT('Ctrl Pts',(367.627959231019,-13.2970901554726,0.325701330360645));
#36860=CARTESIAN_POINT('Ctrl Pts',(367.625394342988,-13.2987731905339,0.299377656379266));
#36861=CARTESIAN_POINT('Ctrl Pts',(367.622218740492,-13.3011347187371,0.262027954688159));
#36862=CARTESIAN_POINT('Ctrl Pts',(367.621340257219,-13.3018270603767,0.251026562332427));
#36863=CARTESIAN_POINT('Ctrl Pts',(367.61992470504,-13.3030140191443,0.232072775333055));
#36864=CARTESIAN_POINT('Ctrl Pts',(367.619360595705,-13.3035101189282,0.224122560233915));
#36865=CARTESIAN_POINT('Ctrl Pts',(367.618243879003,-13.3045428646993,0.207511598722008));
#36866=CARTESIAN_POINT('Ctrl Pts',(367.617696753942,-13.3050792063444,0.198850645169217));
#36867=CARTESIAN_POINT('Ctrl Pts',(367.616333495844,-13.3065018251594,0.175790330038743));
#36868=CARTESIAN_POINT('Ctrl Pts',(367.615579014496,-13.3073847380687,0.161387330596565));
#36869=CARTESIAN_POINT('Ctrl Pts',(367.612708634049,-13.3112161736672,0.0985153197607862));
#36870=CARTESIAN_POINT('Ctrl Pts',(367.611590537686,-13.314113725755,0.0500044601927247));
#36871=CARTESIAN_POINT('Ctrl Pts',(367.61152611906,-13.3223474708209,-0.0898895087334478));
#36872=CARTESIAN_POINT('Ctrl Pts',(367.615370097351,-13.3275739217479,-0.181230011163106));
#36873=CARTESIAN_POINT('Ctrl Pts',(367.631837053038,-13.3385888302066,-0.375432012577366));
#36874=CARTESIAN_POINT('Ctrl Pts',(367.645547218232,-13.3443540436448,-0.478095287026382));
#36875=CARTESIAN_POINT('Ctrl Pts',(367.699506737512,-13.3611356608664,-0.773064853962441));
#36876=CARTESIAN_POINT('Ctrl Pts',(367.752410616362,-13.3722147322438,-0.962551610862094));
#36877=CARTESIAN_POINT('Ctrl Pts',(367.835582377936,-13.3860994397021,-1.18114967775128));
#36878=CARTESIAN_POINT('Ctrl Pts',(367.849554857877,-13.38834846445,-1.21602578044464));
#36879=CARTESIAN_POINT('Ctrl Pts',(367.872057632562,-13.391851202847,-1.26946796292063));
#36880=CARTESIAN_POINT('Ctrl Pts',(367.880160390833,-13.3930905602898,-1.28821123330226));
#36881=CARTESIAN_POINT('Ctrl Pts',(367.894233939394,-13.3952073447871,-1.31993493907177));
#36882=CARTESIAN_POINT('Ctrl Pts',(367.900113996605,-13.3960816555932,-1.33295513097699));
#36883=CARTESIAN_POINT('Ctrl Pts',(367.912200235318,-13.3978588092789,-1.35925013091248));
#36884=CARTESIAN_POINT('Ctrl Pts',(367.918410770279,-13.3987617862099,-1.37252255485698));
#36885=CARTESIAN_POINT('Ctrl Pts',(367.933974561353,-13.4010000345116,-1.40520120538701));
#36886=CARTESIAN_POINT('Ctrl Pts',(367.943432190366,-13.40233890062,-1.42455666311944));
#36887=CARTESIAN_POINT('Ctrl Pts',(367.979730626407,-13.4074000944877,-1.49699273367187));
#36888=CARTESIAN_POINT('Ctrl Pts',(368.007843817285,-13.4111665687017,-1.54941900455738));
#36889=CARTESIAN_POINT('Ctrl Pts',(368.08266968058,-13.4208287695286,-1.68013605331761));
#36890=CARTESIAN_POINT('Ctrl Pts',(368.131280990857,-13.4267869839536,-1.75727464185757));
#36891=CARTESIAN_POINT('Ctrl Pts',(368.288882662348,-13.4451693581102,-1.98532149386245));
#36892=CARTESIAN_POINT('Ctrl Pts',(368.40772836387,-13.4578510523412,-2.12894281901863));
#36893=CARTESIAN_POINT('Ctrl Pts',(368.629914280375,-13.4791617846146,-2.35452146243552));
#36894=CARTESIAN_POINT('Ctrl Pts',(368.727119483038,-13.4878444156479,-2.44190274432244));
#36895=CARTESIAN_POINT('Ctrl Pts',(368.842539968626,-13.4972326517366,-2.53361824978247));
#36896=CARTESIAN_POINT('Ctrl Pts',(368.855793124139,-13.4982977068734,-2.54398123059253));
#36897=CARTESIAN_POINT('Ctrl Pts',(368.877141753162,-13.4999919089834,-2.56040651717105));
#36898=CARTESIAN_POINT('Ctrl Pts',(368.885185468138,-13.5006254434494,-2.56653516861279));
#36899=CARTESIAN_POINT('Ctrl Pts',(368.899537156368,-13.5017470900766,-2.57736359295761));
#36900=CARTESIAN_POINT('Ctrl Pts',(368.905833650295,-13.5022362244657,-2.58207825580126));
#36901=CARTESIAN_POINT('Ctrl Pts',(368.919424265962,-13.5032855859277,-2.59217713514573));
#36902=CARTESIAN_POINT('Ctrl Pts',(368.926723869801,-13.5038452861916,-2.59755364711292));
#36903=CARTESIAN_POINT('Ctrl Pts',(368.947118509198,-13.5053984723475,-2.6124429495335));
#36904=CARTESIAN_POINT('Ctrl Pts',(368.960262871797,-13.5063874311281,-2.621888151746));
#36905=CARTESIAN_POINT('Ctrl Pts',(369.038745747931,-13.5122246628598,-2.67739216387715));
#36906=CARTESIAN_POINT('Ctrl Pts',(369.105714076279,-13.5169292039206,-2.7211099237281));
#36907=CARTESIAN_POINT('Ctrl Pts',(369.361522119318,-13.5341642077513,-2.87484442207167));
#36908=CARTESIAN_POINT('Ctrl Pts',(369.559769261021,-13.5461176600429,-2.96806263918945));
#36909=CARTESIAN_POINT('Ctrl Pts',(369.91389369616,-13.5673162083844,-3.09249602278798));
#36910=CARTESIAN_POINT('Ctrl Pts',(370.065432153398,-13.576336753536,-3.13361104587745));
#36911=CARTESIAN_POINT('Ctrl Pts',(370.245815020426,-13.5873393023443,-3.16867619986333));
#36912=CARTESIAN_POINT('Ctrl Pts',(370.272343236258,-13.5889635615388,-3.17348844447893));
#36913=CARTESIAN_POINT('Ctrl Pts',(370.316073489549,-13.5916525827218,-3.18085564732622));
#36914=CARTESIAN_POINT('Ctrl Pts',(370.33324169018,-13.5927111781906,-3.18360527232994));
#36915=CARTESIAN_POINT('Ctrl Pts',(370.364248977605,-13.5946286782402,-3.18831431226065));
#36916=CARTESIAN_POINT('Ctrl Pts',(370.378080242129,-13.5954860048598,-3.19032288868732));
#36917=CARTESIAN_POINT('Ctrl Pts',(370.407719992446,-13.5973276749636,-3.19443048668303));
#36918=CARTESIAN_POINT('Ctrl Pts',(370.423531819054,-13.5983128547538,-3.19650225850004));
#36919=CARTESIAN_POINT('Ctrl Pts',(370.46667817246,-13.6010088363461,-3.20183016298354));
#36920=CARTESIAN_POINT('Ctrl Pts',(370.49403959225,-13.602726903101,-3.20485350009033));
#36921=CARTESIAN_POINT('Ctrl Pts',(370.647330769736,-13.6124016167754,-3.21980648017633));
#36922=CARTESIAN_POINT('Ctrl Pts',(370.773824213373,-13.6205774322014,-3.22466302329149));
#36923=CARTESIAN_POINT('Ctrl Pts',(371.04773027127,-13.6386776900056,-3.2190570557427));
#36924=CARTESIAN_POINT('Ctrl Pts',(371.194807116949,-13.6486485731016,-3.20591877876712));
#36925=CARTESIAN_POINT('Ctrl Pts',(371.506385445597,-13.6699907999034,-3.15636998119395));
#36926=CARTESIAN_POINT('Ctrl Pts',(371.670013244976,-13.6813332456391,-3.11704510448327));
#36927=CARTESIAN_POINT('Ctrl Pts',(371.855465674427,-13.6938609177849,-3.05681216452416));
#36928=CARTESIAN_POINT('Ctrl Pts',(371.88098647857,-13.6955771186469,-3.04816803683828));
#36929=CARTESIAN_POINT('Ctrl Pts',(371.916137600917,-13.6979272475361,-3.03576848349016));
#36930=CARTESIAN_POINT('Ctrl Pts',(371.925861964596,-13.698575937143,-3.03228555904644));
#36931=CARTESIAN_POINT('Ctrl Pts',(371.942532723594,-13.6996852867208,-3.02622409267568));
#36932=CARTESIAN_POINT('Ctrl Pts',(371.949487209822,-13.7001472547651,-3.02366826333973));
#36933=CARTESIAN_POINT('Ctrl Pts',(371.964026624075,-13.7011112666287,-3.01826792639088));
#36934=CARTESIAN_POINT('Ctrl Pts',(371.971609725868,-13.7016130109258,-3.0154187736737));
#36935=CARTESIAN_POINT('Ctrl Pts',(371.99016701882,-13.7028385004059,-3.00836639485828));
#36936=CARTESIAN_POINT('Ctrl Pts',(372.001129253375,-13.7035603865304,-3.00413162589996));
#36937=CARTESIAN_POINT('Ctrl Pts',(372.040920960685,-13.7061741677018,-2.98850920993887));
#36938=CARTESIAN_POINT('Ctrl Pts',(372.069609935322,-13.7080460274139,-2.97676535690087));
#36939=CARTESIAN_POINT('Ctrl Pts',(372.141281523077,-13.712701193836,-2.94621186656439));
#36940=CARTESIAN_POINT('Ctrl Pts',(372.18403217977,-13.7154585268944,-2.92687377064477));
#36941=CARTESIAN_POINT('Ctrl Pts',(372.531046997476,-13.73779952212,-2.76068182405692));
#36942=CARTESIAN_POINT('Ctrl Pts',(372.810915458976,-13.7557894625375,-2.5677531210639));
#36943=CARTESIAN_POINT('Ctrl Pts',(373.101056629995,-13.7792529894048,-2.29170871048624));
#36944=CARTESIAN_POINT('Ctrl Pts',(373.14512481176,-13.7829673123751,-2.24726587778122));
#36945=CARTESIAN_POINT('Ctrl Pts',(373.203351313582,-13.788103794728,-2.18501982654348));
#36946=CARTESIAN_POINT('Ctrl Pts',(373.21865792552,-13.7894767495379,-2.1683066107217));
#36947=CARTESIAN_POINT('Ctrl Pts',(373.24273233124,-13.7916733861606,-2.14145670716934));
#36948=CARTESIAN_POINT('Ctrl Pts',(373.251615543488,-13.7924921993686,-2.13142417053377));
#36949=CARTESIAN_POINT('Ctrl Pts',(373.269729978326,-13.7941791914049,-2.11070715889527));
#36950=CARTESIAN_POINT('Ctrl Pts',(373.278954055497,-13.7950476403,-2.10001684711344));
#36951=CARTESIAN_POINT('Ctrl Pts',(373.300176618383,-13.7970679369184,-2.07509149318551));
#36952=CARTESIAN_POINT('Ctrl Pts',(373.312122505579,-13.7982219010803,-2.0608125184652));
#36953=CARTESIAN_POINT('Ctrl Pts',(373.349888968601,-13.8019247485918,-2.01486698551734));
#36954=CARTESIAN_POINT('Ctrl Pts',(373.375230504184,-13.804492686541,-1.98281357161192));
#36955=CARTESIAN_POINT('Ctrl Pts',(373.433315409033,-13.8105814537097,-1.90640189792378));
#36956=CARTESIAN_POINT('Ctrl Pts',(373.465542668351,-13.8141209117993,-1.86166911273971));
#36957=CARTESIAN_POINT('Ctrl Pts',(373.581268781811,-13.8274526996217,-1.69202512678628));
#36958=CARTESIAN_POINT('Ctrl Pts',(373.657141591922,-13.8374910907921,-1.56216070074749));
#36959=CARTESIAN_POINT('Ctrl Pts',(373.819915694065,-13.8623021416418,-1.23269299518507));
#36960=CARTESIAN_POINT('Ctrl Pts',(373.896216542839,-13.8771449200178,-1.02864792981419));
#36961=CARTESIAN_POINT('Ctrl Pts',(373.957839906154,-13.8927116088205,-0.793958151326303));
#36962=CARTESIAN_POINT('Ctrl Pts',(373.963985783887,-13.8943238182866,-0.769375264308963));
#36963=CARTESIAN_POINT('Ctrl Pts',(373.972168925151,-13.8965554005894,-0.734921541099628));
#36964=CARTESIAN_POINT('Ctrl Pts',(373.974450623041,-13.8971877114994,-0.725110484981698));
#36965=CARTESIAN_POINT('Ctrl Pts',(373.978316116783,-13.8982765190564,-0.70812880337608));
#36966=CARTESIAN_POINT('Ctrl Pts',(373.979921457231,-13.8987342189227,-0.700963231882924));
#36967=CARTESIAN_POINT('Ctrl Pts',(373.983260885726,-13.8996980689643,-0.685814894684934));
#36968=CARTESIAN_POINT('Ctrl Pts',(373.984989139596,-13.9002038701308,-0.677830907726856));
#36969=CARTESIAN_POINT('Ctrl Pts',(373.989199847953,-13.9014540086259,-0.658014682701625));
#36970=CARTESIAN_POINT('Ctrl Pts',(373.991646143872,-13.9021963108078,-0.646174743527935));
#36971=CARTESIAN_POINT('Ctrl Pts',(374.00058990562,-13.9049729664398,-0.601623687266634));
#36972=CARTESIAN_POINT('Ctrl Pts',(374.006646370228,-13.9069838733238,-0.568824884895273));
#36973=CARTESIAN_POINT('Ctrl Pts',(374.048695384909,-13.9220592638356,-0.319492168098219));
#36974=CARTESIAN_POINT('Ctrl Pts',(374.062994254528,-13.9341635823893,-0.0998567989383284));
#36975=CARTESIAN_POINT('Ctrl Pts',(374.047073243879,-13.9581918143032,0.329040435217189));
#36976=CARTESIAN_POINT('Ctrl Pts',(374.01887701453,-13.970052312387,0.537244822403206));
#36977=CARTESIAN_POINT('Ctrl Pts',(373.964361770695,-13.9842382770039,0.767915933856757));
#36978=CARTESIAN_POINT('Ctrl Pts',(373.957713286412,-13.9858901114944,0.794525458908267));
#36979=CARTESIAN_POINT('Ctrl Pts',(373.946260492195,-13.9886154320116,0.837996312467507));
#36980=CARTESIAN_POINT('Ctrl Pts',(373.941656710622,-13.9896824572253,0.854909360333761));
#36981=CARTESIAN_POINT('Ctrl Pts',(373.933131291607,-13.9916090710798,0.885250534677492));
#36982=CARTESIAN_POINT('Ctrl Pts',(373.929259736393,-13.9924670147716,0.898692363991566));
#36983=CARTESIAN_POINT('Ctrl Pts',(373.920814607482,-13.9943032837923,0.927311495096885));
#36984=CARTESIAN_POINT('Ctrl Pts',(373.916216334613,-13.9952823963435,0.942481065620265));
#36985=CARTESIAN_POINT('Ctrl Pts',(373.903457628865,-13.9979446704448,0.983479699779878));
#36986=CARTESIAN_POINT('Ctrl Pts',(373.895083299703,-13.9996347940009,1.00924035391709));
#36987=CARTESIAN_POINT('Ctrl Pts',(373.848153266492,-14.0088114639682,1.14764481084955));
#36988=CARTESIAN_POINT('Ctrl Pts',(373.803706827241,-14.016491061896,1.25817959056921));
#36989=CARTESIAN_POINT('Ctrl Pts',(373.687045960847,-14.0346272231469,1.50746757623478));
#36990=CARTESIAN_POINT('Ctrl Pts',(373.61064550124,-14.0451844921597,1.64393250650828));
#36991=CARTESIAN_POINT('Ctrl Pts',(373.432411304373,-14.0670839221323,1.91418462638725));
#36992=CARTESIAN_POINT('Ctrl Pts',(373.329385395488,-14.0783940545185,2.0466658113701));
#36993=CARTESIAN_POINT('Ctrl Pts',(373.198365967598,-14.0908925000118,2.1904611785077));
#36994=CARTESIAN_POINT('Ctrl Pts',(373.179967713129,-14.0926089168508,2.21015169310762));
#36995=CARTESIAN_POINT('Ctrl Pts',(373.154177656337,-14.0949592868305,2.23706833940101));
#36996=CARTESIAN_POINT('Ctrl Pts',(373.146995412898,-14.0956080055059,2.24449254243677));
#36997=CARTESIAN_POINT('Ctrl Pts',(373.134600289968,-14.0967173916809,2.2571825736921));
#36998=CARTESIAN_POINT('Ctrl Pts',(373.129404770621,-14.0971793674422,2.26246513873443));
#36999=CARTESIAN_POINT('Ctrl Pts',(373.1184909944,-14.0981433804003,2.27348548307801));
#37000=CARTESIAN_POINT('Ctrl Pts',(373.112769259521,-14.0986451181604,2.27921968479659));
#37001=CARTESIAN_POINT('Ctrl Pts',(373.098694521531,-14.099870566984,2.29321912389067));
#37002=CARTESIAN_POINT('Ctrl Pts',(373.090317713041,-14.1005924192794,2.30146046861299));
#37003=CARTESIAN_POINT('Ctrl Pts',(373.059684110036,-14.1032059374681,2.33127071471267));
#37004=CARTESIAN_POINT('Ctrl Pts',(373.037160773617,-14.1050775733042,2.35256484534791));
#37005=CARTESIAN_POINT('Ctrl Pts',(372.979787410027,-14.1097320666282,2.40526049532694));
#37006=CARTESIAN_POINT('Ctrl Pts',(372.94455168734,-14.1124889600739,2.43623300820811));
#37007=CARTESIAN_POINT('Ctrl Pts',(372.724322232064,-14.1291979847971,2.62145204803921));
#37008=CARTESIAN_POINT('Ctrl Pts',(372.523427225698,-14.1422930003608,2.75513263163544));
#37009=CARTESIAN_POINT('Ctrl Pts',(372.309820586046,-14.1558998485281,2.86513686373549));
#37010=CARTESIAN_POINT('Origin',(370.834317853224,2.31077344927308,0.));
#37011=CARTESIAN_POINT('',(372.309820655984,-15.6509557951682,2.86513682771809));
#37012=CARTESIAN_POINT('',(372.309820571668,-15.4046310424783,2.86513687113949));
#37013=CARTESIAN_POINT('',(372.309820613641,2.31077344927308,2.86513684952399));
#37014=CARTESIAN_POINT('Ctrl Pts',(372.309820655984,-15.6509557951682,2.8651368277181));
#37015=CARTESIAN_POINT('Ctrl Pts',(372.419480262493,-15.6437537932502,2.80866376325994));
#37016=CARTESIAN_POINT('Ctrl Pts',(372.525847643811,-15.6368020532833,2.74592082701906));
#37017=CARTESIAN_POINT('Ctrl Pts',(372.744053914637,-15.6220875706104,2.59969457905109));
#37018=CARTESIAN_POINT('Ctrl Pts',(372.854572862225,-15.614350038891,2.51477082310849));
#37019=CARTESIAN_POINT('Ctrl Pts',(373.027440542832,-15.6012859858726,2.36316664714977));
#37020=CARTESIAN_POINT('Ctrl Pts',(373.093071307726,-15.5960669541733,2.30051620411554));
#37021=CARTESIAN_POINT('Ctrl Pts',(373.197073026259,-15.5872595003788,2.19249122515072));
#37022=CARTESIAN_POINT('Ctrl Pts',(373.236988817073,-15.5837348427075,2.14867432550738));
#37023=CARTESIAN_POINT('Ctrl Pts',(373.289709410992,-15.5788621102471,2.08749425296974));
#37024=CARTESIAN_POINT('Ctrl Pts',(373.303582982364,-15.5775582010808,2.07106485791478));
#37025=CARTESIAN_POINT('Ctrl Pts',(373.326622540085,-15.5753553706888,2.04322029672452));
#37026=CARTESIAN_POINT('Ctrl Pts',(373.335877163479,-15.574460078054,2.03187913992358));
#37027=CARTESIAN_POINT('Ctrl Pts',(373.354006433012,-15.5726852242698,2.00935087147635));
#37028=CARTESIAN_POINT('Ctrl Pts',(373.362884629099,-15.5718058345628,1.99816703839138));
#37029=CARTESIAN_POINT('Ctrl Pts',(373.384280025972,-15.5696613691217,1.97084439100659));
#37030=CARTESIAN_POINT('Ctrl Pts',(373.396718571911,-15.5683932203344,1.95464503735853));
#37031=CARTESIAN_POINT('Ctrl Pts',(373.431624614934,-15.5647722144595,1.90827930400172));
#37032=CARTESIAN_POINT('Ctrl Pts',(373.453718541171,-15.5624050363577,1.8778370963787));
#37033=CARTESIAN_POINT('Ctrl Pts',(373.595803116957,-15.5466689259618,1.67467746921286));
#37034=CARTESIAN_POINT('Ctrl Pts',(373.699154175144,-15.5326791833423,1.49098326481295));
#37035=CARTESIAN_POINT('Ctrl Pts',(373.865428829333,-15.5048019344976,1.11330875122911));
#37036=CARTESIAN_POINT('Ctrl Pts',(373.92936052755,-15.4910015914261,0.920767265776321));
#37037=CARTESIAN_POINT('Ctrl Pts',(373.982050123253,-15.4758622826663,0.69205470833421));
#37038=CARTESIAN_POINT('Ctrl Pts',(373.988819887316,-15.4738018889293,0.660511366434027));
#37039=CARTESIAN_POINT('Ctrl Pts',(373.997443121209,-15.4710133500097,0.617169689688758));
#37040=CARTESIAN_POINT('Ctrl Pts',(373.999706128549,-15.4702639410783,0.605455996560258));
#37041=CARTESIAN_POINT('Ctrl Pts',(374.003402213955,-15.46900980477,0.585737145734349));
#37042=CARTESIAN_POINT('Ctrl Pts',(374.004870118756,-15.4685031460104,0.577738717446529));
#37043=CARTESIAN_POINT('Ctrl Pts',(374.007609840541,-15.4675409350271,0.562485354214488));
#37044=CARTESIAN_POINT('Ctrl Pts',(374.008887080997,-15.4670850675665,0.555231511283665));
#37045=CARTESIAN_POINT('Ctrl Pts',(374.011869374486,-15.466002801693,0.537947397897834));
#37046=CARTESIAN_POINT('Ctrl Pts',(374.013551832461,-15.4653776662136,0.527913236144369));
#37047=CARTESIAN_POINT('Ctrl Pts',(374.019359269913,-15.4631660700878,0.492242783413518));
#37048=CARTESIAN_POINT('Ctrl Pts',(374.023222035485,-15.461593568289,0.466564033176625));
#37049=CARTESIAN_POINT('Ctrl Pts',(374.054825391804,-15.4477302503329,0.237700450547395));
#37050=CARTESIAN_POINT('Ctrl Pts',(374.063427402746,-15.436331269634,0.0323181754851601));
#37051=CARTESIAN_POINT('Ctrl Pts',(374.04397147451,-15.4160080442741,-0.330625899390931));
#37052=CARTESIAN_POINT('Ctrl Pts',(374.02385455652,-15.4071418901333,-0.48789422927185));
#37053=CARTESIAN_POINT('Ctrl Pts',(373.975153476964,-15.3929977768492,-0.727064156446861));
#37054=CARTESIAN_POINT('Ctrl Pts',(373.95469809173,-15.3879466991154,-0.810367812538036));
#37055=CARTESIAN_POINT('Ctrl Pts',(373.924156535075,-15.3813144317105,-0.916305272060674));
#37056=CARTESIAN_POINT('Ctrl Pts',(373.917097800655,-15.3798314760725,-0.939779855343723));
#37057=CARTESIAN_POINT('Ctrl Pts',(373.905205178846,-15.3774098897247,-0.977753599119451));
#37058=CARTESIAN_POINT('Ctrl Pts',(373.900534650598,-15.3764766163456,-0.992303182575875));
#37059=CARTESIAN_POINT('Ctrl Pts',(373.891355505176,-15.3746755411495,-1.0202142929322));
#37060=CARTESIAN_POINT('Ctrl Pts',(373.886862308014,-15.3738082647416,-1.03358054860042));
#37061=CARTESIAN_POINT('Ctrl Pts',(373.876357839396,-15.3718127616344,-1.06416296155162));
#37062=CARTESIAN_POINT('Ctrl Pts',(373.87028791874,-15.3706826148698,-1.08135832432973));
#37063=CARTESIAN_POINT('Ctrl Pts',(373.850472831337,-15.3670641533708,-1.13600994017068));
#37064=CARTESIAN_POINT('Ctrl Pts',(373.83617830905,-15.3645576937593,-1.17326169737432));
#37065=CARTESIAN_POINT('Ctrl Pts',(373.725679012622,-15.3459035874339,-1.44597516383213));
#37066=CARTESIAN_POINT('Ctrl Pts',(373.602605639725,-15.3288135254764,-1.66953579757567));
#37067=CARTESIAN_POINT('Ctrl Pts',(373.380752189736,-15.3030358408299,-1.97936063482201));
#37068=CARTESIAN_POINT('Ctrl Pts',(373.300904160425,-15.2944731657276,-2.07801636328373));
#37069=CARTESIAN_POINT('Ctrl Pts',(373.188180531725,-15.2834834480622,-2.20160967827205));
#37070=CARTESIAN_POINT('Ctrl Pts',(373.160352957041,-15.2808501318521,-2.23098984393509));
#37071=CARTESIAN_POINT('Ctrl Pts',(373.112515222625,-15.2764662125022,-2.27962819584946));
#37072=CARTESIAN_POINT('Ctrl Pts',(373.092796609984,-15.2746983057297,-2.29916545533747));
#37073=CARTESIAN_POINT('Ctrl Pts',(373.064736959048,-15.2722400531265,-2.32625764825913));
#37074=CARTESIAN_POINT('Ctrl Pts',(373.056605654732,-15.2715343164733,-2.3340267714441));
#37075=CARTESIAN_POINT('Ctrl Pts',(373.042619629455,-15.270331991283,-2.34725048729455));
#37076=CARTESIAN_POINT('Ctrl Pts',(373.036784996689,-15.2698338143784,-2.35272609380507));
#37077=CARTESIAN_POINT('Ctrl Pts',(373.025424391811,-15.2688704885271,-2.36330833977107));
#37078=CARTESIAN_POINT('Ctrl Pts',(373.019900892674,-15.2684051391282,-2.36841739409777));
#37079=CARTESIAN_POINT('Ctrl Pts',(373.004803466878,-15.2671412232917,-2.38228422285441));
#37080=CARTESIAN_POINT('Ctrl Pts',(372.995194341379,-15.266345507034,-2.39100370842384));
#37081=CARTESIAN_POINT('Ctrl Pts',(372.958098806748,-15.2633058301426,-2.42425854155291));
#37082=CARTESIAN_POINT('Ctrl Pts',(372.930243927449,-15.2610904781993,-2.44838092792098));
#37083=CARTESIAN_POINT('Ctrl Pts',(372.734110165144,-15.2459007574512,-2.61243225085012));
#37084=CARTESIAN_POINT('Ctrl Pts',(372.552353899354,-15.2338455841046,-2.73539546495539));
#37085=CARTESIAN_POINT('Ctrl Pts',(372.237775341001,-15.213844292626,-2.9043972369454));
#37086=CARTESIAN_POINT('Ctrl Pts',(372.111959712414,-15.206049221562,-2.96189861757119));
#37087=CARTESIAN_POINT('Ctrl Pts',(371.909155490287,-15.193429998353,-3.03925361898433));
#37088=CARTESIAN_POINT('Ctrl Pts',(371.834459248779,-15.1887729294291,-3.06464585342348));
#37089=CARTESIAN_POINT('Ctrl Pts',(371.736079904299,-15.1825912126904,-3.09410904419484));
#37090=CARTESIAN_POINT('Ctrl Pts',(371.713174145387,-15.1811486648937,-3.10069301047388));
#37091=CARTESIAN_POINT('Ctrl Pts',(371.675608547669,-15.1787766694294,-3.1110410687437));
#37092=CARTESIAN_POINT('Ctrl Pts',(371.660991240289,-15.1778521682368,-3.11495708844222));
#37093=CARTESIAN_POINT('Ctrl Pts',(371.632648776992,-15.1760564139625,-3.12233657107358));
#37094=CARTESIAN_POINT('Ctrl Pts',(371.618927294203,-15.175185598627,-3.12581284498552));
#37095=CARTESIAN_POINT('Ctrl Pts',(371.587144307575,-15.1731650258625,-3.13364245786491));
#37096=CARTESIAN_POINT('Ctrl Pts',(371.569067309054,-15.1720131872693,-3.13793019968481));
#37097=CARTESIAN_POINT('Ctrl Pts',(371.51018106823,-15.1682520546185,-3.15136088623723));
#37098=CARTESIAN_POINT('Ctrl Pts',(371.469232069749,-15.1656225413159,-3.15986553422013));
#37099=CARTESIAN_POINT('Ctrl Pts',(371.232875652219,-15.1503581367911,-3.20417440198651));
#37100=CARTESIAN_POINT('Ctrl Pts',(371.03468581796,-15.1371796311015,-3.22264042956758));
#37101=CARTESIAN_POINT('Ctrl Pts',(370.668032052834,-15.1124392265908,-3.22284182234561));
#37102=CARTESIAN_POINT('Ctrl Pts',(370.500222374741,-15.100988250811,-3.20978877467439));
#37103=CARTESIAN_POINT('Ctrl Pts',(370.287485838501,-15.0867693371363,-3.17637019941516));
#37104=CARTESIAN_POINT('Ctrl Pts',(370.240943955677,-15.0836783706995,-3.16800580337536));
#37105=CARTESIAN_POINT('Ctrl Pts',(370.164050381591,-15.0786221906244,-3.1524325030785));
#37106=CARTESIAN_POINT('Ctrl Pts',(370.133590064929,-15.0766325640451,-3.14580194936312));
#37107=CARTESIAN_POINT('Ctrl Pts',(370.091764456354,-15.0739233845355,-3.13605972412198));
#37108=CARTESIAN_POINT('Ctrl Pts',(370.08031395383,-15.0731840689812,-3.13332639063653));
#37109=CARTESIAN_POINT('Ctrl Pts',(370.061010042763,-15.0719419940891,-3.12860643201375));
#37110=CARTESIAN_POINT('Ctrl Pts',(370.053148746188,-15.0714373833856,-3.12665284408184));
#37111=CARTESIAN_POINT('Ctrl Pts',(370.038122705319,-15.0704752964603,-3.12285855697789));
#37112=CARTESIAN_POINT('Ctrl Pts',(370.030956842656,-15.070017530024,-3.12102280826911));
#37113=CARTESIAN_POINT('Ctrl Pts',(370.013831546844,-15.0689259122627,-3.11657276595199));
#37114=CARTESIAN_POINT('Ctrl Pts',(370.003878125414,-15.0682933749425,-3.11393536374566));
#37115=CARTESIAN_POINT('Ctrl Pts',(369.968116878759,-15.0660271213258,-3.10427588552541));
#37116=CARTESIAN_POINT('Ctrl Pts',(369.942383265577,-15.0644082864606,-3.09698009331305));
#37117=CARTESIAN_POINT('Ctrl Pts',(369.740479012171,-15.0517798096493,-3.03701230371523));
#37118=CARTESIAN_POINT('Ctrl Pts',(369.568995670286,-15.0414805518083,-2.96966397531245));
#37119=CARTESIAN_POINT('Ctrl Pts',(369.249091931811,-15.021513446328,-2.81124977245585));
#37120=CARTESIAN_POINT('Ctrl Pts',(369.100450592914,-15.0118720703791,-2.72208855957599));
#37121=CARTESIAN_POINT('Ctrl Pts',(368.91105929198,-14.9984072896181,-2.5866520869862));
#37122=CARTESIAN_POINT('Ctrl Pts',(368.863404077777,-14.9949107079591,-2.55052755251698));
#37123=CARTESIAN_POINT('Ctrl Pts',(368.782874126573,-14.98878719572,-2.48587752626968));
#37124=CARTESIAN_POINT('Ctrl Pts',(368.749520877183,-14.9861838322952,-2.45797268836977));
#37125=CARTESIAN_POINT('Ctrl Pts',(368.702364835397,-14.9823991790438,-2.41686940475033));
#37126=CARTESIAN_POINT('Ctrl Pts',(368.688097903176,-14.9812400116569,-2.40420907818868));
#37127=CARTESIAN_POINT('Ctrl Pts',(368.663420734415,-14.9792097353485,-2.3819161177755));
#37128=CARTESIAN_POINT('Ctrl Pts',(368.652960042747,-14.9783410146094,-2.37233993877343));
#37129=CARTESIAN_POINT('Ctrl Pts',(368.631515767031,-14.9765431826628,-2.35244715030342));
#37130=CARTESIAN_POINT('Ctrl Pts',(368.620540668944,-14.9756137151383,-2.34212194216377));
#37131=CARTESIAN_POINT('Ctrl Pts',(368.592609027097,-14.9732238738964,-2.31547254237094));
#37132=CARTESIAN_POINT('Ctrl Pts',(368.575758404433,-14.9717587837716,-2.29903908724636));
#37133=CARTESIAN_POINT('Ctrl Pts',(368.510165120646,-14.9659617516298,-2.23365256711393));
#37134=CARTESIAN_POINT('Ctrl Pts',(368.462824626564,-14.9615693598081,-2.18332508364247));
#37135=CARTESIAN_POINT('Ctrl Pts',(368.198832778224,-14.9358162937266,-1.88395391810426));
#37136=CARTESIAN_POINT('Ctrl Pts',(368.019904299637,-14.9129295125544,-1.60439022650103));
#37137=CARTESIAN_POINT('Ctrl Pts',(367.867704232485,-14.8880773822789,-1.25995747772335));
#37138=CARTESIAN_POINT('Ctrl Pts',(367.849794628134,-14.8850320631716,-1.21692677633703));
#37139=CARTESIAN_POINT('Ctrl Pts',(367.821593902832,-14.8800422872204,-1.14479825725582));
#37140=CARTESIAN_POINT('Ctrl Pts',(367.810776409617,-14.8780741757684,-1.11591485013125));
#37141=CARTESIAN_POINT('Ctrl Pts',(367.796421163476,-14.8753891912276,-1.07584324722349));
#37142=CARTESIAN_POINT('Ctrl Pts',(367.792527745835,-14.8746530017986,-1.06478539750903));
#37143=CARTESIAN_POINT('Ctrl Pts',(367.786049393996,-14.8734146532972,-1.0460604287733));
#37144=CARTESIAN_POINT('Ctrl Pts',(367.783432857731,-14.8729106675423,-1.0384044344821));
#37145=CARTESIAN_POINT('Ctrl Pts',(367.778475947558,-14.8719485756502,-1.02372002141383));
#37146=CARTESIAN_POINT('Ctrl Pts',(367.776130945283,-14.871490187225,-1.01669330349784));
#37147=CARTESIAN_POINT('Ctrl Pts',(367.770571877757,-14.8703955382334,-0.999842487840838));
#37148=CARTESIAN_POINT('Ctrl Pts',(367.767380783738,-14.8697606082728,-0.990010818754165));
#37149=CARTESIAN_POINT('Ctrl Pts',(367.756014991185,-14.8674745043403,-0.954410746900676));
#37150=CARTESIAN_POINT('Ctrl Pts',(367.748117044674,-14.8658385628919,-0.928554286094378));
#37151=CARTESIAN_POINT('Ctrl Pts',(367.694385006868,-14.8543387201679,-0.744381217167028));
#37152=CARTESIAN_POINT('Ctrl Pts',(367.660424408554,-14.8450416444261,-0.582833759388019));
#37153=CARTESIAN_POINT('Ctrl Pts',(367.620828268992,-14.8279965498355,-0.281142552622508));
#37154=CARTESIAN_POINT('Ctrl Pts',(367.611675000397,-14.820248482665,-0.141874364625561));
#37155=CARTESIAN_POINT('Ctrl Pts',(367.61146598773,-14.804658615031,0.132486177532188));
#37156=CARTESIAN_POINT('Ctrl Pts',(367.619838339009,-14.7968431345822,0.267286335011411));
#37157=CARTESIAN_POINT('Ctrl Pts',(367.640201994004,-14.7870406000304,0.429608870738332));
#37158=CARTESIAN_POINT('Ctrl Pts',(367.644151057036,-14.7853109856536,0.458012703061152));
#37159=CARTESIAN_POINT('Ctrl Pts',(367.650947421777,-14.7825759298296,0.502531482584673));
#37160=CARTESIAN_POINT('Ctrl Pts',(367.653539369659,-14.7815785546884,0.518684314282673));
#37161=CARTESIAN_POINT('Ctrl Pts',(367.658335537501,-14.7798096189369,0.547184795146043));
#37162=CARTESIAN_POINT('Ctrl Pts',(367.660489084109,-14.7790396811135,0.559540710868483));
#37163=CARTESIAN_POINT('Ctrl Pts',(367.665599739343,-14.7772663855529,0.587883839175676));
#37164=CARTESIAN_POINT('Ctrl Pts',(367.668605794752,-14.7762614891453,0.603861773061856));
#37165=CARTESIAN_POINT('Ctrl Pts',(367.677310623361,-14.7734531319098,0.648277794445586));
#37166=CARTESIAN_POINT('Ctrl Pts',(367.683272475573,-14.7716413476168,0.676662166689679));
#37167=CARTESIAN_POINT('Ctrl Pts',(367.724321222029,-14.7598393553334,0.85977295159897));
#37168=CARTESIAN_POINT('Ctrl Pts',(367.77040500797,-14.7494966607915,1.01178731832911));
#37169=CARTESIAN_POINT('Ctrl Pts',(367.91446306147,-14.7227872473142,1.3852728399237));
#37170=CARTESIAN_POINT('Ctrl Pts',(368.026526912386,-14.7061464893408,1.60026214889701));
#37171=CARTESIAN_POINT('Ctrl Pts',(368.194058917271,-14.6864626421441,1.8489272177312));
#37172=CARTESIAN_POINT('Ctrl Pts',(368.227852344572,-14.6826973002642,1.89626939476469));
#37173=CARTESIAN_POINT('Ctrl Pts',(368.272166239886,-14.6780347556983,1.95492517038413));
#37174=CARTESIAN_POINT('Ctrl Pts',(368.281509354715,-14.6770663338005,1.96711008926563));
#37175=CARTESIAN_POINT('Ctrl Pts',(368.296392936976,-14.675547125083,1.98623602188887));
#37176=CARTESIAN_POINT('Ctrl Pts',(368.301875481864,-14.6749924376846,1.99322152691901));
#37177=CARTESIAN_POINT('Ctrl Pts',(368.312288307713,-14.6739483497035,2.0063765600934));
#37178=CARTESIAN_POINT('Ctrl Pts',(368.317212346674,-14.6734585566383,2.01255057064139));
#37179=CARTESIAN_POINT('Ctrl Pts',(368.328788742094,-14.6723161165162,2.02695669682146));
#37180=CARTESIAN_POINT('Ctrl Pts',(368.335459011149,-14.6716647576191,2.03517421176685));
#37181=CARTESIAN_POINT('Ctrl Pts',(368.357295241436,-14.6695542213975,2.06180640113035));
#37182=CARTESIAN_POINT('Ctrl Pts',(368.372625605345,-14.668106318037,2.08008605786806));
#37183=CARTESIAN_POINT('Ctrl Pts',(368.456761783862,-14.6603301514437,2.17817541405429));
#37184=CARTESIAN_POINT('Ctrl Pts',(368.529253925528,-14.654234353839,2.25475179065898));
#37185=CARTESIAN_POINT('Ctrl Pts',(368.780858471539,-14.6344294578026,2.49568726017511));
#37186=CARTESIAN_POINT('Ctrl Pts',(368.974779197389,-14.62117631311,2.64334470517025));
#37187=CARTESIAN_POINT('Ctrl Pts',(369.269662967429,-14.6014205130628,2.81922828196928));
#37188=CARTESIAN_POINT('Ctrl Pts',(369.358217772903,-14.5955419526884,2.86658659373234));
#37189=CARTESIAN_POINT('Ctrl Pts',(369.473027051763,-14.5879082740031,2.92125367503386));
#37190=CARTESIAN_POINT('Ctrl Pts',(369.497364152839,-14.5862895928417,2.93247172488076));
#37191=CARTESIAN_POINT('Ctrl Pts',(369.536250510381,-14.5837011358999,2.94981147975506));
#37192=CARTESIAN_POINT('Ctrl Pts',(369.550710049389,-14.582738190549,2.9561322001436));
#37193=CARTESIAN_POINT('Ctrl Pts',(369.576785568937,-14.5810006088074,2.96730324701622));
#37194=CARTESIAN_POINT('Ctrl Pts',(369.588384718044,-14.5802273082243,2.97219222482454));
#37195=CARTESIAN_POINT('Ctrl Pts',(369.615656826155,-14.5784080911209,2.98349957203311));
#37196=CARTESIAN_POINT('Ctrl Pts',(369.631352214069,-14.5773603258432,2.98986254679237));
#37197=CARTESIAN_POINT('Ctrl Pts',(369.677053059222,-14.5743068596351,3.00797174884617));
#37198=CARTESIAN_POINT('Ctrl Pts',(369.707184755305,-14.5722903196723,3.01939177712752));
#37199=CARTESIAN_POINT('Ctrl Pts',(369.931522667188,-14.5572476653161,3.1005907432903));
#37200=CARTESIAN_POINT('Ctrl Pts',(370.13182645524,-14.543610081372,3.15201218383113));
#37201=CARTESIAN_POINT('Ctrl Pts',(370.564734213961,-14.5140699315101,3.21981609019599));
#37202=CARTESIAN_POINT('Ctrl Pts',(370.797047834559,-14.4981788607032,3.23086916491071));
#37203=CARTESIAN_POINT('Ctrl Pts',(371.052768884613,-14.4817639507858,3.21542929740228));
#37204=CARTESIAN_POINT('Ctrl Pts',(371.076974714773,-14.4802214603532,3.21369322571111));
#37205=CARTESIAN_POINT('Ctrl Pts',(371.110886678961,-14.4780784505727,3.2108756623871));
#37206=CARTESIAN_POINT('Ctrl Pts',(371.120610336352,-14.4774660585031,3.21002327944402));
#37207=CARTESIAN_POINT('Ctrl Pts',(371.138281787113,-14.4763570811278,3.20839325152281));
#37208=CARTESIAN_POINT('Ctrl Pts',(371.146230846521,-14.4758596962908,3.20763021858007));
#37209=CARTESIAN_POINT('Ctrl Pts',(371.162579548382,-14.4748398467784,3.20599955155334));
#37210=CARTESIAN_POINT('Ctrl Pts',(371.170978727587,-14.4743175779978,3.20512844120082));
#37211=CARTESIAN_POINT('Ctrl Pts',(371.192681651692,-14.4729721934408,3.20279129577709));
#37212=CARTESIAN_POINT('Ctrl Pts',(371.205980016667,-14.4721518242902,3.20127536258272));
#37213=CARTESIAN_POINT('Ctrl Pts',(371.262848154292,-14.468659351576,3.19443359472653));
#37214=CARTESIAN_POINT('Ctrl Pts',(371.306318290806,-14.4660291521273,3.18830052353345));
#37215=CARTESIAN_POINT('Ctrl Pts',(371.425177468573,-14.4589127948247,3.16904658591004));
#37216=CARTESIAN_POINT('Ctrl Pts',(371.500248395448,-14.4545015619683,3.15412576860375));
#37217=CARTESIAN_POINT('Ctrl Pts',(371.802124908353,-14.436852394796,3.08286570568824));
#37218=CARTESIAN_POINT('Ctrl Pts',(372.02301539167,-14.4240935452109,3.00461561056256));
#37219=CARTESIAN_POINT('Ctrl Pts',(372.259116579889,-14.4090751790053,2.89082587148885));
#37220=CARTESIAN_POINT('Ctrl Pts',(372.28455597185,-14.4074387292058,2.87814776360241));
#37221=CARTESIAN_POINT('Ctrl Pts',(372.309820634558,-14.4057934188676,2.86513683875233));
#37222=CARTESIAN_POINT('',(367.611568484837,-14.5621367793278,0.00201768782053767));
#37223=CARTESIAN_POINT('Ctrl Pts',(372.309820586045,-14.1558998485281,2.86513686373551));
#37224=CARTESIAN_POINT('Ctrl Pts',(372.223986561129,-14.1613675181967,2.90934010579923));
#37225=CARTESIAN_POINT('Ctrl Pts',(372.136099635432,-14.1669097736879,2.94972063990983));
#37226=CARTESIAN_POINT('Ctrl Pts',(371.988269349969,-14.1762564371237,3.0097259781714));
#37227=CARTESIAN_POINT('Ctrl Pts',(371.929457461496,-14.1799804756913,3.03162052081622));
#37228=CARTESIAN_POINT('Ctrl Pts',(371.848563681688,-14.1851283612968,3.05907463848042));
#37229=CARTESIAN_POINT('Ctrl Pts',(371.827004648204,-14.1865027145504,3.06613847225981));
#37230=CARTESIAN_POINT('Ctrl Pts',(371.792591562831,-14.1887010291996,3.07701295819168));
#37231=CARTESIAN_POINT('Ctrl Pts',(371.77978495866,-14.1895201083055,3.08097211792375));
#37232=CARTESIAN_POINT('Ctrl Pts',(371.753440591567,-14.1912072316123,3.08893675282229));
#37233=CARTESIAN_POINT('Ctrl Pts',(371.739900480351,-14.1920755432671,3.09293339185411));
#37234=CARTESIAN_POINT('Ctrl Pts',(371.708458733053,-14.1940948111414,3.10198990130513));
#37235=CARTESIAN_POINT('Ctrl Pts',(371.690538811805,-14.19524787698,3.10698395110427));
#37236=CARTESIAN_POINT('Ctrl Pts',(371.633200270867,-14.1989448871394,3.12242974014236));
#37237=CARTESIAN_POINT('Ctrl Pts',(371.593627335898,-14.20150780166,3.13228821534759));
#37238=CARTESIAN_POINT('Ctrl Pts',(371.500278255754,-14.2075825748627,3.15367058063603));
#37239=CARTESIAN_POINT('Ctrl Pts',(371.446374388373,-14.2111129467584,3.16457384372551));
#37240=CARTESIAN_POINT('Ctrl Pts',(371.244871072057,-14.2243937593663,3.19999159751943));
#37241=CARTESIAN_POINT('Ctrl Pts',(371.095912009801,-14.2343882016061,3.21559640364351));
#37242=CARTESIAN_POINT('Ctrl Pts',(370.728312221536,-14.2592198316396,3.22839125848892));
#37243=CARTESIAN_POINT('Ctrl Pts',(370.509980669571,-14.2741318438301,3.213808701539));
#37244=CARTESIAN_POINT('Ctrl Pts',(370.269786349402,-14.2897610465618,3.17302140301347));
#37245=CARTESIAN_POINT('Ctrl Pts',(370.244835285122,-14.2913745081963,3.168480872173));
#37246=CARTESIAN_POINT('Ctrl Pts',(370.210089462614,-14.293604826614,3.16173325281457));
#37247=CARTESIAN_POINT('Ctrl Pts',(370.200248220215,-14.2942346736358,3.15977435149492));
#37248=CARTESIAN_POINT('Ctrl Pts',(370.183230598161,-14.2953204059993,3.15630428310791));
#37249=CARTESIAN_POINT('Ctrl Pts',(370.176049997681,-14.2957774789257,3.15481453879244));
#37250=CARTESIAN_POINT('Ctrl Pts',(370.160870548104,-14.2967413894517,3.15161120782683));
#37251=CARTESIAN_POINT('Ctrl Pts',(370.152873018193,-14.2972478703358,3.14989165171628));
#37252=CARTESIAN_POINT('Ctrl Pts',(370.133018409303,-14.2985020423274,3.14554353782786));
#37253=CARTESIAN_POINT('Ctrl Pts',(370.121169339341,-14.2992476692183,3.14287834102476));
#37254=CARTESIAN_POINT('Ctrl Pts',(370.076453826311,-14.3020516640907,3.13255462980272));
#37255=CARTESIAN_POINT('Ctrl Pts',(370.043692030089,-14.3040859848517,3.1244467358504));
#37256=CARTESIAN_POINT('Ctrl Pts',(369.792393436752,-14.3195773498738,3.05804924326558));
#37257=CARTESIAN_POINT('Ctrl Pts',(369.580386001519,-14.332018490769,2.97740705792136));
#37258=CARTESIAN_POINT('Ctrl Pts',(369.198082779311,-14.3560257450671,2.78384097563209));
#37259=CARTESIAN_POINT('Ctrl Pts',(369.026641659745,-14.3674964530608,2.67569200545997));
#37260=CARTESIAN_POINT('Ctrl Pts',(368.844689098034,-14.3812464190204,2.53539974943799));
#37261=CARTESIAN_POINT('Ctrl Pts',(368.82311799837,-14.3829032746543,2.51832276451449));
#37262=CARTESIAN_POINT('Ctrl Pts',(368.788146039231,-14.3856352015933,2.48990092508703));
#37263=CARTESIAN_POINT('Ctrl Pts',(368.774614308145,-14.3867037578458,2.47871882160117));
#37264=CARTESIAN_POINT('Ctrl Pts',(368.75046320298,-14.3886320367758,2.45842695572304));
#37265=CARTESIAN_POINT('Ctrl Pts',(368.739810450985,-14.3894901023403,2.44935747333377));
#37266=CARTESIAN_POINT('Ctrl Pts',(368.717711302272,-14.3912861304441,2.43029322893714));
#37267=CARTESIAN_POINT('Ctrl Pts',(368.706275888992,-14.3922245842296,2.42028631694347));
#37268=CARTESIAN_POINT('Ctrl Pts',(368.675843627777,-14.3947467544945,2.39327321060066));
#37269=CARTESIAN_POINT('Ctrl Pts',(368.656977417908,-14.39633652132,2.37612209518331));
#37270=CARTESIAN_POINT('Ctrl Pts',(368.615734598434,-14.3998710875583,2.33772494081934));
#37271=CARTESIAN_POINT('Ctrl Pts',(368.59345582189,-14.4018200967631,2.31637795023291));
#37272=CARTESIAN_POINT('Ctrl Pts',(368.52697459957,-14.4077588625314,2.25082047322648));
#37273=CARTESIAN_POINT('Ctrl Pts',(368.483750797434,-14.4117893125636,2.2056426227508));
#37274=CARTESIAN_POINT('Ctrl Pts',(368.33858245214,-14.425927373716,2.04479535131051));
#37275=CARTESIAN_POINT('Ctrl Pts',(368.243648890569,-14.4362747606188,1.92309884255712));
#37276=CARTESIAN_POINT('Ctrl Pts',(368.047198427823,-14.4601204493167,1.63018635058073));
#37277=CARTESIAN_POINT('Ctrl Pts',(367.952068702746,-14.4736262941071,1.45540205072955));
#37278=CARTESIAN_POINT('Ctrl Pts',(367.863255122363,-14.4880636653893,1.24883681004773));
#37279=CARTESIAN_POINT('Ctrl Pts',(367.853177638638,-14.4897355994879,1.22458574715773));
#37280=CARTESIAN_POINT('Ctrl Pts',(367.839588517502,-14.4920357522168,1.19072178319475));
#37281=CARTESIAN_POINT('Ctrl Pts',(367.835824836624,-14.4926779380862,1.18121200266286));
#37282=CARTESIAN_POINT('Ctrl Pts',(367.82942236771,-14.4937791112338,1.16480693090007));
#37283=CARTESIAN_POINT('Ctrl Pts',(367.826761912075,-14.4942393647444,1.15792026003089));
#37284=CARTESIAN_POINT('Ctrl Pts',(367.8212227985,-14.4952032008594,1.14343420822557));
#37285=CARTESIAN_POINT('Ctrl Pts',(367.818349182529,-14.4957064646365,1.13583298806097));
#37286=CARTESIAN_POINT('Ctrl Pts',(367.811345283805,-14.496941314451,1.1170924524523));
#37287=CARTESIAN_POINT('Ctrl Pts',(367.807247736193,-14.4976709748604,1.10594087528126));
#37288=CARTESIAN_POINT('Ctrl Pts',(367.792383530459,-14.5003457860907,1.0647860034953));
#37289=CARTESIAN_POINT('Ctrl Pts',(367.782000123076,-14.5022696567905,1.03464501456254));
#37290=CARTESIAN_POINT('Ctrl Pts',(367.756879105932,-14.5070819782502,0.958051574230242));
#37291=CARTESIAN_POINT('Ctrl Pts',(367.742744331952,-14.5099421570616,0.911408638277277));
#37292=CARTESIAN_POINT('Ctrl Pts',(367.651482169859,-14.5296669372514,0.583647475138517));
#37293=CARTESIAN_POINT('Ctrl Pts',(367.611750993081,-14.5453464830234,0.293528753126043));
#37294=CARTESIAN_POINT('Ctrl Pts',(367.611568484837,-14.5621367793278,0.00201768782053767));
#37295=CARTESIAN_POINT('Ctrl Pts',(367.611568482398,-14.5621370039932,0.00201378720837838));
#37296=CARTESIAN_POINT('Ctrl Pts',(367.611529543686,-14.5657262072406,-0.0603014899340788));
#37297=CARTESIAN_POINT('Ctrl Pts',(367.613298001685,-14.5693556441044,-0.122602711417325));
#37298=CARTESIAN_POINT('Ctrl Pts',(367.619123992365,-14.5753575806756,-0.224029177529986));
#37299=CARTESIAN_POINT('Ctrl Pts',(367.622093417936,-14.5776982320454,-0.263200716430373));
#37300=CARTESIAN_POINT('Ctrl Pts',(367.627485851368,-14.5811558607185,-0.32043338973456));
#37301=CARTESIAN_POINT('Ctrl Pts',(367.629347258197,-14.5822555702037,-0.338544693856912));
#37302=CARTESIAN_POINT('Ctrl Pts',(367.632894712695,-14.5842002783055,-0.370404195808923));
#37303=CARTESIAN_POINT('Ctrl Pts',(367.634516128718,-14.5850432468155,-0.384159221583366));
#37304=CARTESIAN_POINT('Ctrl Pts',(367.637873932442,-14.5867039800211,-0.411147102473858));
#37305=CARTESIAN_POINT('Ctrl Pts',(367.639603956755,-14.587521529145,-0.424380477676149));
#37306=CARTESIAN_POINT('Ctrl Pts',(367.643209043072,-14.5891531316318,-0.450684451132964));
#37307=CARTESIAN_POINT('Ctrl Pts',(367.645082337404,-14.5899671142311,-0.463755031332736));
#37308=CARTESIAN_POINT('Ctrl Pts',(367.649713767579,-14.5919029387403,-0.494714036293463));
#37309=CARTESIAN_POINT('Ctrl Pts',(367.652542361493,-14.5930269887199,-0.512591317510589));
#37310=CARTESIAN_POINT('Ctrl Pts',(367.663120110933,-14.5970352283152,-0.575980746669439));
#37311=CARTESIAN_POINT('Ctrl Pts',(367.671696156822,-14.5999453753308,-0.621347400769385));
#37312=CARTESIAN_POINT('Ctrl Pts',(367.700889455498,-14.6089359498101,-0.759452330405161));
#37313=CARTESIAN_POINT('Ctrl Pts',(367.724633449776,-14.6151108731505,-0.851470184924121));
#37314=CARTESIAN_POINT('Ctrl Pts',(367.82339296904,-14.6374219417203,-1.17447643183663));
#37315=CARTESIAN_POINT('Ctrl Pts',(367.920381600721,-14.6541041518821,-1.39786380971215));
#37316=CARTESIAN_POINT('Ctrl Pts',(368.086491169778,-14.6762588318194,-1.68632334492067));
#37317=CARTESIAN_POINT('Ctrl Pts',(368.134719837601,-14.6821651427856,-1.76250150926248));
#37318=CARTESIAN_POINT('Ctrl Pts',(368.195595639249,-14.6889519677809,-1.85028140904557));
#37319=CARTESIAN_POINT('Ctrl Pts',(368.205215171511,-14.6900062229206,-1.86392471200062));
#37320=CARTESIAN_POINT('Ctrl Pts',(368.220285921368,-14.6916292470805,-1.8849506124113));
#37321=CARTESIAN_POINT('Ctrl Pts',(368.225663229509,-14.6922028227161,-1.89238548162658));
#37322=CARTESIAN_POINT('Ctrl Pts',(368.235700035469,-14.6932630573907,-1.90613866954504));
#37323=CARTESIAN_POINT('Ctrl Pts',(368.240350842862,-14.6937502669214,-1.91246289932247));
#37324=CARTESIAN_POINT('Ctrl Pts',(368.251049560078,-14.6948618280029,-1.92690033023722));
#37325=CARTESIAN_POINT('Ctrl Pts',(368.257112603532,-14.695485119697,-1.93500208383904));
#37326=CARTESIAN_POINT('Ctrl Pts',(368.273149413321,-14.6971167843962,-1.9562222121564));
#37327=CARTESIAN_POINT('Ctrl Pts',(368.283185953523,-14.6981209597262,-1.9692930653197));
#37328=CARTESIAN_POINT('Ctrl Pts',(368.360801338117,-14.7057626398311,-2.06878439063798));
#37329=CARTESIAN_POINT('Ctrl Pts',(368.432660357244,-14.7121285853512,-2.15178977397477));
#37330=CARTESIAN_POINT('Ctrl Pts',(368.648473988236,-14.7298793679245,-2.37676628524619));
#37331=CARTESIAN_POINT('Ctrl Pts',(368.801727361925,-14.7409658535802,-2.50908590259739));
#37332=CARTESIAN_POINT('Ctrl Pts',(369.043461084339,-14.7577911171689,-2.68102602330532));
#37333=CARTESIAN_POINT('Ctrl Pts',(369.122929835695,-14.7632252055085,-2.73243803474336));
#37334=CARTESIAN_POINT('Ctrl Pts',(369.239935230264,-14.7711831019791,-2.80102567857583));
#37335=CARTESIAN_POINT('Ctrl Pts',(369.275721381436,-14.7736112476814,-2.82109511080739));
#37336=CARTESIAN_POINT('Ctrl Pts',(369.340241994816,-14.7779857525509,-2.85567687128589));
#37337=CARTESIAN_POINT('Ctrl Pts',(369.368829465222,-14.7799228371907,-2.87045235737246));
#37338=CARTESIAN_POINT('Ctrl Pts',(369.412702618209,-14.7828962044104,-2.89230204465149));
#37339=CARTESIAN_POINT('Ctrl Pts',(369.42783094632,-14.7839215683452,-2.89968887260062));
#37340=CARTESIAN_POINT('Ctrl Pts',(369.44313006262,-14.7849587739765,-2.90701119875706));
#37341=CARTESIAN_POINT('Ctrl Pts',(369.443243891176,-14.7849664910133,-2.90706567014499));
#37342=CARTESIAN_POINT('Ctrl Pts',(369.44347956101,-14.784982468342,-2.90717843030899));
#37343=CARTESIAN_POINT('Ctrl Pts',(369.443601403232,-14.7849907287,-2.90723671834003));
#37344=CARTESIAN_POINT('Ctrl Pts',(369.44385368473,-14.785007832293,-2.90735738765271));
#37345=CARTESIAN_POINT('Ctrl Pts',(369.443984124403,-14.7850166755574,-2.90741976775063));
#37346=CARTESIAN_POINT('Ctrl Pts',(369.444254229332,-14.7850349875826,-2.90754891755886));
#37347=CARTESIAN_POINT('Ctrl Pts',(369.444393895036,-14.7850444563766,-2.90761568590466));
#37348=CARTESIAN_POINT('Ctrl Pts',(369.444683127018,-14.7850640652319,-2.9077539300466));
#37349=CARTESIAN_POINT('Ctrl Pts',(369.444832694614,-14.7850742053858,-2.90782540465923));
#37350=CARTESIAN_POINT('Ctrl Pts',(369.445142461662,-14.7850952065497,-2.90797340522548));
#37351=CARTESIAN_POINT('Ctrl Pts',(369.445302661015,-14.7851060675567,-2.90804992904742));
#37352=CARTESIAN_POINT('Ctrl Pts',(369.445634474543,-14.7851285635215,-2.90820839563492));
#37353=CARTESIAN_POINT('Ctrl Pts',(369.445806090231,-14.7851401985863,-2.90829033672642));
#37354=CARTESIAN_POINT('Ctrl Pts',(369.446161583289,-14.7851643000955,-2.9084600348383));
#37355=CARTESIAN_POINT('Ctrl Pts',(369.446345461694,-14.7851767666152,-2.90854778959569));
#37356=CARTESIAN_POINT('Ctrl Pts',(369.446726392235,-14.7852025928852,-2.90872954183718));
#37357=CARTESIAN_POINT('Ctrl Pts',(369.446923445436,-14.7852159527137,-2.90882353665617));
#37358=CARTESIAN_POINT('Ctrl Pts',(369.447331708293,-14.785243632247,-2.90901822803156));
#37359=CARTESIAN_POINT('Ctrl Pts',(369.447542919348,-14.7852579520536,-2.90911892160163));
#37360=CARTESIAN_POINT('Ctrl Pts',(369.447980556,-14.7852876233021,-2.90932750369134));
#37361=CARTESIAN_POINT('Ctrl Pts',(369.448206983806,-14.7853029749017,-2.90943538905564));
#37362=CARTESIAN_POINT('Ctrl Pts',(369.448676195715,-14.7853347871718,-2.9096588858121));
#37363=CARTESIAN_POINT('Ctrl Pts',(369.448918981691,-14.7853512479786,-2.90977449324957));
#37364=CARTESIAN_POINT('Ctrl Pts',(369.449422140198,-14.785385362104,-2.91001400506745));
#37365=CARTESIAN_POINT('Ctrl Pts',(369.449682514275,-14.7854030155383,-2.91013790459845));
#37366=CARTESIAN_POINT('Ctrl Pts',(369.450222172062,-14.7854396046585,-2.9103946130254));
#37367=CARTESIAN_POINT('Ctrl Pts',(369.450501458114,-14.7854585405159,-2.91052741659699));
#37368=CARTESIAN_POINT('Ctrl Pts',(369.45095012229,-14.7854889605257,-2.91074068214148));
#37369=CARTESIAN_POINT('Ctrl Pts',(369.451119488603,-14.785500443816,-2.91082116966564));
#37370=CARTESIAN_POINT('Ctrl Pts',(369.451525152882,-14.7855279485492,-2.91101390907347));
#37371=CARTESIAN_POINT('Ctrl Pts',(369.45176145728,-14.7855439704622,-2.91112614686676));
#37372=CARTESIAN_POINT('Ctrl Pts',(369.464636110533,-14.7864169016701,-2.9172393157375));
#37373=CARTESIAN_POINT('Ctrl Pts',(369.477313227918,-14.7872766423694,-2.92315783676663));
#37374=CARTESIAN_POINT('Ctrl Pts',(369.505982921319,-14.7892216200159,-2.93631606601768));
#37375=CARTESIAN_POINT('Ctrl Pts',(369.521996822386,-14.7903084690579,-2.94350797915841));
#37376=CARTESIAN_POINT('Ctrl Pts',(369.563258768175,-14.7931103964096,-2.9616352558956));
#37377=CARTESIAN_POINT('Ctrl Pts',(369.588589140412,-14.7948319315181,-2.97237859050976));
#37378=CARTESIAN_POINT('Ctrl Pts',(369.801060619626,-14.8092875278524,-3.05930086161237));
#37379=CARTESIAN_POINT('Ctrl Pts',(369.994815099907,-14.8226115143557,-3.11803650085941));
#37380=CARTESIAN_POINT('Ctrl Pts',(370.414642241851,-14.8514628291443,-3.20331911012692));
#37381=CARTESIAN_POINT('Ctrl Pts',(370.640664368604,-14.8669854764521,-3.22488589164837));
#37382=CARTESIAN_POINT('Ctrl Pts',(370.900846086614,-14.8837891595983,-3.22224009950534));
#37383=CARTESIAN_POINT('Ctrl Pts',(370.934597928943,-14.8859473316224,-3.22136638429714));
#37384=CARTESIAN_POINT('Ctrl Pts',(370.980467394636,-14.8888453255572,-3.21945731660136));
#37385=CARTESIAN_POINT('Ctrl Pts',(370.992600743006,-14.8896085645721,-3.21888360145778));
#37386=CARTESIAN_POINT('Ctrl Pts',(371.01289985147,-14.8908795556085,-3.2178087191754));
#37387=CARTESIAN_POINT('Ctrl Pts',(371.021067375818,-14.8913893478805,-3.21734503954768));
#37388=CARTESIAN_POINT('Ctrl Pts',(371.036552848112,-14.8923527529241,-3.21640674411154));
#37389=CARTESIAN_POINT('Ctrl Pts',(371.043871065989,-14.8928067129957,-3.2159382441647));
#37390=CARTESIAN_POINT('Ctrl Pts',(371.061197822731,-14.8938784976677,-3.21476961852181));
#37391=CARTESIAN_POINT('Ctrl Pts',(371.071204885147,-14.8944951189018,-3.21404772227204));
#37392=CARTESIAN_POINT('Ctrl Pts',(371.106493513815,-14.8966616417776,-3.21133633790211));
#37393=CARTESIAN_POINT('Ctrl Pts',(371.131755542328,-14.8981982525318,-3.20909513368419));
#37394=CARTESIAN_POINT('Ctrl Pts',(371.374156337586,-14.9128273865256,-3.18470265991466));
#37395=CARTESIAN_POINT('Ctrl Pts',(371.588572828108,-14.9249031331154,-3.14084106498018));
#37396=CARTESIAN_POINT('Ctrl Pts',(371.93967960176,-14.9454832122059,-3.0309513879916));
#37397=CARTESIAN_POINT('Ctrl Pts',(372.079137539878,-14.9538846835172,-2.97639217264208));
#37398=CARTESIAN_POINT('Ctrl Pts',(372.263982497451,-14.9657538279371,-2.88880594163498));
#37399=CARTESIAN_POINT('Ctrl Pts',(372.313057550088,-14.968978471874,-2.86399531935684));
#37400=CARTESIAN_POINT('Ctrl Pts',(372.397380354294,-14.9746666327631,-2.81861951332702));
#37401=CARTESIAN_POINT('Ctrl Pts',(372.432917359687,-14.9771110002828,-2.79861746871052));
#37402=CARTESIAN_POINT('Ctrl Pts',(372.484098876848,-14.980705486509,-2.76851696381506));
#37403=CARTESIAN_POINT('Ctrl Pts',(372.500051401872,-14.9818365219561,-2.7589482284486));
#37404=CARTESIAN_POINT('Ctrl Pts',(372.527963276131,-14.983834799941,-2.74187564456478));
#37405=CARTESIAN_POINT('Ctrl Pts',(372.539957925444,-14.9846998862187,-2.73443025195699));
#37406=CARTESIAN_POINT('Ctrl Pts',(372.563245523905,-14.9863920802445,-2.7197621884444));
#37407=CARTESIAN_POINT('Ctrl Pts',(372.574543104809,-14.9872188844856,-2.71254738524966));
#37408=CARTESIAN_POINT('Ctrl Pts',(372.604839728448,-14.9894521568887,-2.69293233776965));
#37409=CARTESIAN_POINT('Ctrl Pts',(372.623753109014,-14.9908634673373,-2.68040178136115));
#37410=CARTESIAN_POINT('Ctrl Pts',(372.694476070924,-14.9962067746047,-2.63246401506292));
#37411=CARTESIAN_POINT('Ctrl Pts',(372.74537731758,-15.0001878644663,-2.59574772045186));
#37412=CARTESIAN_POINT('Ctrl Pts',(373.063186167333,-15.0259400767039,-2.35208812934773));
#37413=CARTESIAN_POINT('Ctrl Pts',(373.297165870306,-15.049362723905,-2.10581814719845));
#37414=CARTESIAN_POINT('Ctrl Pts',(373.515235068,-15.07474446331,-1.78913401456201));
#37415=CARTESIAN_POINT('Ctrl Pts',(373.540991783389,-15.0778102481464,-1.74992408904023));
#37416=CARTESIAN_POINT('Ctrl Pts',(373.582330977327,-15.0828301131175,-1.68389488407781));
#37417=CARTESIAN_POINT('Ctrl Pts',(373.598398297926,-15.0848081787999,-1.65738878096312));
#37418=CARTESIAN_POINT('Ctrl Pts',(373.620027139034,-15.0875046943282,-1.62051825677079));
#37419=CARTESIAN_POINT('Ctrl Pts',(373.62591750103,-15.0882426627077,-1.61034998121272));
#37420=CARTESIAN_POINT('Ctrl Pts',(373.63577420305,-15.0894833990594,-1.59311816853934));
#37421=CARTESIAN_POINT('Ctrl Pts',(373.639769734243,-15.0899880060545,-1.58607153914489));
#37422=CARTESIAN_POINT('Ctrl Pts',(373.647368963763,-15.0909508281979,-1.5725507652667));
#37423=CARTESIAN_POINT('Ctrl Pts',(373.650976949577,-15.0914093290709,-1.56607917979689));
#37424=CARTESIAN_POINT('Ctrl Pts',(373.65956142729,-15.0925036783252,-1.55055570969226));
#37425=CARTESIAN_POINT('Ctrl Pts',(373.664516817666,-15.0931382002379,-1.54149216348104));
#37426=CARTESIAN_POINT('Ctrl Pts',(373.682241520336,-15.0954185894691,-1.50869959115124));
#37427=CARTESIAN_POINT('Ctrl Pts',(373.694757081233,-15.097049334235,-1.48483372825997));
#37428=CARTESIAN_POINT('Ctrl Pts',(373.782882984625,-15.108703943065,-1.31153618912381));
#37429=CARTESIAN_POINT('Ctrl Pts',(373.847052218332,-15.1181416774105,-1.156550391605));
#37430=CARTESIAN_POINT('Ctrl Pts',(373.94723804733,-15.136273113025,-0.848681079501607));
#37431=CARTESIAN_POINT('Ctrl Pts',(373.984718395765,-15.1449528553108,-0.696782618238089));
#37432=CARTESIAN_POINT('Ctrl Pts',(374.031087543922,-15.1606901858902,-0.425394552490045));
#37433=CARTESIAN_POINT('Ctrl Pts',(374.044619760704,-15.167627509278,-0.307008298993963));
#37434=CARTESIAN_POINT('Ctrl Pts',(374.053152217895,-15.1763988089038,-0.161110782556596));
#37435=CARTESIAN_POINT('Ctrl Pts',(374.054392668747,-15.1780347503003,-0.134050236484528));
#37436=CARTESIAN_POINT('Ctrl Pts',(374.055818003606,-15.1806448840402,-0.0911351358949342));
#37437=CARTESIAN_POINT('Ctrl Pts',(374.056227285777,-15.1816120514834,-0.0752889519820703));
#37438=CARTESIAN_POINT('Ctrl Pts',(374.056777643753,-15.1834396202582,-0.0454547290851735));
#37439=CARTESIAN_POINT('Ctrl Pts',(374.056944580141,-15.1842991912654,-0.0314674935290114));
#37440=CARTESIAN_POINT('Ctrl Pts',(374.057115518403,-15.1862423225575,4.79464644808931E-5));
#37441=CARTESIAN_POINT('Ctrl Pts',(374.057067589397,-15.1873274823166,0.0175758795245109));
#37442=CARTESIAN_POINT('Ctrl Pts',(374.056577958902,-15.1901221470586,0.0625263277847719));
#37443=CARTESIAN_POINT('Ctrl Pts',(374.055929189083,-15.1918380525257,0.0899447401956231));
#37444=CARTESIAN_POINT('Ctrl Pts',(374.047285624018,-15.2067842976116,0.327161352660448));
#37445=CARTESIAN_POINT('Ctrl Pts',(374.019158402656,-15.2206551917808,0.535684977525285));
#37446=CARTESIAN_POINT('Ctrl Pts',(373.9206296805,-15.2495867121422,0.95334347585698));
#37447=CARTESIAN_POINT('Ctrl Pts',(373.848645715502,-15.26459357155,1.161043725027));
#37448=CARTESIAN_POINT('Ctrl Pts',(373.742062090989,-15.2809012068014,1.39005471166277));
#37449=CARTESIAN_POINT('Ctrl Pts',(373.727528603959,-15.2830315919661,1.42005648084333));
#37450=CARTESIAN_POINT('Ctrl Pts',(373.707093814898,-15.2858986397865,1.46062381908723));
#37451=CARTESIAN_POINT('Ctrl Pts',(373.701595242644,-15.2866580966725,1.47138847687503));
#37452=CARTESIAN_POINT('Ctrl Pts',(373.692279606572,-15.2879245438182,1.48937533860907));
#37453=CARTESIAN_POINT('Ctrl Pts',(373.688495454932,-15.2884335439982,1.49661434754555));
#37454=CARTESIAN_POINT('Ctrl Pts',(373.68125704012,-15.289396785489,1.51033398812035));
#37455=CARTESIAN_POINT('Ctrl Pts',(373.677808094293,-15.2898513651982,1.51681730641792));
#37456=CARTESIAN_POINT('Ctrl Pts',(373.669575173422,-15.290926288746,1.53216676074724));
#37457=CARTESIAN_POINT('Ctrl Pts',(373.664771693647,-15.2915454121538,1.54102242617792));
#37458=CARTESIAN_POINT('Ctrl Pts',(373.64773680582,-15.2937135463022,1.57207946848017));
#37459=CARTESIAN_POINT('Ctrl Pts',(373.635284720688,-15.2952493084193,1.59415957664774));
#37460=CARTESIAN_POINT('Ctrl Pts',(373.513707501154,-15.3098065356114,1.80391772552069));
#37461=CARTESIAN_POINT('Ctrl Pts',(373.386125988914,-15.3218226087251,1.98029024685482));
#37462=CARTESIAN_POINT('Ctrl Pts',(373.141814194786,-15.342378645182,2.25481247409797));
#37463=CARTESIAN_POINT('Ctrl Pts',(373.034138701614,-15.3508204547322,2.35997931752947));
#37464=CARTESIAN_POINT('Ctrl Pts',(372.877473715543,-15.3627418466324,2.49292461823461));
#37465=CARTESIAN_POINT('Ctrl Pts',(372.834516845515,-15.3659758919759,2.52752102546892));
#37466=CARTESIAN_POINT('Ctrl Pts',(372.758215635121,-15.3716791764802,2.58580846468359));
#37467=CARTESIAN_POINT('Ctrl Pts',(372.725268236795,-15.3741291221087,2.60999894859004));
#37468=CARTESIAN_POINT('Ctrl Pts',(372.676655439127,-15.3777303140805,2.64428751544775));
#37469=CARTESIAN_POINT('Ctrl Pts',(372.661347632427,-15.378862374457,2.65488726844239));
#37470=CARTESIAN_POINT('Ctrl Pts',(372.634271146596,-15.3808618280139,2.67329105811179));
#37471=CARTESIAN_POINT('Ctrl Pts',(372.622541324314,-15.3817270566629,2.68115157108491));
#37472=CARTESIAN_POINT('Ctrl Pts',(372.599580451992,-15.3834190486863,2.69632065294771));
#37473=CARTESIAN_POINT('Ctrl Pts',(372.588354716294,-15.384245505401,2.70363676932782));
#37474=CARTESIAN_POINT('Ctrl Pts',(372.558023627186,-15.3864766491972,2.72313595018312));
#37475=CARTESIAN_POINT('Ctrl Pts',(372.538835142652,-15.3878861620485,2.73518770220726));
#37476=CARTESIAN_POINT('Ctrl Pts',(372.466205231059,-15.3932148616151,2.77974343487143));
#37477=CARTESIAN_POINT('Ctrl Pts',(372.411951233608,-15.3971827967621,2.81088989862553));
#37478=CARTESIAN_POINT('Ctrl Pts',(372.341222145031,-15.4023427007326,2.84880159784428));
#37479=CARTESIAN_POINT('Ctrl Pts',(372.325552341488,-15.4034850341071,2.85703524452286));
#37480=CARTESIAN_POINT('Ctrl Pts',(372.309820571668,-15.4046310424783,2.8651368711395));
#37481=CARTESIAN_POINT('Origin',(370.834317853224,2.31077344927308,0.));
#37482=CARTESIAN_POINT('',(372.309820641399,-16.9034565314269,2.86513683522929));
#37483=CARTESIAN_POINT('',(372.309820496378,-16.659489044147,2.86513690991276));
#37484=CARTESIAN_POINT('',(372.309820613641,2.31077344927308,2.86513684952399));
#37485=CARTESIAN_POINT('',(367.611567947997,-16.0577322247446,-0.00078157510278719));
#37486=CARTESIAN_POINT('Ctrl Pts',(372.309820641399,-16.9034565314269,2.86513683522934));
#37487=CARTESIAN_POINT('Ctrl Pts',(372.325909722202,-16.9022323513834,2.85685119829489));
#37488=CARTESIAN_POINT('Ctrl Pts',(372.341930769895,-16.9010077354113,2.84842913430061));
#37489=CARTESIAN_POINT('Ctrl Pts',(372.505759160986,-16.8884311056161,2.76053675089465));
#37490=CARTESIAN_POINT('Ctrl Pts',(372.647228207769,-16.8771027798122,2.66976513787703));
#37491=CARTESIAN_POINT('Ctrl Pts',(372.80246186057,-16.8645883578776,2.55210744017415));
#37492=CARTESIAN_POINT('Ctrl Pts',(372.823726159882,-16.8628724789041,2.53556658744123));
#37493=CARTESIAN_POINT('Ctrl Pts',(372.85284972562,-16.8605230212038,2.51232028550546));
#37494=CARTESIAN_POINT('Ctrl Pts',(372.860887248126,-16.859874683756,2.50584130209764));
#37495=CARTESIAN_POINT('Ctrl Pts',(372.874635760793,-16.8587659944343,2.49464931815305));
#37496=CARTESIAN_POINT('Ctrl Pts',(372.880361838071,-16.8583043355179,2.48995509983542));
#37497=CARTESIAN_POINT('Ctrl Pts',(372.892313323745,-16.8573410536013,2.4800882474694));
#37498=CARTESIAN_POINT('Ctrl Pts',(372.898535493,-16.8568397291628,2.47491183869975));
#37499=CARTESIAN_POINT('Ctrl Pts',(372.913733967472,-16.8556154366311,2.4621705838769));
#37500=CARTESIAN_POINT('Ctrl Pts',(372.922688679771,-16.8548943228249,2.45457993575919));
#37501=CARTESIAN_POINT('Ctrl Pts',(372.955098319559,-16.8522843683828,2.42680148232818));
#37502=CARTESIAN_POINT('Ctrl Pts',(372.978304460663,-16.8504154960276,2.4063243357264));
#37503=CARTESIAN_POINT('Ctrl Pts',(373.035868637231,-16.8457687630433,2.35403561752845));
#37504=CARTESIAN_POINT('Ctrl Pts',(373.069835922902,-16.8430167664751,2.32180294956494));
#37505=CARTESIAN_POINT('Ctrl Pts',(373.341360001274,-16.8208157859511,2.05265946845745));
#37506=CARTESIAN_POINT('Ctrl Pts',(373.541299064155,-16.8029432288099,1.78071996647468));
#37507=CARTESIAN_POINT('Ctrl Pts',(373.725373100968,-16.7795282714451,1.42551050641333));
#37508=CARTESIAN_POINT('Ctrl Pts',(373.75333113971,-16.7757013781764,1.36734825183877));
#37509=CARTESIAN_POINT('Ctrl Pts',(373.788830260338,-16.7704333959477,1.28743912752393));
#37510=CARTESIAN_POINT('Ctrl Pts',(373.797913069125,-16.7690449222066,1.26639110291828));
#37511=CARTESIAN_POINT('Ctrl Pts',(373.812541765713,-16.7667391386269,1.23147187965546));
#37512=CARTESIAN_POINT('Ctrl Pts',(373.818217226164,-16.765826244692,1.21765560963807));
#37513=CARTESIAN_POINT('Ctrl Pts',(373.829117726463,-16.7640362766019,1.19058566772046));
#37514=CARTESIAN_POINT('Ctrl Pts',(373.83435133797,-16.7631595166423,1.17733580297789));
#37515=CARTESIAN_POINT('Ctrl Pts',(373.846524403341,-16.7610782894638,1.1459091609273));
#37516=CARTESIAN_POINT('Ctrl Pts',(373.853387378807,-16.759871294863,1.12770354204574));
#37517=CARTESIAN_POINT('Ctrl Pts',(373.875825271191,-16.755809160591,1.06650869819381));
#37518=CARTESIAN_POINT('Ctrl Pts',(373.890649521697,-16.7529293804579,1.02325195564793));
#37519=CARTESIAN_POINT('Ctrl Pts',(373.923962025596,-16.7459560656058,0.918855254082635));
#37520=CARTESIAN_POINT('Ctrl Pts',(373.941562200785,-16.7418357351535,0.857454239297127));
#37521=CARTESIAN_POINT('Ctrl Pts',(374.003524581494,-16.7254431429028,0.614222323204082));
#37522=CARTESIAN_POINT('Ctrl Pts',(374.03383462416,-16.7127939529725,0.4292076850403));
#37523=CARTESIAN_POINT('Ctrl Pts',(374.052274408795,-16.6962283953781,0.184976232893961));
#37524=CARTESIAN_POINT('Ctrl Pts',(374.055075140046,-16.6923227461787,0.127213662083228));
#37525=CARTESIAN_POINT('Ctrl Pts',(374.057610445119,-16.6844200056457,0.00951870105741554));
#37526=CARTESIAN_POINT('Ctrl Pts',(374.05723060713,-16.6804261206773,-0.0503957971463344));
#37527=CARTESIAN_POINT('Ctrl Pts',(374.053034137692,-16.6723548701964,-0.172973011430824));
#37528=CARTESIAN_POINT('Ctrl Pts',(374.049056479242,-16.6682841191934,-0.235607576669509));
#37529=CARTESIAN_POINT('Ctrl Pts',(374.041813555831,-16.6633151407042,-0.31357741551113));
#37530=CARTESIAN_POINT('Ctrl Pts',(374.040262782967,-16.6623336884095,-0.329054110797701));
#37531=CARTESIAN_POINT('Ctrl Pts',(374.037636352438,-16.6607929462501,-0.353481838647011));
#37532=CARTESIAN_POINT('Ctrl Pts',(374.036635105261,-16.6602296732624,-0.362440394593988));
#37533=CARTESIAN_POINT('Ctrl Pts',(374.034780488765,-16.6592278542868,-0.378426467662355));
#37534=CARTESIAN_POINT('Ctrl Pts',(374.033941557743,-16.6587885247435,-0.385455345868134));
#37535=CARTESIAN_POINT('Ctrl Pts',(374.031872864361,-16.6577374339569,-0.402315388999192));
#37536=CARTESIAN_POINT('Ctrl Pts',(374.03062092058,-16.6571269237507,-0.412143699649872));
#37537=CARTESIAN_POINT('Ctrl Pts',(374.026671092672,-16.6552754778802,-0.442050649803302));
#37538=CARTESIAN_POINT('Ctrl Pts',(374.023829132134,-16.6540423092407,-0.462110194509896));
#37539=CARTESIAN_POINT('Ctrl Pts',(373.996214745117,-16.6428908964535,-0.644613825384406));
#37540=CARTESIAN_POINT('Ctrl Pts',(373.959237736352,-16.6335771954796,-0.804989980482481));
#37541=CARTESIAN_POINT('Ctrl Pts',(373.829315695519,-16.6091555115711,-1.2204572388388));
#37542=CARTESIAN_POINT('Ctrl Pts',(373.716174339148,-16.594215009074,-1.46779347140523));
#37543=CARTESIAN_POINT('Ctrl Pts',(373.555299592743,-16.5760459106668,-1.72729839558306));
#37544=CARTESIAN_POINT('Ctrl Pts',(373.536704302207,-16.5739825942352,-1.75624847873965));
#37545=CARTESIAN_POINT('Ctrl Pts',(373.507903350223,-16.5708382231381,-1.79954656094379));
#37546=CARTESIAN_POINT('Ctrl Pts',(373.498037417929,-16.5697697824507,-1.81411832481062));
#37547=CARTESIAN_POINT('Ctrl Pts',(373.480635499177,-16.5678998009398,-1.83937254616221));
#37548=CARTESIAN_POINT('Ctrl Pts',(373.473152872376,-16.5671002912839,-1.85009139791578));
#37549=CARTESIAN_POINT('Ctrl Pts',(373.457339398711,-16.5654199530555,-1.87245306672002));
#37550=CARTESIAN_POINT('Ctrl Pts',(373.448995786434,-16.5645386465747,-1.88408646569699));
#37551=CARTESIAN_POINT('Ctrl Pts',(373.428898112143,-16.5624280861523,-1.91171779454894));
#37552=CARTESIAN_POINT('Ctrl Pts',(373.417073309084,-16.5611961088051,-1.92766331938697));
#37553=CARTESIAN_POINT('Ctrl Pts',(373.376078744505,-16.5569575585351,-1.98188934212332));
#37554=CARTESIAN_POINT('Ctrl Pts',(373.346200349984,-16.5539233328718,-2.0196236565588));
#37555=CARTESIAN_POINT('Ctrl Pts',(373.22974159564,-16.542293448099,-2.16011955613223));
#37556=CARTESIAN_POINT('Ctrl Pts',(373.137618444344,-16.5334798573043,-2.25808995462906));
#37557=CARTESIAN_POINT('Ctrl Pts',(372.896009439958,-16.5113436817431,-2.48482478203979));
#37558=CARTESIAN_POINT('Ctrl Pts',(372.740306805638,-16.4978641595868,-2.60617130714752));
#37559=CARTESIAN_POINT('Ctrl Pts',(372.495855143005,-16.4785027089262,-2.76299522431061));
#37560=CARTESIAN_POINT('Ctrl Pts',(372.415042136443,-16.4723665423346,-2.81001119069164));
#37561=CARTESIAN_POINT('Ctrl Pts',(372.318203714575,-16.4654097092436,-2.86084839102259));
#37562=CARTESIAN_POINT('Ctrl Pts',(372.304059840075,-16.4644032324974,-2.86814038740558));
#37563=CARTESIAN_POINT('Ctrl Pts',(372.280988626841,-16.4627777540035,-2.87981946543494));
#37564=CARTESIAN_POINT('Ctrl Pts',(372.272094160435,-16.4621549915347,-2.88427040642093));
#37565=CARTESIAN_POINT('Ctrl Pts',(372.256158973332,-16.4610463989456,-2.8921526120886));
#37566=CARTESIAN_POINT('Ctrl Pts',(372.249126226424,-16.4605596217961,-2.89559944979315));
#37567=CARTESIAN_POINT('Ctrl Pts',(372.233723147319,-16.4594989209627,-2.90307917661999));
#37568=CARTESIAN_POINT('Ctrl Pts',(372.225347918544,-16.458925646247,-2.90710151960614));
#37569=CARTESIAN_POINT('Ctrl Pts',(372.201371805636,-16.4572940665186,-2.91848910916759));
#37570=CARTESIAN_POINT('Ctrl Pts',(372.185728747011,-16.4562410633533,-2.92576550929154));
#37571=CARTESIAN_POINT('Ctrl Pts',(372.075285116867,-16.4488820900499,-2.97606378893287));
#37572=CARTESIAN_POINT('Ctrl Pts',(371.978497226611,-16.4428215134212,-3.01460006081601));
#37573=CARTESIAN_POINT('Ctrl Pts',(371.675401585834,-16.4245262844205,-3.11857079053734));
#37574=CARTESIAN_POINT('Ctrl Pts',(371.464249767503,-16.4126886525198,-3.16798013063101));
#37575=CARTESIAN_POINT('Ctrl Pts',(371.116237981162,-16.3927453744618,-3.21321657456114));
#37576=CARTESIAN_POINT('Ctrl Pts',(370.981800657999,-16.3849477960543,-3.22218596219761));
#37577=CARTESIAN_POINT('Ctrl Pts',(370.818545452719,-16.3751654088909,-3.22283884775045));
#37578=CARTESIAN_POINT('Ctrl Pts',(370.789885301376,-16.3734367211124,-3.22257112805646));
#37579=CARTESIAN_POINT('Ctrl Pts',(370.744881476628,-16.370702813201,-3.2215502811411));
#37580=CARTESIAN_POINT('Ctrl Pts',(370.72853304133,-16.3697056480773,-3.22105489514798));
#37581=CARTESIAN_POINT('Ctrl Pts',(370.698396849238,-16.3678597907341,-3.21991204055672));
#37582=CARTESIAN_POINT('Ctrl Pts',(370.684608057561,-16.3670122400859,-3.219300395418));
#37583=CARTESIAN_POINT('Ctrl Pts',(370.654065400149,-16.3651280978956,-3.21774893114551));
#37584=CARTESIAN_POINT('Ctrl Pts',(370.637314176059,-16.3640902036087,-3.21676680299875));
#37585=CARTESIAN_POINT('Ctrl Pts',(370.589171527548,-16.3610939258599,-3.2135667356678));
#37586=CARTESIAN_POINT('Ctrl Pts',(370.557804610997,-16.3591253182421,-3.21101980679819));
#37587=CARTESIAN_POINT('Ctrl Pts',(370.487169381023,-16.3546538388649,-3.20424173956248));
#37588=CARTESIAN_POINT('Ctrl Pts',(370.447931989098,-16.3521431032443,-3.19974732322143));
#37589=CARTESIAN_POINT('Ctrl Pts',(370.320135022441,-16.3438762244035,-3.18272406280029));
#37590=CARTESIAN_POINT('Ctrl Pts',(370.23201853106,-16.3380340783113,-3.16723060599847));
#37591=CARTESIAN_POINT('Ctrl Pts',(370.006507465763,-16.3227377422392,-3.11782799692219));
#37592=CARTESIAN_POINT('Ctrl Pts',(369.870498325785,-16.3131693936757,-3.07850108825781));
#37593=CARTESIAN_POINT('Ctrl Pts',(369.582656729771,-16.2924635401514,-2.974321187145));
#37594=CARTESIAN_POINT('Ctrl Pts',(369.432301889864,-16.2813548480603,-2.90647616002652));
#37595=CARTESIAN_POINT('Ctrl Pts',(369.264158619013,-16.2690415811167,-2.81450573788576));
#37596=CARTESIAN_POINT('Ctrl Pts',(369.240697529743,-16.2673264597083,-2.80128844353948));
#37597=CARTESIAN_POINT('Ctrl Pts',(369.208468468072,-16.2649773420076,-2.78259555850076));
#37598=CARTESIAN_POINT('Ctrl Pts',(369.19955777666,-16.2643286069238,-2.77736993651894));
#37599=CARTESIAN_POINT('Ctrl Pts',(369.184301980301,-16.263219416897,-2.76832440798745));
#37600=CARTESIAN_POINT('Ctrl Pts',(369.177944699307,-16.2627576523458,-2.76452534558062));
#37601=CARTESIAN_POINT('Ctrl Pts',(369.164807622842,-16.2618044568689,-2.75661314556102));
#37602=CARTESIAN_POINT('Ctrl Pts',(369.158029838833,-16.2613132540862,-2.75249685523508));
#37603=CARTESIAN_POINT('Ctrl Pts',(369.141582255117,-16.260122497351,-2.74242460843516));
#37604=CARTESIAN_POINT('Ctrl Pts',(369.131928496297,-16.2594246399089,-2.73644240291207));
#37605=CARTESIAN_POINT('Ctrl Pts',(369.111212317908,-16.2579289012428,-2.72345301840999));
#37606=CARTESIAN_POINT('Ctrl Pts',(369.100160531888,-16.2571320649984,-2.71642916841906));
#37607=CARTESIAN_POINT('Ctrl Pts',(369.069251640905,-16.2549057747582,-2.69651982109413));
#37608=CARTESIAN_POINT('Ctrl Pts',(369.049492844587,-16.2534852232699,-2.68348237110937));
#37609=CARTESIAN_POINT('Ctrl Pts',(368.983985918588,-16.2487781135972,-2.63921527155641));
#37610=CARTESIAN_POINT('Ctrl Pts',(368.93889752219,-16.2455422602912,-2.60702281492231));
#37611=CARTESIAN_POINT('Ctrl Pts',(368.799243045708,-16.2354573079859,-2.50177205215575));
#37612=CARTESIAN_POINT('Ctrl Pts',(368.707894629632,-16.2287645624368,-2.42460722287221));
#37613=CARTESIAN_POINT('Ctrl Pts',(368.450036902546,-16.2089234129788,-2.18097843011303));
#37614=CARTESIAN_POINT('Ctrl Pts',(368.297259405153,-16.1958088288278,-2.00119524996881));
#37615=CARTESIAN_POINT('Ctrl Pts',(368.142377486986,-16.1793981642233,-1.77236102539354));
#37616=CARTESIAN_POINT('Ctrl Pts',(368.119995923379,-16.1769349825886,-1.73789032184905));
#37617=CARTESIAN_POINT('Ctrl Pts',(368.088530507135,-16.1733305634356,-1.68733809187866));
#37618=CARTESIAN_POINT('Ctrl Pts',(368.078915503128,-16.1722088668653,-1.67159081517988));
#37619=CARTESIAN_POINT('Ctrl Pts',(368.062174494859,-16.1702191035882,-1.64363577052792));
#37620=CARTESIAN_POINT('Ctrl Pts',(368.054992537633,-16.1693531039936,-1.6314619595809));
#37621=CARTESIAN_POINT('Ctrl Pts',(368.040260998156,-16.167550611066,-1.60611159725536));
#37622=CARTESIAN_POINT('Ctrl Pts',(368.032724016678,-16.1666136902732,-1.59292816367406));
#37623=CARTESIAN_POINT('Ctrl Pts',(368.013478835883,-16.164182528865,-1.55870603339544));
#37624=CARTESIAN_POINT('Ctrl Pts',(368.001912893915,-16.1626832516834,-1.53758881247696));
#37625=CARTESIAN_POINT('Ctrl Pts',(367.952346208536,-16.1560861030596,-1.44463208451442));
#37626=CARTESIAN_POINT('Ctrl Pts',(367.91683684042,-16.1509018547886,-1.37150467360372));
#37627=CARTESIAN_POINT('Ctrl Pts',(367.825785047635,-16.1362280826729,-1.16441504258489));
#37628=CARTESIAN_POINT('Ctrl Pts',(367.776464921742,-16.1265584651244,-1.02793951760935));
#37629=CARTESIAN_POINT('Ctrl Pts',(367.680143790595,-16.1029930879962,-0.692155113000229));
#37630=CARTESIAN_POINT('Ctrl Pts',(367.64260182306,-16.0890276708331,-0.490764710893553));
#37631=CARTESIAN_POINT('Ctrl Pts',(367.620767434018,-16.0731142928088,-0.246701889451502));
#37632=CARTESIAN_POINT('Ctrl Pts',(367.61791261563,-16.0705057516962,-0.206169398443341));
#37633=CARTESIAN_POINT('Ctrl Pts',(367.61513268978,-16.0670833664798,-0.152137864877246));
#37634=CARTESIAN_POINT('Ctrl Pts',(367.614524841718,-16.0662354427632,-0.138679574765838));
#37635=CARTESIAN_POINT('Ctrl Pts',(367.613672552055,-16.0648622698571,-0.116760590996401));
#37636=CARTESIAN_POINT('Ctrl Pts',(367.613377023756,-16.0643342638905,-0.108302209163852));
#37637=CARTESIAN_POINT('Ctrl Pts',(367.612884972192,-16.0633469595842,-0.0924272495048247));
#37638=CARTESIAN_POINT('Ctrl Pts',(367.61268073451,-16.0628872413884,-0.085011057575803));
#37639=CARTESIAN_POINT('Ctrl Pts',(367.612310034364,-16.0619361444319,-0.0696190826078667));
#37640=CARTESIAN_POINT('Ctrl Pts',(367.612147572256,-16.0614449863556,-0.0616432077410594));
#37641=CARTESIAN_POINT('Ctrl Pts',(367.611861842461,-16.0603919769561,-0.0444871727029009));
#37642=CARTESIAN_POINT('Ctrl Pts',(367.611748183298,-16.0598306413629,-0.0353068958615575));
#37643=CARTESIAN_POINT('Ctrl Pts',(367.611605266647,-16.0587566060512,-0.0176782066592246));
#37644=CARTESIAN_POINT('Ctrl Pts',(367.611569996882,-16.0582436059849,-0.00922995489554233));
#37645=CARTESIAN_POINT('Ctrl Pts',(367.611567947997,-16.0577322247446,-0.00078157510278719));
#37646=CARTESIAN_POINT('Ctrl Pts',(367.611567948554,-16.0577323635611,-0.000783868448169546));
#37647=CARTESIAN_POINT('Ctrl Pts',(367.611558543255,-16.0553917611876,0.0378845160265506));
#37648=CARTESIAN_POINT('Ctrl Pts',(367.612245086453,-16.0530852721127,0.076552140657268));
#37649=CARTESIAN_POINT('Ctrl Pts',(367.61924901596,-16.041536127642,0.272363362098293));
#37650=CARTESIAN_POINT('Ctrl Pts',(367.636367475431,-16.032722440087,0.428919686002358));
#37651=CARTESIAN_POINT('Ctrl Pts',(367.696311832866,-16.0142065883644,0.754463912204947));
#37652=CARTESIAN_POINT('Ctrl Pts',(367.741534008391,-16.0045302483034,0.922486301583004));
#37653=CARTESIAN_POINT('Ctrl Pts',(367.820264686816,-15.991020743859,1.14244968281997));
#37654=CARTESIAN_POINT('Ctrl Pts',(367.842025001008,-15.987516969942,1.19828654531898));
#37655=CARTESIAN_POINT('Ctrl Pts',(367.882268797683,-15.9813819831846,1.29360773869993));
#37656=CARTESIAN_POINT('Ctrl Pts',(367.900020506377,-15.9787744610406,1.33338419662031));
#37657=CARTESIAN_POINT('Ctrl Pts',(367.926702488772,-15.9749848335776,1.39005566491259));
#37658=CARTESIAN_POINT('Ctrl Pts',(367.934985851469,-15.9738249330681,1.40725114265235));
#37659=CARTESIAN_POINT('Ctrl Pts',(367.949690306032,-15.971793802957,1.43709521717563));
#37660=CARTESIAN_POINT('Ctrl Pts',(367.956043128462,-15.9709249675335,1.44977699936811));
#37661=CARTESIAN_POINT('Ctrl Pts',(367.968491948276,-15.9692388069575,1.47422352688446));
#37662=CARTESIAN_POINT('Ctrl Pts',(367.97457720096,-15.9684218725892,1.48599344484594));
#37663=CARTESIAN_POINT('Ctrl Pts',(367.990916067982,-15.9662473617425,1.51712352738365));
#37664=CARTESIAN_POINT('Ctrl Pts',(368.001294670479,-15.9648853863186,1.53641697388562));
#37665=CARTESIAN_POINT('Ctrl Pts',(368.039587657036,-15.9599278808336,1.6058948649576));
#37666=CARTESIAN_POINT('Ctrl Pts',(368.068644050648,-15.9562919096499,1.65543436205101));
#37667=CARTESIAN_POINT('Ctrl Pts',(368.234340344584,-15.9362010568114,1.92138858625597));
#37668=CARTESIAN_POINT('Ctrl Pts',(368.395049497262,-15.9188529075266,2.12168455659783));
#37669=CARTESIAN_POINT('Ctrl Pts',(368.687444003093,-15.8911977730566,2.40845922980061));
#37670=CARTESIAN_POINT('Ctrl Pts',(368.804752641828,-15.8809063011847,2.50811063957212));
#37671=CARTESIAN_POINT('Ctrl Pts',(368.939328040708,-15.8702824408994,2.60678031072377));
#37672=CARTESIAN_POINT('Ctrl Pts',(368.949964974113,-15.8694503064739,2.61447972226268));
#37673=CARTESIAN_POINT('Ctrl Pts',(368.96991709048,-15.8679039912597,2.62873679149439));
#37674=CARTESIAN_POINT('Ctrl Pts',(368.979220523612,-15.867188801396,2.635310461769));
#37675=CARTESIAN_POINT('Ctrl Pts',(368.995043066117,-15.8659825908233,2.64636512787702));
#37676=CARTESIAN_POINT('Ctrl Pts',(369.001544124791,-15.8654898633921,2.65087166751089));
#37677=CARTESIAN_POINT('Ctrl Pts',(369.014156817787,-15.864539567564,2.65954621850779));
#37678=CARTESIAN_POINT('Ctrl Pts',(369.020266282239,-15.8640817895662,2.6637171741215));
#37679=CARTESIAN_POINT('Ctrl Pts',(369.034914581061,-15.8629901153259,2.6736438550759));
#37680=CARTESIAN_POINT('Ctrl Pts',(369.043466808301,-15.8623575333972,2.6793798053355));
#37681=CARTESIAN_POINT('Ctrl Pts',(369.074313013917,-15.860092495342,2.69985458281451));
#37682=CARTESIAN_POINT('Ctrl Pts',(369.09676331998,-15.8584748932765,2.71435741049251));
#37683=CARTESIAN_POINT('Ctrl Pts',(369.275571127005,-15.8458120799247,2.82673898134911));
#37684=CARTESIAN_POINT('Ctrl Pts',(369.439910331565,-15.8354819853616,2.911320943536));
#37685=CARTESIAN_POINT('Ctrl Pts',(369.770306512907,-15.8155061306556,3.0469328305337));
#37686=CARTESIAN_POINT('Ctrl Pts',(369.935013743376,-15.8058870282335,3.09954306551405));
#37687=CARTESIAN_POINT('Ctrl Pts',(370.161284180084,-15.7924507460144,3.15225450396176));
#37688=CARTESIAN_POINT('Ctrl Pts',(370.219799101908,-15.7889587599341,3.16418218238292));
#37689=CARTESIAN_POINT('Ctrl Pts',(370.321397456469,-15.7828425807606,3.18196749943756));
#37690=CARTESIAN_POINT('Ctrl Pts',(370.364331130253,-15.7802418760712,3.18859165005315));
#37691=CARTESIAN_POINT('Ctrl Pts',(370.426282439285,-15.7764604032467,3.19687162561534));
#37692=CARTESIAN_POINT('Ctrl Pts',(370.445202503272,-15.7753017049714,3.19922964320208));
#37693=CARTESIAN_POINT('Ctrl Pts',(370.478228966909,-15.7732719748428,3.20304844818476));
#37694=CARTESIAN_POINT('Ctrl Pts',(370.492326282178,-15.7724033273363,3.20458428061597));
#37695=CARTESIAN_POINT('Ctrl Pts',(370.521426418436,-15.7706053857465,3.20756039123727));
#37696=CARTESIAN_POINT('Ctrl Pts',(370.536430102122,-15.7696757335476,3.2089885616552));
#37697=CARTESIAN_POINT('Ctrl Pts',(370.5749026246,-15.7672848663603,3.21237854653832));
#37698=CARTESIAN_POINT('Ctrl Pts',(370.598383634439,-15.765818927103,3.21418841766123));
#37699=CARTESIAN_POINT('Ctrl Pts',(370.69098732607,-15.7600100085974,3.22030593670393));
#37700=CARTESIAN_POINT('Ctrl Pts',(370.760217317485,-15.7556062413676,3.22264206790362));
#37701=CARTESIAN_POINT('Ctrl Pts',(371.159343406374,-15.7298520816828,3.22324310190208));
#37702=CARTESIAN_POINT('Ctrl Pts',(371.487257202047,-15.7069787162743,3.17309562573088));
#37703=CARTESIAN_POINT('Ctrl Pts',(371.846259928825,-15.6821398371778,3.06010812443847));
#37704=CARTESIAN_POINT('Ctrl Pts',(371.890397785148,-15.6790950398932,3.04515748598768));
#37705=CARTESIAN_POINT('Ctrl Pts',(371.963182546608,-15.6741060238483,3.01873034918337));
#37706=CARTESIAN_POINT('Ctrl Pts',(371.992015796015,-15.6721381590867,3.00779056004922));
#37707=CARTESIAN_POINT('Ctrl Pts',(372.031587989533,-15.6694534521488,2.99212285804948));
#37708=CARTESIAN_POINT('Ctrl Pts',(372.042463770167,-15.668717298722,2.9877480533522));
#37709=CARTESIAN_POINT('Ctrl Pts',(372.060805027621,-15.6674789931086,2.98025371896806));
#37710=CARTESIAN_POINT('Ctrl Pts',(372.068283007404,-15.6669750145239,2.97716526611397));
#37711=CARTESIAN_POINT('Ctrl Pts',(372.082585473385,-15.6660129224498,2.97119511054539));
#37712=CARTESIAN_POINT('Ctrl Pts',(372.089411736594,-15.6655545267642,2.96831800570742));
#37713=CARTESIAN_POINT('Ctrl Pts',(372.105739531959,-15.6644598424752,2.96136983962954));
#37714=CARTESIAN_POINT('Ctrl Pts',(372.115231586048,-15.6638248846716,2.95727652207977));
#37715=CARTESIAN_POINT('Ctrl Pts',(372.149479209147,-15.6615385423578,2.94231187670626));
#37716=CARTESIAN_POINT('Ctrl Pts',(372.174118198749,-15.6599023946376,2.93117445996874));
#37717=CARTESIAN_POINT('Ctrl Pts',(372.236039048279,-15.6558055709026,2.90224079126109));
#37718=CARTESIAN_POINT('Ctrl Pts',(372.273114281798,-15.6533665221963,2.88404006384538));
#37719=CARTESIAN_POINT('Ctrl Pts',(372.309820655984,-15.6509557951682,2.86513682771809));
#37720=CARTESIAN_POINT('Ctrl Pts',(372.309820571668,-15.4046310424783,2.86513687113946));
#37721=CARTESIAN_POINT('Ctrl Pts',(372.025277739051,-15.4253590643006,3.01167218233879));
#37722=CARTESIAN_POINT('Ctrl Pts',(371.720480749908,-15.4475437349958,3.11501642052086));
#37723=CARTESIAN_POINT('Ctrl Pts',(371.359227982871,-15.471774267914,3.18006098518721));
#37724=CARTESIAN_POINT('Ctrl Pts',(371.31287769668,-15.4748406834038,3.1873655951699));
#37725=CARTESIAN_POINT('Ctrl Pts',(371.235664752265,-15.4798614659379,3.19781160499005));
#37726=CARTESIAN_POINT('Ctrl Pts',(371.204887598201,-15.4818398289967,3.20152410950472));
#37727=CARTESIAN_POINT('Ctrl Pts',(371.162374312456,-15.4845366789787,3.20603097630842));
#37728=CARTESIAN_POINT('Ctrl Pts',(371.150681339494,-15.485274690602,3.20720592043849));
#37729=CARTESIAN_POINT('Ctrl Pts',(371.130917739862,-15.4865154784946,3.20908268642529));
#37730=CARTESIAN_POINT('Ctrl Pts',(371.122850484533,-15.4870200941273,3.20981808002048));
#37731=CARTESIAN_POINT('Ctrl Pts',(371.107399355604,-15.4879829161681,3.21116784842592));
#37732=CARTESIAN_POINT('Ctrl Pts',(371.100016046143,-15.4884414084109,3.21178718638036));
#37733=CARTESIAN_POINT('Ctrl Pts',(371.082334832843,-15.4895357156332,3.21320896116639));
#37734=CARTESIAN_POINT('Ctrl Pts',(371.072035003531,-15.4901702043731,3.21398736984018));
#37735=CARTESIAN_POINT('Ctrl Pts',(371.03485625716,-15.4924503160593,3.2166174471686));
#37736=CARTESIAN_POINT('Ctrl Pts',(371.007957282404,-15.4940808213809,3.2181816153142));
#37737=CARTESIAN_POINT('Ctrl Pts',(370.813110436838,-15.5057733297517,3.2270616685182));
#37738=CARTESIAN_POINT('Ctrl Pts',(370.644816952915,-15.5152446234542,3.22156483063877));
#37739=CARTESIAN_POINT('Ctrl Pts',(370.330957683941,-15.5329290412395,3.18662007183154));
#37740=CARTESIAN_POINT('Ctrl Pts',(370.185509914545,-15.5411350240599,3.16021605524769));
#37741=CARTESIAN_POINT('Ctrl Pts',(369.920003521484,-15.5567519071712,3.09290928588405));
#37742=CARTESIAN_POINT('Ctrl Pts',(369.799558618616,-15.564090614991,3.05472201469633));
#37743=CARTESIAN_POINT('Ctrl Pts',(369.655977875133,-15.573314931458,2.99973157101965));
#37744=CARTESIAN_POINT('Ctrl Pts',(369.630411240774,-15.5749761358368,2.98956240936314));
#37745=CARTESIAN_POINT('Ctrl Pts',(369.590239987775,-15.5776173351037,2.97298537543862));
#37746=CARTESIAN_POINT('Ctrl Pts',(369.575546992478,-15.5785900112208,2.96679417616491));
#37747=CARTESIAN_POINT('Ctrl Pts',(369.548061419041,-15.5804223151932,2.95497162358561));
#37748=CARTESIAN_POINT('Ctrl Pts',(369.535258317569,-15.5812810651284,2.94936556291936));
#37749=CARTESIAN_POINT('Ctrl Pts',(369.506607139596,-15.5832147886038,2.93659739719836));
#37750=CARTESIAN_POINT('Ctrl Pts',(369.490779851015,-15.5842912969811,2.92938997573834));
#37751=CARTESIAN_POINT('Ctrl Pts',(369.450554468205,-15.5870488500567,2.91067759585452));
#37752=CARTESIAN_POINT('Ctrl Pts',(369.426241445198,-15.588736010971,2.89899395149917));
#37753=CARTESIAN_POINT('Ctrl Pts',(369.261210994774,-15.6003309907493,2.81712261552336));
#37754=CARTESIAN_POINT('Ctrl Pts',(369.125667843278,-15.610585849957,2.73703260199142));
#37755=CARTESIAN_POINT('Ctrl Pts',(368.817334177866,-15.6356315725808,2.52298982554617));
#37756=CARTESIAN_POINT('Ctrl Pts',(368.651243842037,-15.6505984631149,2.38073184346979));
#37757=CARTESIAN_POINT('Ctrl Pts',(368.46388180627,-15.6686073600612,2.1840364852025));
#37758=CARTESIAN_POINT('Ctrl Pts',(368.427934161896,-15.6721197930694,2.14436484273628));
#37759=CARTESIAN_POINT('Ctrl Pts',(368.370704461978,-15.6777831504157,2.07795380187474));
#37760=CARTESIAN_POINT('Ctrl Pts',(368.348830592228,-15.6799659748668,2.05173980739089));
#37761=CARTESIAN_POINT('Ctrl Pts',(368.319710796621,-15.6828913834033,2.01569286317304));
#37762=CARTESIAN_POINT('Ctrl Pts',(368.312098982396,-15.6836579437112,2.00616009994196));
#37763=CARTESIAN_POINT('Ctrl Pts',(368.299466566243,-15.6849329290432,1.99015416829915));
#37764=CARTESIAN_POINT('Ctrl Pts',(368.294416248236,-15.6854434210197,1.98370474162987));
#37765=CARTESIAN_POINT('Ctrl Pts',(368.284896912626,-15.6864069898513,1.97145227540206));
#37766=CARTESIAN_POINT('Ctrl Pts',(368.280423007563,-15.6868604217393,1.96565315515727));
#37767=CARTESIAN_POINT('Ctrl Pts',(368.269889284293,-15.687929513276,1.95190256464055));
#37768=CARTESIAN_POINT('Ctrl Pts',(368.263846577545,-15.6885439841889,1.94393799645155));
#37769=CARTESIAN_POINT('Ctrl Pts',(368.242886760738,-15.6906800021544,1.91604336343282));
#37770=CARTESIAN_POINT('Ctrl Pts',(368.228163164279,-15.6921888085721,1.89596811703243));
#37771=CARTESIAN_POINT('Ctrl Pts',(368.083669887638,-15.7071022282203,1.69409107064014));
#37772=CARTESIAN_POINT('Ctrl Pts',(367.972882826127,-15.7194382937699,1.49940874058233));
#37773=CARTESIAN_POINT('Ctrl Pts',(367.797473221262,-15.7438675047481,1.09960503934842));
#37774=CARTESIAN_POINT('Ctrl Pts',(367.731418556255,-15.7558976998376,0.896413326277192));
#37775=CARTESIAN_POINT('Ctrl Pts',(367.678972346146,-15.770573726751,0.656480483783131));
#37776=CARTESIAN_POINT('Ctrl Pts',(367.672518443659,-15.7725284225183,0.624656923953805));
#37777=CARTESIAN_POINT('Ctrl Pts',(367.663420893998,-15.7755294644004,0.576037204796292));
#37778=CARTESIAN_POINT('Ctrl Pts',(367.660427362353,-15.7765646926789,0.559308074378739));
#37779=CARTESIAN_POINT('Ctrl Pts',(367.655217516292,-15.7784574667457,0.528803615118159));
#37780=CARTESIAN_POINT('Ctrl Pts',(367.652958061819,-15.7793136207491,0.515036002221224));
#37781=CARTESIAN_POINT('Ctrl Pts',(367.6482613794,-15.7811728488783,0.485206776664554));
#37782=CARTESIAN_POINT('Ctrl Pts',(367.645856068077,-15.782176908691,0.469140596973328));
#37783=CARTESIAN_POINT('Ctrl Pts',(367.639616551988,-15.7849307424308,0.425197558401056));
#37784=CARTESIAN_POINT('Ctrl Pts',(367.636025893485,-15.7866881317583,0.397288091169767));
#37785=CARTESIAN_POINT('Ctrl Pts',(367.618558134734,-15.7962699865278,0.245872203411862));
#37786=CARTESIAN_POINT('Ctrl Pts',(367.611470409427,-15.8043047509393,0.121702817941861));
#37787=CARTESIAN_POINT('Ctrl Pts',(367.61168598124,-15.8222767577775,-0.150361365533153));
#37788=CARTESIAN_POINT('Ctrl Pts',(367.621971522796,-15.8322681552496,-0.297976929090117));
#37789=CARTESIAN_POINT('Ctrl Pts',(367.665539758003,-15.853643745467,-0.610944278953389));
#37790=CARTESIAN_POINT('Ctrl Pts',(367.701738994466,-15.8649990219507,-0.775479145063843));
#37791=CARTESIAN_POINT('Ctrl Pts',(367.758450440369,-15.8775383431487,-0.96222819727075));
#37792=CARTESIAN_POINT('Ctrl Pts',(367.766602426614,-15.8792544997248,-0.987909720862183));
#37793=CARTESIAN_POINT('Ctrl Pts',(367.778324066333,-15.8816045791753,-1.02329185690301));
#37794=CARTESIAN_POINT('Ctrl Pts',(367.781619477406,-15.8822532628188,-1.03308125673883));
#37795=CARTESIAN_POINT('Ctrl Pts',(367.787359479625,-15.8833626048898,-1.049865290023));
#37796=CARTESIAN_POINT('Ctrl Pts',(367.789781207601,-15.8838245713511,-1.0568675762433));
#37797=CARTESIAN_POINT('Ctrl Pts',(367.794901190632,-15.8847885829895,-1.07150806527044));
#37798=CARTESIAN_POINT('Ctrl Pts',(367.797604125347,-15.885290328627,-1.07914453132832));
#37799=CARTESIAN_POINT('Ctrl Pts',(367.804298694291,-15.8865158264506,-1.09783403049992));
#37800=CARTESIAN_POINT('Ctrl Pts',(367.808322096293,-15.8872377195161,-1.10887571485367));
#37801=CARTESIAN_POINT('Ctrl Pts',(367.823177396167,-15.8898515546441,-1.14896107542089));
#37802=CARTESIAN_POINT('Ctrl Pts',(367.834368153605,-15.8917234602903,-1.17787111605591));
#37803=CARTESIAN_POINT('Ctrl Pts',(367.86353987318,-15.89637876482,-1.25011869018984));
#37804=CARTESIAN_POINT('Ctrl Pts',(367.882053696358,-15.89913618808,-1.2932344450927));
#37805=CARTESIAN_POINT('Ctrl Pts',(368.041566553706,-15.9214797048832,-1.64341800223679));
#37806=CARTESIAN_POINT('Ctrl Pts',(368.229112338637,-15.9394717597361,-1.92697354739763));
#37807=CARTESIAN_POINT('Ctrl Pts',(368.499548716523,-15.9629361954599,-2.22235961619356));
#37808=CARTESIAN_POINT('Ctrl Pts',(368.54311377023,-15.966648523197,-2.26724772926983));
#37809=CARTESIAN_POINT('Ctrl Pts',(368.604201983852,-15.971782663577,-2.32663150691058));
#37810=CARTESIAN_POINT('Ctrl Pts',(368.62061463122,-15.9731553309329,-2.34225296764824));
#37811=CARTESIAN_POINT('Ctrl Pts',(368.646992930526,-15.9753516226572,-2.36683476067277));
#37812=CARTESIAN_POINT('Ctrl Pts',(368.656852295318,-15.976170381231,-2.37590842361511));
#37813=CARTESIAN_POINT('Ctrl Pts',(368.677217144973,-15.9778573464397,-2.39441714750869));
#37814=CARTESIAN_POINT('Ctrl Pts',(368.687728614372,-15.9787258236816,-2.40384516377056));
#37815=CARTESIAN_POINT('Ctrl Pts',(368.712244216327,-15.980746332422,-2.4255448343693));
#37816=CARTESIAN_POINT('Ctrl Pts',(368.726293313437,-15.9819004817632,-2.43776470978677));
#37817=CARTESIAN_POINT('Ctrl Pts',(368.771519544025,-15.9856045333485,-2.47641908096368));
#37818=CARTESIAN_POINT('Ctrl Pts',(368.803093025258,-15.9881735076257,-2.50238162171343));
#37819=CARTESIAN_POINT('Ctrl Pts',(368.878410791953,-15.9942651626766,-2.56194987869804));
#37820=CARTESIAN_POINT('Ctrl Pts',(368.922539942347,-15.9978064962388,-2.59504609852665));
#37821=CARTESIAN_POINT('Ctrl Pts',(369.090063792928,-16.0111488235541,-2.71409381614047));
#37822=CARTESIAN_POINT('Ctrl Pts',(369.218566235213,-16.0211963058601,-2.792501681698));
#37823=CARTESIAN_POINT('Ctrl Pts',(369.544813190576,-16.0460031779589,-2.96148914426724));
#37824=CARTESIAN_POINT('Ctrl Pts',(369.747174718968,-16.0608317272373,-3.04160709039922));
#37825=CARTESIAN_POINT('Ctrl Pts',(369.980455695816,-16.0763865435603,-3.10768073246277));
#37826=CARTESIAN_POINT('Ctrl Pts',(370.004926514732,-16.0779994653569,-3.1143009197698));
#37827=CARTESIAN_POINT('Ctrl Pts',(370.03922905887,-16.0802318665744,-3.12314790999112));
#37828=CARTESIAN_POINT('Ctrl Pts',(370.04899625515,-16.0808642961358,-3.1256181872605));
#37829=CARTESIAN_POINT('Ctrl Pts',(370.065902776158,-16.0819532518912,-3.12980985998363));
#37830=CARTESIAN_POINT('Ctrl Pts',(370.073036630265,-16.0824109820555,-3.13155271270328));
#37831=CARTESIAN_POINT('Ctrl Pts',(370.088117928119,-16.0833748297816,-3.13518260307879));
#37832=CARTESIAN_POINT('Ctrl Pts',(370.096066703054,-16.0838805987039,-3.13706383815625));
#37833=CARTESIAN_POINT('Ctrl Pts',(370.115795270121,-16.0851305452592,-3.14165385704228));
#37834=CARTESIAN_POINT('Ctrl Pts',(370.127583451163,-16.0858726891269,-3.14432666172176));
#37835=CARTESIAN_POINT('Ctrl Pts',(370.171933471353,-16.0886480488088,-3.15412039216201));
#37836=CARTESIAN_POINT('Ctrl Pts',(370.204591337821,-16.0906578463273,-3.16080262460133));
#37837=CARTESIAN_POINT('Ctrl Pts',(370.45274566944,-16.1057138709211,-3.20757926218942));
#37838=CARTESIAN_POINT('Ctrl Pts',(370.671751067082,-16.117802492749,-3.22610578570191));
#37839=CARTESIAN_POINT('Ctrl Pts',(371.1009010831,-16.1418313442101,-3.21856153531412));
#37840=CARTESIAN_POINT('Ctrl Pts',(371.30994669702,-16.1537094556595,-3.19436478554087));
#37841=CARTESIAN_POINT('Ctrl Pts',(371.54194965591,-16.1679154334896,-3.14422121751639));
#37842=CARTESIAN_POINT('Ctrl Pts',(371.568682479037,-16.1695672960928,-3.13808514214414));
#37843=CARTESIAN_POINT('Ctrl Pts',(371.612365966074,-16.1722926536017,-3.12746957572566));
#37844=CARTESIAN_POINT('Ctrl Pts',(371.629364489063,-16.1733596873915,-3.12319157929255));
#37845=CARTESIAN_POINT('Ctrl Pts',(371.659864022225,-16.1752863105638,-3.11525067342172));
#37846=CARTESIAN_POINT('Ctrl Pts',(371.673377770979,-16.17614425493,-3.11163810236189));
#37847=CARTESIAN_POINT('Ctrl Pts',(371.702153805507,-16.1779805186812,-3.10374444500678));
#37848=CARTESIAN_POINT('Ctrl Pts',(371.717408836428,-16.1789596252393,-3.09943851705888));
#37849=CARTESIAN_POINT('Ctrl Pts',(371.758644542212,-16.1816218660906,-3.08747006962052));
#37850=CARTESIAN_POINT('Ctrl Pts',(371.784560932768,-16.1833119620926,-3.07959238805969));
#37851=CARTESIAN_POINT('Ctrl Pts',(371.923834492422,-16.1924881617337,-3.03533265652999));
#37852=CARTESIAN_POINT('Ctrl Pts',(372.035196464518,-16.2001672931004,-2.99302115859517));
#37853=CARTESIAN_POINT('Ctrl Pts',(372.286656963632,-16.2183016927497,-2.88118401238031));
#37854=CARTESIAN_POINT('Ctrl Pts',(372.424548989944,-16.2288576245951,-2.8074309045405));
#37855=CARTESIAN_POINT('Ctrl Pts',(372.698187026081,-16.2507576231464,-2.63442464190561));
#37856=CARTESIAN_POINT('Ctrl Pts',(372.832646419374,-16.2620696723749,-2.53394850991685));
#37857=CARTESIAN_POINT('Ctrl Pts',(372.978952845682,-16.2745698460313,-2.40569831769175));
#37858=CARTESIAN_POINT('Ctrl Pts',(372.998993015467,-16.2762862448348,-2.38768197186743));
#37859=CARTESIAN_POINT('Ctrl Pts',(373.02639998404,-16.2786365946828,-2.36241406028341));
#37860=CARTESIAN_POINT('Ctrl Pts',(373.033960786732,-16.2792853109311,-2.35537581552413));
#37861=CARTESIAN_POINT('Ctrl Pts',(373.046886597713,-16.2803946940512,-2.3432268371922));
#37862=CARTESIAN_POINT('Ctrl Pts',(373.052268005961,-16.2808566691676,-2.33813378193352));
#37863=CARTESIAN_POINT('Ctrl Pts',(373.063496010433,-16.281820682033,-2.32743376365624));
#37864=CARTESIAN_POINT('Ctrl Pts',(373.069339096466,-16.2823224203379,-2.32182325443305));
#37865=CARTESIAN_POINT('Ctrl Pts',(373.083606420539,-16.2835478725564,-2.30802005801452));
#37866=CARTESIAN_POINT('Ctrl Pts',(373.092007227394,-16.2842697276756,-2.29980311047356));
#37867=CARTESIAN_POINT('Ctrl Pts',(373.122400814623,-16.2868832678142,-2.26974767398716));
#37868=CARTESIAN_POINT('Ctrl Pts',(373.14412399018,-16.2887549223363,-2.24763740686851));
#37869=CARTESIAN_POINT('Ctrl Pts',(373.19791291814,-16.2934094718393,-2.19128640286177));
#37870=CARTESIAN_POINT('Ctrl Pts',(373.229557139794,-16.2961664019762,-2.15665178592457));
#37871=CARTESIAN_POINT('Ctrl Pts',(373.482690714373,-16.3184961462378,-1.86714954484856));
#37872=CARTESIAN_POINT('Ctrl Pts',(373.663628178267,-16.3364766525888,-1.57961056321843));
#37873=CARTESIAN_POINT('Ctrl Pts',(373.821331351251,-16.3599361288771,-1.21152925151641));
#37874=CARTESIAN_POINT('Ctrl Pts',(373.844346112093,-16.3636593570963,-1.15316168393667));
#37875=CARTESIAN_POINT('Ctrl Pts',(373.873343715202,-16.3688062916375,-1.07282522608097));
#37876=CARTESIAN_POINT('Ctrl Pts',(373.880819767758,-16.3701805283311,-1.0514077229525));
#37877=CARTESIAN_POINT('Ctrl Pts',(373.892352637534,-16.372378703109,-1.01721211911853));
#37878=CARTESIAN_POINT('Ctrl Pts',(373.896556988662,-16.3731977600452,-1.00448429863444));
#37879=CARTESIAN_POINT('Ctrl Pts',(373.905026222533,-16.3748848723642,-0.978298005006675));
#37880=CARTESIAN_POINT('Ctrl Pts',(373.909282309256,-16.375753195416,-0.964837012145004));
#37881=CARTESIAN_POINT('Ctrl Pts',(373.918941605234,-16.3777725488329,-0.933573766835426));
#37882=CARTESIAN_POINT('Ctrl Pts',(373.92427933988,-16.378925689385,-0.915751962765309));
#37883=CARTESIAN_POINT('Ctrl Pts',(373.940825948793,-16.3826231847994,-0.858713330257394));
#37884=CARTESIAN_POINT('Ctrl Pts',(373.951444414233,-16.3851865168706,-0.819330756820049));
#37885=CARTESIAN_POINT('Ctrl Pts',(373.974619922245,-16.3912624529728,-0.726392151438716));
#37886=CARTESIAN_POINT('Ctrl Pts',(373.986558577369,-16.3947935798126,-0.672696428392339));
#37887=CARTESIAN_POINT('Ctrl Pts',(374.025849689343,-16.4080786223829,-0.471847747902337));
#37888=CARTESIAN_POINT('Ctrl Pts',(374.04431361308,-16.418076710204,-0.323163328932099));
#37889=CARTESIAN_POINT('Ctrl Pts',(374.064142574974,-16.4429066093382,0.0440956859872955));
#37890=CARTESIAN_POINT('Ctrl Pts',(374.053754847137,-16.4578128503601,0.262585741215501));
#37891=CARTESIAN_POINT('Ctrl Pts',(374.017614573982,-16.4734322616272,0.503367580842284));
#37892=CARTESIAN_POINT('Ctrl Pts',(374.013567032374,-16.4750411104205,0.528329142222957));
#37893=CARTESIAN_POINT('Ctrl Pts',(374.007498328675,-16.4772688285565,0.563155852975093));
#37894=CARTESIAN_POINT('Ctrl Pts',(374.005724226252,-16.4779005791181,0.573062359578017));
#37895=CARTESIAN_POINT('Ctrl Pts',(374.002575834159,-16.4789886869301,0.590180326034277));
#37896=CARTESIAN_POINT('Ctrl Pts',(374.001223268762,-16.4794462438367,0.597395633215517));
#37897=CARTESIAN_POINT('Ctrl Pts',(373.998313051562,-16.480410105544,0.612632612996904));
#37898=CARTESIAN_POINT('Ctrl Pts',(373.996749522974,-16.4809160595897,0.620653099833034));
#37899=CARTESIAN_POINT('Ctrl Pts',(373.992794707616,-16.482167107379,0.640537262129272));
#37900=CARTESIAN_POINT('Ctrl Pts',(373.990367040153,-16.482910159428,0.652393718856743));
#37901=CARTESIAN_POINT('Ctrl Pts',(373.980980545483,-16.4856929606646,0.696957406043927));
#37902=CARTESIAN_POINT('Ctrl Pts',(373.973579337385,-16.487709128971,0.729570598966351));
#37903=CARTESIAN_POINT('Ctrl Pts',(373.913417886548,-16.502876781086,0.976776543161759));
#37904=CARTESIAN_POINT('Ctrl Pts',(373.839212363841,-16.5150558614424,1.18557298503233));
#37905=CARTESIAN_POINT('Ctrl Pts',(373.654800620771,-16.539080145388,1.57298082266496));
#37906=CARTESIAN_POINT('Ctrl Pts',(373.547428172945,-16.5508555038655,1.75168733897278));
#37907=CARTESIAN_POINT('Ctrl Pts',(373.407260112967,-16.5649454219879,1.94083445839598));
#37908=CARTESIAN_POINT('Ctrl Pts',(373.390644912604,-16.5665977522904,1.96266710433325));
#37909=CARTESIAN_POINT('Ctrl Pts',(373.362959355716,-16.5693237252037,1.99809835813762));
#37910=CARTESIAN_POINT('Ctrl Pts',(373.352052977023,-16.5703909016546,2.01182373095153));
#37911=CARTESIAN_POINT('Ctrl Pts',(373.332243703026,-16.5723176798561,2.03633977771281));
#37912=CARTESIAN_POINT('Ctrl Pts',(373.32338144701,-16.5731756354563,2.04716283127113));
#37913=CARTESIAN_POINT('Ctrl Pts',(373.30432820077,-16.5750118116152,2.07012503321343));
#37914=CARTESIAN_POINT('Ctrl Pts',(373.294117588436,-16.5759908185356,2.08224734804377));
#37915=CARTESIAN_POINT('Ctrl Pts',(373.266220519242,-16.5786525065559,2.11487595162464));
#37916=CARTESIAN_POINT('Ctrl Pts',(373.248364652252,-16.5803421444424,2.13523508025426));
#37917=CARTESIAN_POINT('Ctrl Pts',(373.150711199032,-16.5895105300705,2.24378809742133));
#37918=CARTESIAN_POINT('Ctrl Pts',(373.06634310773,-16.5971819105454,2.32772865472945));
#37919=CARTESIAN_POINT('Ctrl Pts',(372.861134771292,-16.6152870729816,2.51046307751723));
#37920=CARTESIAN_POINT('Ctrl Pts',(372.737372936722,-16.6258208207289,2.60552992763899));
#37921=CARTESIAN_POINT('Ctrl Pts',(372.511239339714,-16.6441391148463,2.75449903459483));
#37922=CARTESIAN_POINT('Ctrl Pts',(372.411958976517,-16.6519005815039,2.81253712073997));
#37923=CARTESIAN_POINT('Ctrl Pts',(372.309820496378,-16.659489044147,2.8651369099128));
#37924=CARTESIAN_POINT('Origin',(370.834317853224,2.31077344927308,0.));
#37925=CARTESIAN_POINT('',(372.309820613645,-18.1566220988445,2.86513684952226));
#37926=CARTESIAN_POINT('',(372.30982061364,-17.9078850417037,2.86513684952483));
#37927=CARTESIAN_POINT('',(372.309820613641,2.31077344927308,2.86513684952399));
#37928=CARTESIAN_POINT('Ctrl Pts',(372.309820613645,-18.1566220988445,2.86513684952223));
#37929=CARTESIAN_POINT('Ctrl Pts',(372.311272455587,-18.1565224746897,2.86438917256799));
#37930=CARTESIAN_POINT('Ctrl Pts',(372.312723729234,-18.1564228118652,2.86364039207921));
#37931=CARTESIAN_POINT('Ctrl Pts',(372.326767808063,-18.1554576139208,2.85638086804062));
#37932=CARTESIAN_POINT('Ctrl Pts',(372.339317931448,-18.1545892200256,2.84978828782492));
#37933=CARTESIAN_POINT('Ctrl Pts',(372.36512906347,-18.1527908926273,2.83601164631683));
#37934=CARTESIAN_POINT('Ctrl Pts',(372.378383934423,-18.1518605947356,2.82881688060898));
#37935=CARTESIAN_POINT('Ctrl Pts',(372.412247200125,-18.1494661414153,2.81012693188647));
#37936=CARTESIAN_POINT('Ctrl Pts',(372.432780445712,-18.1479972342059,2.79849811327024));
#37937=CARTESIAN_POINT('Ctrl Pts',(372.513369501142,-18.142163295722,2.75168093150799));
#37938=CARTESIAN_POINT('Ctrl Pts',(372.572402702544,-18.1377368166799,2.71477848919915));
#37939=CARTESIAN_POINT('Ctrl Pts',(372.903756766383,-18.1119825699006,2.49240520076421));
#37940=CARTESIAN_POINT('Ctrl Pts',(373.147485721579,-18.0891386287628,2.26800440197018));
#37941=CARTESIAN_POINT('Ctrl Pts',(373.382019222329,-18.0643288144873,1.97420987794159));
#37942=CARTESIAN_POINT('Ctrl Pts',(373.410286213246,-18.0612851649056,1.93718206565545));
#37943=CARTESIAN_POINT('Ctrl Pts',(373.455912336209,-18.0562978202709,1.87464937232052));
#37944=CARTESIAN_POINT('Ctrl Pts',(373.47372525588,-18.0543304981424,1.84948550355376));
#37945=CARTESIAN_POINT('Ctrl Pts',(373.497809231683,-18.0516464018496,1.81440585998606));
#37946=CARTESIAN_POINT('Ctrl Pts',(373.504390730472,-18.0509103276274,1.80470656563241));
#37947=CARTESIAN_POINT('Ctrl Pts',(373.515425294158,-18.0496721163653,1.78825219267867));
#37948=CARTESIAN_POINT('Ctrl Pts',(373.519906069262,-18.0491681535526,1.78151591444796));
#37949=CARTESIAN_POINT('Ctrl Pts',(373.528441075473,-18.0482060610674,1.76857923310684));
#37950=CARTESIAN_POINT('Ctrl Pts',(373.532499344245,-18.0477476494008,1.76238165122051));
#37951=CARTESIAN_POINT('Ctrl Pts',(373.542169638696,-18.0466528874298,1.74750197171174));
#37952=CARTESIAN_POINT('Ctrl Pts',(373.547761370958,-18.0460178683492,1.73880669312301));
#37953=CARTESIAN_POINT('Ctrl Pts',(373.567829863526,-18.0437310008234,1.70726713642371));
#37954=CARTESIAN_POINT('Ctrl Pts',(373.582061219956,-18.0420943985745,1.68426704681048));
#37955=CARTESIAN_POINT('Ctrl Pts',(373.680851554203,-18.0306056967888,1.52002083554513));
#37956=CARTESIAN_POINT('Ctrl Pts',(373.754778409436,-18.021318990523,1.37264003441066));
#37957=CARTESIAN_POINT('Ctrl Pts',(373.869780397681,-18.0043043085601,1.09152415619711));
#37958=CARTESIAN_POINT('Ctrl Pts',(373.91404932033,-17.9965759599883,0.959536767928402));
#37959=CARTESIAN_POINT('Ctrl Pts',(373.972914253652,-17.9835134164142,0.737281790762283));
#37960=CARTESIAN_POINT('Ctrl Pts',(373.992449289228,-17.9782858701628,0.648518210451095));
#37961=CARTESIAN_POINT('Ctrl Pts',(374.018501010872,-17.9694654434798,0.500615603629913));
#37962=CARTESIAN_POINT('Ctrl Pts',(374.027177755205,-17.9659365810877,0.441908752567425));
#37963=CARTESIAN_POINT('Ctrl Pts',(374.036785426267,-17.9610589387017,0.361637699410192));
#37964=CARTESIAN_POINT('Ctrl Pts',(374.039128103955,-17.9597544427021,0.340252265720417));
#37965=CARTESIAN_POINT('Ctrl Pts',(374.042704875131,-17.9575509014232,0.30427719254953));
#37966=CARTESIAN_POINT('Ctrl Pts',(374.04405399143,-17.9566554900278,0.289699506760121));
#37967=CARTESIAN_POINT('Ctrl Pts',(374.0465225546,-17.954880620755,0.260887665127171));
#37968=CARTESIAN_POINT('Ctrl Pts',(374.047646825911,-17.9540013358557,0.246654252351041));
#37969=CARTESIAN_POINT('Ctrl Pts',(374.05014874386,-17.9518575153502,0.212051944139108));
#37970=CARTESIAN_POINT('Ctrl Pts',(374.051427479241,-17.9505899111106,0.191676726808597));
#37971=CARTESIAN_POINT('Ctrl Pts',(374.054509972385,-17.9469714890389,0.133763252387256));
#37972=CARTESIAN_POINT('Ctrl Pts',(374.055850774254,-17.9446063798233,0.096204673597261));
#37973=CARTESIAN_POINT('Ctrl Pts',(374.060118796779,-17.9297162148921,-0.138349548598383));
#37974=CARTESIAN_POINT('Ctrl Pts',(374.045632434078,-17.9166524107532,-0.335213734643995));
#37975=CARTESIAN_POINT('Ctrl Pts',(373.977994876229,-17.8888800873244,-0.741293296357779));
#37976=CARTESIAN_POINT('Ctrl Pts',(373.921637211871,-17.8741982093691,-0.949047432136426));
#37977=CARTESIAN_POINT('Ctrl Pts',(373.833242583549,-17.8582047356997,-1.18053383136164));
#37978=CARTESIAN_POINT('Ctrl Pts',(373.820978923856,-17.8560929931491,-1.21122479857131));
#37979=CARTESIAN_POINT('Ctrl Pts',(373.803605061511,-17.8532470790033,-1.25283520240953));
#37980=CARTESIAN_POINT('Ctrl Pts',(373.798902997843,-17.8524905226537,-1.26392147729961));
#37981=CARTESIAN_POINT('Ctrl Pts',(373.790912679704,-17.8512278199055,-1.28247069868622));
#37982=CARTESIAN_POINT('Ctrl Pts',(373.787658072661,-17.8507196851463,-1.28994791127096));
#37983=CARTESIAN_POINT('Ctrl Pts',(373.781418381097,-17.8497572653634,-1.30413572164383));
#37984=CARTESIAN_POINT('Ctrl Pts',(373.778438692717,-17.849302647879,-1.31084857510864));
#37985=CARTESIAN_POINT('Ctrl Pts',(373.771310236494,-17.8482266275866,-1.32676114935411));
#37986=CARTESIAN_POINT('Ctrl Pts',(373.767141124425,-17.8476064537096,-1.33595174801758));
#37987=CARTESIAN_POINT('Ctrl Pts',(373.752295274384,-17.8454294343591,-1.3682742401605));
#37988=CARTESIAN_POINT('Ctrl Pts',(373.741387172071,-17.8438859864404,-1.39129964200097));
#37989=CARTESIAN_POINT('Ctrl Pts',(373.636197315612,-17.8294946859269,-1.60670016403932));
#37990=CARTESIAN_POINT('Ctrl Pts',(373.523213188884,-17.8176247779347,-1.78938009521692));
#37991=CARTESIAN_POINT('Ctrl Pts',(373.257455177897,-17.7931791000757,-2.1363891967906));
#37992=CARTESIAN_POINT('Ctrl Pts',(373.104036478827,-17.7806386349199,-2.29872005507313));
#37993=CARTESIAN_POINT('Ctrl Pts',(372.911099012102,-17.7654259002684,-2.46456903345395));
#37994=CARTESIAN_POINT('Ctrl Pts',(372.886780802671,-17.7635185832077,-2.48485738749289));
#37995=CARTESIAN_POINT('Ctrl Pts',(372.84909412177,-17.7605759114643,-2.51536818698017));
#37996=CARTESIAN_POINT('Ctrl Pts',(372.835937584093,-17.7595510163357,-2.52585014690899));
#37997=CARTESIAN_POINT('Ctrl Pts',(372.811836523562,-17.7576775674519,-2.54474517693252));
#37998=CARTESIAN_POINT('Ctrl Pts',(372.800918797294,-17.756830379529,-2.55319188947021));
#37999=CARTESIAN_POINT('Ctrl Pts',(372.776976276307,-17.7549755315757,-2.57147080952233));
#38000=CARTESIAN_POINT('Ctrl Pts',(372.763930443029,-17.7539667908113,-2.58127470653681));
#38001=CARTESIAN_POINT('Ctrl Pts',(372.727900031589,-17.7511857674438,-2.60792564975395));
#38002=CARTESIAN_POINT('Ctrl Pts',(372.704766007083,-17.7494056114818,-2.62456725591072));
#38003=CARTESIAN_POINT('Ctrl Pts',(372.573798457109,-17.7393554033275,-2.7161685379367));
#38004=CARTESIAN_POINT('Ctrl Pts',(372.461695482452,-17.7308492103,-2.78477983918326));
#38005=CARTESIAN_POINT('Ctrl Pts',(372.152216154913,-17.7076472245125,-2.9491132722235));
#38006=CARTESIAN_POINT('Ctrl Pts',(371.948728804061,-17.692641303294,-3.03186442814594));
#38007=CARTESIAN_POINT('Ctrl Pts',(371.637790762505,-17.6709764271891,-3.12274655071335));
#38008=CARTESIAN_POINT('Ctrl Pts',(371.535747746345,-17.6640663585574,-3.1472393293699));
#38009=CARTESIAN_POINT('Ctrl Pts',(371.415703805194,-17.6562990364168,-3.16992216028446));
#38010=CARTESIAN_POINT('Ctrl Pts',(371.398699248294,-17.6552071638666,-3.17299382272355));
#38011=CARTESIAN_POINT('Ctrl Pts',(371.372508792167,-17.6535391992345,-3.17750759298088));
#38012=CARTESIAN_POINT('Ctrl Pts',(371.363340281956,-17.6529578760478,-3.17904691145144));
#38013=CARTESIAN_POINT('Ctrl Pts',(371.346436060333,-17.6518909909958,-3.18180983694083));
#38014=CARTESIAN_POINT('Ctrl Pts',(371.338702562616,-17.6514048118915,-3.18304492014342));
#38015=CARTESIAN_POINT('Ctrl Pts',(371.321144695166,-17.6503052835796,-3.18578341389902));
#38016=CARTESIAN_POINT('Ctrl Pts',(371.311317831575,-17.6496929080889,-3.1872695777252));
#38017=CARTESIAN_POINT('Ctrl Pts',(371.285764027622,-17.6481079433627,-3.19101337179345));
#38018=CARTESIAN_POINT('Ctrl Pts',(371.270026777515,-17.6471391758871,-3.19320023549246));
#38019=CARTESIAN_POINT('Ctrl Pts',(371.162223264578,-17.6405490738872,-3.20736889704702));
#38020=CARTESIAN_POINT('Ctrl Pts',(371.069683910013,-17.6351217352367,-3.21548493149783));
#38021=CARTESIAN_POINT('Ctrl Pts',(370.89497092361,-17.6250931827155,-3.22322303948595));
#38022=CARTESIAN_POINT('Ctrl Pts',(370.812915000222,-17.6204731452029,-3.22372276897205));
#38023=CARTESIAN_POINT('Ctrl Pts',(370.59828778088,-17.6084366279982,-3.21683362490853));
#38024=CARTESIAN_POINT('Ctrl Pts',(370.466039115849,-17.6010634035132,-3.20438743792046));
#38025=CARTESIAN_POINT('Ctrl Pts',(370.238247108365,-17.5880033552765,-3.16865842814046));
#38026=CARTESIAN_POINT('Ctrl Pts',(370.142304174231,-17.5823902094017,-3.14909693923421));
#38027=CARTESIAN_POINT('Ctrl Pts',(370.006711540312,-17.5741925626739,-3.11495526004104));
#38028=CARTESIAN_POINT('Ctrl Pts',(369.966223825611,-17.5717106375951,-3.10391543249087));
#38029=CARTESIAN_POINT('Ctrl Pts',(369.894288036021,-17.5672322257253,-3.08278307605368));
#38030=CARTESIAN_POINT('Ctrl Pts',(369.862757389896,-17.5652453452894,-3.07299165242911));
#38031=CARTESIAN_POINT('Ctrl Pts',(369.815133883546,-17.5622054729207,-3.05739659949721));
#38032=CARTESIAN_POINT('Ctrl Pts',(369.798927037312,-17.5611640629864,-3.05194622682745));
#38033=CARTESIAN_POINT('Ctrl Pts',(369.769580670656,-17.5592654367029,-3.04181636856075));
#38034=CARTESIAN_POINT('Ctrl Pts',(369.756426619538,-17.5584096655022,-3.03718003527179));
#38035=CARTESIAN_POINT('Ctrl Pts',(369.728117436705,-17.5565574994371,-3.02699498839624));
#38036=CARTESIAN_POINT('Ctrl Pts',(369.712973114192,-17.5555601670673,-3.02141754519029));
#38037=CARTESIAN_POINT('Ctrl Pts',(369.671948971665,-17.5528405125514,-3.00595800900626));
#38038=CARTESIAN_POINT('Ctrl Pts',(369.646154111898,-17.5511108769936,-2.99585577348444));
#38039=CARTESIAN_POINT('Ctrl Pts',(369.511670807134,-17.5419878780569,-2.94117703568361));
#38040=CARTESIAN_POINT('Ctrl Pts',(369.405361236193,-17.5344076589766,-2.89101972272695));
#38041=CARTESIAN_POINT('Ctrl Pts',(369.100207979186,-17.5115502347573,-2.7260985344978));
#38042=CARTESIAN_POINT('Ctrl Pts',(368.910612341183,-17.4958394940733,-2.5957833433018));
#38043=CARTESIAN_POINT('Ctrl Pts',(368.680121355113,-17.4755063573029,-2.39813829373268));
#38044=CARTESIAN_POINT('Ctrl Pts',(368.625443682218,-17.4705828018742,-2.34787267731464));
#38045=CARTESIAN_POINT('Ctrl Pts',(368.541914925819,-17.462959462446,-2.2655806277239));
#38046=CARTESIAN_POINT('Ctrl Pts',(368.511887106196,-17.4601967082233,-2.23478916354029));
#38047=CARTESIAN_POINT('Ctrl Pts',(368.473399270228,-17.4566367725319,-2.19370862359015));
#38048=CARTESIAN_POINT('Ctrl Pts',(368.464375436289,-17.4558007154867,-2.18395673846982));
#38049=CARTESIAN_POINT('Ctrl Pts',(368.449729970821,-17.4544419318746,-2.16793199424891));
#38050=CARTESIAN_POINT('Ctrl Pts',(368.444072271429,-17.4539165530998,-2.16169252280414));
#38051=CARTESIAN_POINT('Ctrl Pts',(368.433089187723,-17.4528958689476,-2.14948422688604));
#38052=CARTESIAN_POINT('Ctrl Pts',(368.427761483458,-17.4524003974966,-2.14351766647589));
#38053=CARTESIAN_POINT('Ctrl Pts',(368.414720051287,-17.4511865064303,-2.12880249813699));
#38054=CARTESIAN_POINT('Ctrl Pts',(368.407031400889,-17.4504699357884,-2.12003162411374));
#38055=CARTESIAN_POINT('Ctrl Pts',(368.380832281767,-17.4480242800004,-2.08981545373216));
#38056=CARTESIAN_POINT('Ctrl Pts',(368.362556463019,-17.4463114373808,-2.06816726455138));
#38057=CARTESIAN_POINT('Ctrl Pts',(368.138316755813,-17.4251682794733,-1.7953303082772));
#38058=CARTESIAN_POINT('Ctrl Pts',(367.971161677067,-17.4078836424248,-1.51460813668211));
#38059=CARTESIAN_POINT('Ctrl Pts',(367.804805783727,-17.382611375939,-1.10536121641511));
#38060=CARTESIAN_POINT('Ctrl Pts',(367.766733022571,-17.3757999892202,-0.994829521371667));
#38061=CARTESIAN_POINT('Ctrl Pts',(367.727371254028,-17.3671716546808,-0.856577987980679));
#38062=CARTESIAN_POINT('Ctrl Pts',(367.720321072374,-17.3655448668063,-0.830582326898628));
#38063=CARTESIAN_POINT('Ctrl Pts',(367.709650907161,-17.3629464395477,-0.789191998261899));
#38064=CARTESIAN_POINT('Ctrl Pts',(367.705816875335,-17.3619817232031,-0.773853443073163));
#38065=CARTESIAN_POINT('Ctrl Pts',(367.698805235388,-17.3601569824079,-0.744898434275763));
#38066=CARTESIAN_POINT('Ctrl Pts',(367.695603065259,-17.3592977719579,-0.731288263296041));
#38067=CARTESIAN_POINT('Ctrl Pts',(367.688579399558,-17.3573530286158,-0.70053941658764));
#38068=CARTESIAN_POINT('Ctrl Pts',(367.684809233268,-17.3562658776419,-0.683389586071041));
#38069=CARTESIAN_POINT('Ctrl Pts',(367.675483915894,-17.3534612699564,-0.639253333006067));
#38070=CARTESIAN_POINT('Ctrl Pts',(367.67013443683,-17.3517373288029,-0.612225366257496));
#38071=CARTESIAN_POINT('Ctrl Pts',(367.629312528714,-17.3375790029011,-0.391126490720944));
#38072=CARTESIAN_POINT('Ctrl Pts',(367.611388699999,-17.3245840805187,-0.194274640082018));
#38073=CARTESIAN_POINT('Ctrl Pts',(367.611756317698,-17.2975526701401,0.207397995299695));
#38074=CARTESIAN_POINT('Ctrl Pts',(367.631397625581,-17.2835589428912,0.411367515210719));
#38075=CARTESIAN_POINT('Ctrl Pts',(367.680579773175,-17.2665934771642,0.665599276409641));
#38076=CARTESIAN_POINT('Ctrl Pts',(367.692284086745,-17.2630710855992,0.718826047744092));
#38077=CARTESIAN_POINT('Ctrl Pts',(367.708940487933,-17.2586611938674,0.786359205967593));
#38078=CARTESIAN_POINT('Ctrl Pts',(367.712650277796,-17.2577113791877,0.800959453061964));
#38079=CARTESIAN_POINT('Ctrl Pts',(367.718693296946,-17.2562146856849,0.824062441180066));
#38080=CARTESIAN_POINT('Ctrl Pts',(367.720959225455,-17.2556640927977,0.832582333418417));
#38081=CARTESIAN_POINT('Ctrl Pts',(367.725325752797,-17.2546230601939,0.848733365040112));
#38082=CARTESIAN_POINT('Ctrl Pts',(367.72741948144,-17.2541322640714,0.856365992984681));
#38083=CARTESIAN_POINT('Ctrl Pts',(367.732412322328,-17.2529811997489,0.874307908959234));
#38084=CARTESIAN_POINT('Ctrl Pts',(367.735334727508,-17.2523222807221,0.884610556343805));
#38085=CARTESIAN_POINT('Ctrl Pts',(367.745128867118,-17.2501613579301,0.918494560075191));
#38086=CARTESIAN_POINT('Ctrl Pts',(367.752219016763,-17.2486713882148,0.942012576382163));
#38087=CARTESIAN_POINT('Ctrl Pts',(367.793068157957,-17.2404724321887,1.07210813275743));
#38088=CARTESIAN_POINT('Ctrl Pts',(367.832089524263,-17.2340245788628,1.17696459774762));
#38089=CARTESIAN_POINT('Ctrl Pts',(367.994451570116,-17.2108341043497,1.55227199535719));
#38090=CARTESIAN_POINT('Ctrl Pts',(368.149546398421,-17.1947082962738,1.8073165771048));
#38091=CARTESIAN_POINT('Ctrl Pts',(368.369696370391,-17.1741710836258,2.07710621084808));
#38092=CARTESIAN_POINT('Ctrl Pts',(368.402942043159,-17.1711235540913,2.11592544849935));
#38093=CARTESIAN_POINT('Ctrl Pts',(368.451061991343,-17.1667767712337,2.16948052544261));
#38094=CARTESIAN_POINT('Ctrl Pts',(368.465179273883,-17.165508970542,2.18488823825482));
#38095=CARTESIAN_POINT('Ctrl Pts',(368.488364251498,-17.1634382307613,2.20970358716528));
#38096=CARTESIAN_POINT('Ctrl Pts',(368.497341213578,-17.1626391743246,2.21919544484741));
#38097=CARTESIAN_POINT('Ctrl Pts',(368.516280450613,-17.1609588428651,2.23897863220294));
#38098=CARTESIAN_POINT('Ctrl Pts',(368.52625409672,-17.1600770840736,2.24925863358192));
#38099=CARTESIAN_POINT('Ctrl Pts',(368.550240660873,-17.157963663427,2.27365444860545));
#38100=CARTESIAN_POINT('Ctrl Pts',(368.564316250548,-17.156729258969,2.28770755728963));
#38101=CARTESIAN_POINT('Ctrl Pts',(368.613062650418,-17.1524732593598,2.33548327426032));
#38102=CARTESIAN_POINT('Ctrl Pts',(368.648360640956,-17.1494237035336,2.36855387511503));
#38103=CARTESIAN_POINT('Ctrl Pts',(368.794694906472,-17.1369032868009,2.49959614354931));
#38104=CARTESIAN_POINT('Ctrl Pts',(368.91166430413,-17.1271600299159,2.59064394632193));
#38105=CARTESIAN_POINT('Ctrl Pts',(369.185238553045,-17.1050566465925,2.77483199317565));
#38106=CARTESIAN_POINT('Ctrl Pts',(369.344326446425,-17.0926381768084,2.86340343563949));
#38107=CARTESIAN_POINT('Ctrl Pts',(369.596220774644,-17.0742120008577,2.97693990324591));
#38108=CARTESIAN_POINT('Ctrl Pts',(369.684087726991,-17.0680011140411,3.01198102555866));
#38109=CARTESIAN_POINT('Ctrl Pts',(369.788443786333,-17.0609710397771,3.04836343364431));
#38110=CARTESIAN_POINT('Ctrl Pts',(369.803550462248,-17.0599616954946,3.05350467448696));
#38111=CARTESIAN_POINT('Ctrl Pts',(369.828146749709,-17.0583325213329,3.06167216697092));
#38112=CARTESIAN_POINT('Ctrl Pts',(369.837613092478,-17.0577089034025,3.0647669362743));
#38113=CARTESIAN_POINT('Ctrl Pts',(369.854550052235,-17.0565993984479,3.07021725158917));
#38114=CARTESIAN_POINT('Ctrl Pts',(369.862015044824,-17.0561125577271,3.07258948912748));
#38115=CARTESIAN_POINT('Ctrl Pts',(369.878343644799,-17.0550524288006,3.07771294987256));
#38116=CARTESIAN_POINT('Ctrl Pts',(369.887210511191,-17.0544797841385,3.08045311223727));
#38117=CARTESIAN_POINT('Ctrl Pts',(369.912546848122,-17.0528518171205,3.08816316151229));
#38118=CARTESIAN_POINT('Ctrl Pts',(369.929044727598,-17.0518017598808,3.09303962079563));
#38119=CARTESIAN_POINT('Ctrl Pts',(370.044350253084,-17.04452726393,3.12612012043599));
#38120=CARTESIAN_POINT('Ctrl Pts',(370.144428580246,-17.0385418272147,3.14971951048712));
#38121=CARTESIAN_POINT('Ctrl Pts',(370.388709111282,-17.0243477330293,3.1951174534242));
#38122=CARTESIAN_POINT('Ctrl Pts',(370.533590594242,-17.0162661444774,3.21199457798821));
#38123=CARTESIAN_POINT('Ctrl Pts',(370.883060434138,-16.9966680405207,3.22884336333444));
#38124=CARTESIAN_POINT('Ctrl Pts',(371.087444345024,-16.9850959737636,3.2192727689767));
#38125=CARTESIAN_POINT('Ctrl Pts',(371.316663332644,-16.9712379720792,3.18656731558649));
#38126=CARTESIAN_POINT('Ctrl Pts',(371.343739220006,-16.9695876342822,3.18235105223757));
#38127=CARTESIAN_POINT('Ctrl Pts',(371.388027066876,-16.9668646948732,3.17487486494676));
#38128=CARTESIAN_POINT('Ctrl Pts',(371.405272371843,-16.9657985413286,3.17181891352475));
#38129=CARTESIAN_POINT('Ctrl Pts',(371.43623459049,-16.9638734507462,3.16607156899831));
#38130=CARTESIAN_POINT('Ctrl Pts',(371.449960613528,-16.9630161555497,3.16343119422142));
#38131=CARTESIAN_POINT('Ctrl Pts',(371.479203946042,-16.9611812253746,3.15760833501188));
#38132=CARTESIAN_POINT('Ctrl Pts',(371.494715791472,-16.9602028039494,3.15440057996654));
#38133=CARTESIAN_POINT('Ctrl Pts',(371.53667114559,-16.957542305202,3.14540143720601));
#38134=CARTESIAN_POINT('Ctrl Pts',(371.56306589521,-16.9558532742018,3.13939111420503));
#38135=CARTESIAN_POINT('Ctrl Pts',(371.705059756929,-16.9466820864274,3.10517066284102));
#38136=CARTESIAN_POINT('Ctrl Pts',(371.819092226175,-16.9390070957941,3.07091028896699));
#38137=CARTESIAN_POINT('Ctrl Pts',(372.060678684937,-16.9220784159541,2.9834857840475));
#38138=CARTESIAN_POINT('Ctrl Pts',(372.187224989695,-16.9127845441374,2.92827176954826));
#38139=CARTESIAN_POINT('Ctrl Pts',(372.309820641399,-16.9034565314269,2.86513683522936));
#38140=CARTESIAN_POINT('',(367.611567912033,-17.0672029561653,-0.000615672028770192));
#38141=CARTESIAN_POINT('Ctrl Pts',(372.309820496378,-16.659489044147,2.86513690991278));
#38142=CARTESIAN_POINT('Ctrl Pts',(372.262650708085,-16.6629935624819,2.88942864517458));
#38143=CARTESIAN_POINT('Ctrl Pts',(372.214871312371,-16.6664605937869,2.91256053053015));
#38144=CARTESIAN_POINT('Ctrl Pts',(372.141992305273,-16.671602854912,2.94564610246232));
#38145=CARTESIAN_POINT('Ctrl Pts',(372.117320350931,-16.6733189975538,2.95647562724856));
#38146=CARTESIAN_POINT('Ctrl Pts',(372.083005338726,-16.6756690614488,2.97102740022174));
#38147=CARTESIAN_POINT('Ctrl Pts',(372.073476620043,-16.6763177432156,2.97501425320145));
#38148=CARTESIAN_POINT('Ctrl Pts',(372.057080114797,-16.6774270829223,2.98178216997762));
#38149=CARTESIAN_POINT('Ctrl Pts',(372.050221672257,-16.6778890488854,2.98458545915616));
#38150=CARTESIAN_POINT('Ctrl Pts',(372.035844558692,-16.6788530604544,2.99040411298314));
#38151=CARTESIAN_POINT('Ctrl Pts',(372.028324103031,-16.6793548065152,2.99341481590983));
#38152=CARTESIAN_POINT('Ctrl Pts',(372.009866088416,-16.6805803069624,3.0007235810072));
#38153=CARTESIAN_POINT('Ctrl Pts',(371.998916083265,-16.6813022022125,3.00499028873532));
#38154=CARTESIAN_POINT('Ctrl Pts',(371.958999122469,-16.6839160543264,3.02029310874339));
#38155=CARTESIAN_POINT('Ctrl Pts',(371.929895653298,-16.6857879744324,3.03097143922983));
#38156=CARTESIAN_POINT('Ctrl Pts',(371.856368790584,-16.6904433224381,3.05675162136396));
#38157=CARTESIAN_POINT('Ctrl Pts',(371.811760227619,-16.6932007740934,3.07130679575183));
#38158=CARTESIAN_POINT('Ctrl Pts',(371.443406119834,-16.7155450849012,3.1826566025822));
#38159=CARTESIAN_POINT('Ctrl Pts',(371.106594318805,-16.7335378055608,3.22896227462198));
#38160=CARTESIAN_POINT('Ctrl Pts',(370.706189162994,-16.7570025275489,3.22080903927003));
#38161=CARTESIAN_POINT('Ctrl Pts',(370.643723679882,-16.7607142270674,3.21771672472883));
#38162=CARTESIAN_POINT('Ctrl Pts',(370.558803700995,-16.7658476300432,3.21103142973763));
#38163=CARTESIAN_POINT('Ctrl Pts',(370.536236670781,-16.7672202068724,3.20901518527397));
#38164=CARTESIAN_POINT('Ctrl Pts',(370.500360748185,-16.7694163899799,3.20542816889744));
#38165=CARTESIAN_POINT('Ctrl Pts',(370.487036892193,-16.7702351313492,3.20401201926006));
#38166=CARTESIAN_POINT('Ctrl Pts',(370.459690769202,-16.7719220881224,3.20093290988067));
#38167=CARTESIAN_POINT('Ctrl Pts',(370.44566984396,-16.7727905743016,3.19926079906817));
#38168=CARTESIAN_POINT('Ctrl Pts',(370.413185603054,-16.7748111498907,3.19517009347095));
#38169=CARTESIAN_POINT('Ctrl Pts',(370.394731501116,-16.7759653575872,3.19268352864213));
#38170=CARTESIAN_POINT('Ctrl Pts',(370.335835132856,-16.7796697886667,3.18422733541922));
#38171=CARTESIAN_POINT('Ctrl Pts',(370.295485767457,-16.7822390895788,3.177648262919));
#38172=CARTESIAN_POINT('Ctrl Pts',(370.201007904746,-16.7883316549126,3.16039223939409));
#38173=CARTESIAN_POINT('Ctrl Pts',(370.147008117449,-16.791873579666,3.14908960577615));
#38174=CARTESIAN_POINT('Ctrl Pts',(369.946950222638,-16.80521923053,3.10182502334244));
#38175=CARTESIAN_POINT('Ctrl Pts',(369.803188308791,-16.8152695799673,3.05704156139889));
#38176=CARTESIAN_POINT('Ctrl Pts',(369.460642174878,-16.840094972195,2.92341508949743));
#38177=CARTESIAN_POINT('Ctrl Pts',(369.26668564817,-16.8549393966478,2.82416070148185));
#38178=CARTESIAN_POINT('Ctrl Pts',(369.063066496116,-16.8704934669863,2.69247446804024));
#38179=CARTESIAN_POINT('Ctrl Pts',(369.042107199391,-16.8720935828904,2.67856887046183));
#38180=CARTESIAN_POINT('Ctrl Pts',(369.013010656927,-16.8743112548417,2.65877010694048));
#38181=CARTESIAN_POINT('Ctrl Pts',(369.00473551571,-16.8749415449182,2.6530825206512));
#38182=CARTESIAN_POINT('Ctrl Pts',(368.990461450957,-16.8760278299444,2.64317326987093));
#38183=CARTESIAN_POINT('Ctrl Pts',(368.984450164862,-16.8764850152884,2.6389696672845));
#38184=CARTESIAN_POINT('Ctrl Pts',(368.971925758133,-16.8774368647073,2.63014771338083));
#38185=CARTESIAN_POINT('Ctrl Pts',(368.965415352056,-16.8779312566451,2.62552561473488));
#38186=CARTESIAN_POINT('Ctrl Pts',(368.949377502307,-16.8791483489555,2.61404957514139));
#38187=CARTESIAN_POINT('Ctrl Pts',(368.939870086883,-16.8798691521744,2.60716761607293));
#38188=CARTESIAN_POINT('Ctrl Pts',(368.919403109872,-16.8814198309935,2.59218148776407));
#38189=CARTESIAN_POINT('Ctrl Pts',(368.908456890568,-16.882248530284,2.58405938529645));
#38190=CARTESIAN_POINT('Ctrl Pts',(368.877524678459,-16.8845895054829,2.56080193004355));
#38191=CARTESIAN_POINT('Ctrl Pts',(368.857662877341,-16.8860917153746,2.54550215868964));
#38192=CARTESIAN_POINT('Ctrl Pts',(368.790781951608,-16.8911545437106,2.49272810742424));
#38193=CARTESIAN_POINT('Ctrl Pts',(368.74463159088,-16.8946557137532,2.45416881047839));
#38194=CARTESIAN_POINT('Ctrl Pts',(368.473097825576,-16.9154859910744,2.21408147750278));
#38195=CARTESIAN_POINT('Ctrl Pts',(368.275914163258,-16.9317540681465,1.98295407454614));
#38196=CARTESIAN_POINT('Ctrl Pts',(368.074281504201,-16.9536608277038,1.66545987109065));
#38197=CARTESIAN_POINT('Ctrl Pts',(368.03689325041,-16.9580202953467,1.60186503628977));
#38198=CARTESIAN_POINT('Ctrl Pts',(367.990227832369,-16.9639084551325,1.51586616965014));
#38199=CARTESIAN_POINT('Ctrl Pts',(367.978972649988,-16.9653667830668,1.494557463995));
#38200=CARTESIAN_POINT('Ctrl Pts',(367.961010735384,-16.9677585880796,1.45960773681184));
#38201=CARTESIAN_POINT('Ctrl Pts',(367.954159544919,-16.9686869629579,1.44604171637026));
#38202=CARTESIAN_POINT('Ctrl Pts',(367.941117647913,-16.970485911897,1.41975709571559));
#38203=CARTESIAN_POINT('Ctrl Pts',(367.934914208457,-16.9713560152189,1.40704517817393));
#38204=CARTESIAN_POINT('Ctrl Pts',(367.920667614035,-16.9733884946347,1.37735715012612));
#38205=CARTESIAN_POINT('Ctrl Pts',(367.912688868128,-16.9745530678839,1.36035086827977));
#38206=CARTESIAN_POINT('Ctrl Pts',(367.887439612811,-16.9783253268818,1.30528650333673));
#38207=CARTESIAN_POINT('Ctrl Pts',(367.870761162794,-16.9809530857138,1.26696317971802));
#38208=CARTESIAN_POINT('Ctrl Pts',(367.83319658768,-16.9872090820167,1.17584493234048));
#38209=CARTESIAN_POINT('Ctrl Pts',(367.812951534621,-16.9908573621093,1.12280234002851));
#38210=CARTESIAN_POINT('Ctrl Pts',(367.741722098781,-17.0048111140382,0.920276643044859));
#38211=CARTESIAN_POINT('Ctrl Pts',(367.700352129991,-17.0153885726118,0.76766326205813));
#38212=CARTESIAN_POINT('Ctrl Pts',(367.631209677124,-17.0399686176423,0.410581857261768));
#38213=CARTESIAN_POINT('Ctrl Pts',(367.611528588751,-17.053991323043,0.205222988379962));
#38214=CARTESIAN_POINT('Ctrl Pts',(367.611567912033,-17.0672029561653,-0.000615672028770192));
#38215=CARTESIAN_POINT('Ctrl Pts',(367.611567912602,-17.0672031470406,-0.00061864588800962));
#38216=CARTESIAN_POINT('Ctrl Pts',(367.611570957118,-17.0682211099538,-0.0164786273153796));
#38217=CARTESIAN_POINT('Ctrl Pts',(367.611691078271,-17.0692338931669,-0.0323387716768588));
#38218=CARTESIAN_POINT('Ctrl Pts',(367.612138722679,-17.0711344453491,-0.0622672202399708));
#38219=CARTESIAN_POINT('Ctrl Pts',(367.612441307727,-17.072023403668,-0.076335432346843));
#38220=CARTESIAN_POINT('Ctrl Pts',(367.613056974207,-17.0734023779987,-0.0982748725629377));
#38221=CARTESIAN_POINT('Ctrl Pts',(367.613306783411,-17.0738957229655,-0.106147503405766));
#38222=CARTESIAN_POINT('Ctrl Pts',(367.613851155909,-17.0748563448645,-0.121524541521579));
#38223=CARTESIAN_POINT('Ctrl Pts',(367.614143093733,-17.0753237617378,-0.12902901098511));
#38224=CARTESIAN_POINT('Ctrl Pts',(367.614827398663,-17.0763258391311,-0.145167017576318));
#38225=CARTESIAN_POINT('Ctrl Pts',(367.615228262234,-17.076860022709,-0.153800062710141));
#38226=CARTESIAN_POINT('Ctrl Pts',(367.616382604606,-17.0782706427935,-0.17667388015715));
#38227=CARTESIAN_POINT('Ctrl Pts',(367.617195895314,-17.0791438146921,-0.190911627513823));
#38228=CARTESIAN_POINT('Ctrl Pts',(367.621107655103,-17.0828857601728,-0.2522396163173));
#38229=CARTESIAN_POINT('Ctrl Pts',(367.625145896418,-17.0857063948571,-0.299266566907833));
#38230=CARTESIAN_POINT('Ctrl Pts',(367.662099032802,-17.1059737394695,-0.641279429069706));
#38231=CARTESIAN_POINT('Ctrl Pts',(367.734595054949,-17.1218983053493,-0.930576127672779));
#38232=CARTESIAN_POINT('Ctrl Pts',(367.89059535041,-17.1457207982213,-1.31720314357685));
#38233=CARTESIAN_POINT('Ctrl Pts',(367.941690097384,-17.152711835624,-1.42591245093985));
#38234=CARTESIAN_POINT('Ctrl Pts',(368.011625526135,-17.1615437755249,-1.55539788589501));
#38235=CARTESIAN_POINT('Ctrl Pts',(368.024827587978,-17.1631832237465,-1.57911967181968));
#38236=CARTESIAN_POINT('Ctrl Pts',(368.046216795702,-17.1657976701473,-1.61643488371139));
#38237=CARTESIAN_POINT('Ctrl Pts',(368.054207536525,-17.1667656029413,-1.63013982625584));
#38238=CARTESIAN_POINT('Ctrl Pts',(368.069432953017,-17.1685938218349,-1.65581541066522));
#38239=CARTESIAN_POINT('Ctrl Pts',(368.076645026661,-17.1694532709602,-1.6677990758605));
#38240=CARTESIAN_POINT('Ctrl Pts',(368.093060422651,-17.1713950574803,-1.6946774941438));
#38241=CARTESIAN_POINT('Ctrl Pts',(368.102307522788,-17.1724789851461,-1.70954486482611));
#38242=CARTESIAN_POINT('Ctrl Pts',(368.126314836691,-17.175268356208,-1.74745124779751));
#38243=CARTESIAN_POINT('Ctrl Pts',(368.141247911939,-17.1769801591818,-1.77037860870688));
#38244=CARTESIAN_POINT('Ctrl Pts',(368.271494725808,-17.1917189099354,-1.96489013794532));
#38245=CARTESIAN_POINT('Ctrl Pts',(368.402759537296,-17.205365686685,-2.12517111702655));
#38246=CARTESIAN_POINT('Ctrl Pts',(368.651990502347,-17.2291920824747,-2.37595113128453));
#38247=CARTESIAN_POINT('Ctrl Pts',(368.762543333597,-17.2391926531057,-2.47294309358282));
#38248=CARTESIAN_POINT('Ctrl Pts',(368.932572722941,-17.2534719468017,-2.60268491932549));
#38249=CARTESIAN_POINT('Ctrl Pts',(368.987074884175,-17.2578984733887,-2.64164680296096));
#38250=CARTESIAN_POINT('Ctrl Pts',(369.065175067175,-17.2639946059058,-2.69387803304517));
#38251=CARTESIAN_POINT('Ctrl Pts',(369.087783503371,-17.2657313259898,-2.70859057811791));
#38252=CARTESIAN_POINT('Ctrl Pts',(369.122693706617,-17.2683673846775,-2.73068966860798));
#38253=CARTESIAN_POINT('Ctrl Pts',(369.134863997648,-17.2692779991825,-2.73828046322356));
#38254=CARTESIAN_POINT('Ctrl Pts',(369.155069719111,-17.2707755590437,-2.75069647539726));
#38255=CARTESIAN_POINT('Ctrl Pts',(369.163076108545,-17.2713652836882,-2.75556825928215));
#38256=CARTESIAN_POINT('Ctrl Pts',(369.178590250877,-17.2725007510968,-2.76491592356747));
#38257=CARTESIAN_POINT('Ctrl Pts',(369.186095176108,-17.2730467745846,-2.7693963184189));
#38258=CARTESIAN_POINT('Ctrl Pts',(369.200112346615,-17.2740604111612,-2.77768732061275));
#38259=CARTESIAN_POINT('Ctrl Pts',(369.206619690619,-17.2745284981946,-2.78150556022892));
#38260=CARTESIAN_POINT('Ctrl Pts',(369.221869653992,-17.2756197465412,-2.79038176201841));
#38261=CARTESIAN_POINT('Ctrl Pts',(369.230622697484,-17.2762417359791,-2.79542151148647));
#38262=CARTESIAN_POINT('Ctrl Pts',(369.253981461589,-17.2778904370138,-2.80872498806493));
#38263=CARTESIAN_POINT('Ctrl Pts',(369.26862849445,-17.2789126976185,-2.81691604923042));
#38264=CARTESIAN_POINT('Ctrl Pts',(369.395504761955,-17.2876744336074,-2.88657371442765));
#38265=CARTESIAN_POINT('Ctrl Pts',(369.511252215524,-17.2950431499279,-2.94142753055836));
#38266=CARTESIAN_POINT('Ctrl Pts',(369.755685715311,-17.3099559672069,-3.0399080259698));
#38267=CARTESIAN_POINT('Ctrl Pts',(369.884475764445,-17.3174721576643,-3.08257839165419));
#38268=CARTESIAN_POINT('Ctrl Pts',(370.180477252832,-17.3346536825963,-3.16032910483207));
#38269=CARTESIAN_POINT('Ctrl Pts',(370.34854102955,-17.3443548904515,-3.19048568180492));
#38270=CARTESIAN_POINT('Ctrl Pts',(370.558603406045,-17.3568949861004,-3.21119108833059));
#38271=CARTESIAN_POINT('Ctrl Pts',(370.599086902747,-17.3593294714796,-3.21441018537751));
#38272=CARTESIAN_POINT('Ctrl Pts',(370.658156874634,-17.3629120748944,-3.21798536042964));
#38273=CARTESIAN_POINT('Ctrl Pts',(370.676703688881,-17.3640412909574,-3.21894706746407));
#38274=CARTESIAN_POINT('Ctrl Pts',(370.70935749729,-17.3660374839419,-3.22035737973027));
#38275=CARTESIAN_POINT('Ctrl Pts',(370.723461178377,-17.3669023192771,-3.22087372173741));
#38276=CARTESIAN_POINT('Ctrl Pts',(370.750976167829,-17.3685948790892,-3.22170012218377));
#38277=CARTESIAN_POINT('Ctrl Pts',(370.764386933254,-17.3694223056793,-3.22201911408936));
#38278=CARTESIAN_POINT('Ctrl Pts',(370.80053399765,-17.371659387394,-3.22265313777134));
#38279=CARTESIAN_POINT('Ctrl Pts',(370.823271955808,-17.3730739144129,-3.22281127912992));
#38280=CARTESIAN_POINT('Ctrl Pts',(370.909124649413,-17.3784434197128,-3.22249982387998));
#38281=CARTESIAN_POINT('Ctrl Pts',(370.972215863131,-17.3824481121993,-3.22041680755756));
#38282=CARTESIAN_POINT('Ctrl Pts',(371.3718192139,-17.4082000183046,-3.19545975670053));
#38283=CARTESIAN_POINT('Ctrl Pts',(371.702956587845,-17.4315913740504,-3.12173925962892));
#38284=CARTESIAN_POINT('Ctrl Pts',(372.060220880805,-17.4569422422504,-2.98085186165981));
#38285=CARTESIAN_POINT('Ctrl Pts',(372.103461516991,-17.4600068931505,-2.96269992769949));
#38286=CARTESIAN_POINT('Ctrl Pts',(372.174593463969,-17.4650251082468,-2.93099622797123));
#38287=CARTESIAN_POINT('Ctrl Pts',(372.202712074826,-17.4670026391745,-2.91797447221289));
#38288=CARTESIAN_POINT('Ctrl Pts',(372.241229225719,-17.4696985532576,-2.89945788155222));
#38289=CARTESIAN_POINT('Ctrl Pts',(372.25179104359,-17.4704364438616,-2.89430913718401));
#38290=CARTESIAN_POINT('Ctrl Pts',(372.269586213686,-17.4716770875192,-2.88551345664637));
#38291=CARTESIAN_POINT('Ctrl Pts',(372.276834344788,-17.4721816789811,-2.88189683224231));
#38292=CARTESIAN_POINT('Ctrl Pts',(372.290686401712,-17.4731445013185,-2.87491967099586));
#38293=CARTESIAN_POINT('Ctrl Pts',(372.297292455,-17.473603017721,-2.87156364736597));
#38294=CARTESIAN_POINT('Ctrl Pts',(372.313080913513,-17.4746974426093,-2.8634741300774));
#38295=CARTESIAN_POINT('Ctrl Pts',(372.32225231543,-17.4753320242106,-2.85871917561391));
#38296=CARTESIAN_POINT('Ctrl Pts',(372.355269753859,-17.477612913445,-2.84139919359176));
#38297=CARTESIAN_POINT('Ctrl Pts',(372.378981538499,-17.4792440896457,-2.82857884255323));
#38298=CARTESIAN_POINT('Ctrl Pts',(372.548405847168,-17.490869591487,-2.73420948188425));
#38299=CARTESIAN_POINT('Ctrl Pts',(372.687764411577,-17.5002813403914,-2.64173211187344));
#38300=CARTESIAN_POINT('Ctrl Pts',(372.942702201732,-17.5184052891386,-2.44240742459958));
#38301=CARTESIAN_POINT('Ctrl Pts',(373.058868420832,-17.5271031772986,-2.33709461935308));
#38302=CARTESIAN_POINT('Ctrl Pts',(373.249167487908,-17.5428664953261,-2.1374817241649));
#38303=CARTESIAN_POINT('Ctrl Pts',(373.326561631098,-17.5498108484044,-2.04671523926428));
#38304=CARTESIAN_POINT('Ctrl Pts',(373.415156990239,-17.5585900845478,-1.93031632678799));
#38305=CARTESIAN_POINT('Ctrl Pts',(373.43129505862,-17.5602264871636,-1.9085494751868));
#38306=CARTESIAN_POINT('Ctrl Pts',(373.456436743717,-17.5628371881133,-1.87372927866225));
#38307=CARTESIAN_POINT('Ctrl Pts',(373.465622017144,-17.5638044562273,-1.86080822990685));
#38308=CARTESIAN_POINT('Ctrl Pts',(373.482731740458,-17.5656321103684,-1.83635974401741));
#38309=CARTESIAN_POINT('Ctrl Pts',(373.490677222235,-17.5664916651961,-1.82484742387543));
#38310=CARTESIAN_POINT('Ctrl Pts',(373.508408103083,-17.5684346188864,-1.79879571891066));
#38311=CARTESIAN_POINT('Ctrl Pts',(373.518150294236,-17.5695196160096,-1.78422759532211));
#38312=CARTESIAN_POINT('Ctrl Pts',(373.542827532757,-17.5723135818269,-1.74666670538541));
#38313=CARTESIAN_POINT('Ctrl Pts',(373.557588625952,-17.5740289455973,-1.72356186068839));
#38314=CARTESIAN_POINT('Ctrl Pts',(373.68123918879,-17.5887860097614,-1.52446286166184));
#38315=CARTESIAN_POINT('Ctrl Pts',(373.773217809876,-17.6024488708771,-1.33857669212179));
#38316=CARTESIAN_POINT('Ctrl Pts',(373.925633105795,-17.6313549520017,-0.937649155496241));
#38317=CARTESIAN_POINT('Ctrl Pts',(373.982875888344,-17.6465623976405,-0.722501540273425));
#38318=CARTESIAN_POINT('Ctrl Pts',(374.022776003527,-17.6630631548155,-0.470079244576507));
#38319=CARTESIAN_POINT('Ctrl Pts',(374.027490475314,-17.6652044765469,-0.436908095776338));
#38320=CARTESIAN_POINT('Ctrl Pts',(374.033203981388,-17.6680837102208,-0.391652616151649));
#38321=CARTESIAN_POINT('Ctrl Pts',(374.034653209938,-17.6688446606219,-0.379628566137522));
#38322=CARTESIAN_POINT('Ctrl Pts',(374.036966895449,-17.6701129014934,-0.35947666703041));
#38323=CARTESIAN_POINT('Ctrl Pts',(374.037868265382,-17.6706222138474,-0.351353273828388));
#38324=CARTESIAN_POINT('Ctrl Pts',(374.039520386064,-17.6715855169474,-0.335928790195689));
#38325=CARTESIAN_POINT('Ctrl Pts',(374.040277113279,-17.6720398496192,-0.328628443722183));
#38326=CARTESIAN_POINT('Ctrl Pts',(374.042011723599,-17.6731135243446,-0.3113177741166));
#38327=CARTESIAN_POINT('Ctrl Pts',(374.042967704247,-17.6737316527555,-0.301305264299879));
#38328=CARTESIAN_POINT('Ctrl Pts',(374.046158364721,-17.6758924354209,-0.266148983439942));
#38329=CARTESIAN_POINT('Ctrl Pts',(374.048144560642,-17.6774219602216,-0.240982855618438));
#38330=CARTESIAN_POINT('Ctrl Pts',(374.064485526612,-17.692076590735,0.00251039764335815));
#38331=CARTESIAN_POINT('Ctrl Pts',(374.056868616474,-17.7041795515152,0.221771927720396));
#38332=CARTESIAN_POINT('Ctrl Pts',(374.006773978729,-17.7247707915569,0.586438806639206));
#38333=CARTESIAN_POINT('Ctrl Pts',(373.976220623224,-17.7331540235787,0.732687411003659));
#38334=CARTESIAN_POINT('Ctrl Pts',(373.920717203207,-17.7449995364376,0.929124077846322));
#38335=CARTESIAN_POINT('Ctrl Pts',(373.904439967954,-17.7482199173833,0.981571301054406));
#38336=CARTESIAN_POINT('Ctrl Pts',(373.873767628938,-17.7539012191369,1.07215758850318));
#38337=CARTESIAN_POINT('Ctrl Pts',(373.859973838216,-17.7563430556571,1.11048749201427));
#38338=CARTESIAN_POINT('Ctrl Pts',(373.838830925856,-17.7599344988351,1.16591788336398));
#38339=CARTESIAN_POINT('Ctrl Pts',(373.8320540067,-17.7610650687459,1.18323338612762));
#38340=CARTESIAN_POINT('Ctrl Pts',(373.81986928966,-17.7630628130109,1.21358949282197));
#38341=CARTESIAN_POINT('Ctrl Pts',(373.814524896591,-17.7639278348604,1.22665512893726));
#38342=CARTESIAN_POINT('Ctrl Pts',(373.803937549914,-17.7656201216009,1.25206077161786));
#38343=CARTESIAN_POINT('Ctrl Pts',(373.798703082882,-17.7664470844208,1.26440401783152));
#38344=CARTESIAN_POINT('Ctrl Pts',(373.784398860316,-17.7686813277719,1.29755729202507));
#38345=CARTESIAN_POINT('Ctrl Pts',(373.775186129058,-17.7700934581313,1.31830444751966));
#38346=CARTESIAN_POINT('Ctrl Pts',(373.739645163729,-17.7754434363473,1.39611612572322));
#38347=CARTESIAN_POINT('Ctrl Pts',(373.711870267672,-17.7794305350366,1.4525006832974));
#38348=CARTESIAN_POINT('Ctrl Pts',(373.52448889745,-17.8051826665246,1.80639845349481));
#38349=CARTESIAN_POINT('Ctrl Pts',(373.320661075031,-17.8285973427458,2.07800650840981));
#38350=CARTESIAN_POINT('Ctrl Pts',(373.044782431174,-17.8539712184178,2.34566911183202));
#38351=CARTESIAN_POINT('Ctrl Pts',(373.010410543838,-17.8570367148681,2.3775908566064));
#38352=CARTESIAN_POINT('Ctrl Pts',(372.95218938131,-17.8620561602466,2.4293410982708));
#38353=CARTESIAN_POINT('Ctrl Pts',(372.928729540129,-17.8640340899359,2.44959544254447));
#38354=CARTESIAN_POINT('Ctrl Pts',(372.895976042751,-17.8667304525125,2.47705897141263));
#38355=CARTESIAN_POINT('Ctrl Pts',(372.886930502134,-17.8674684011147,2.48455971187591));
#38356=CARTESIAN_POINT('Ctrl Pts',(372.871580342513,-17.8687091138961,2.49714731797277));
#38357=CARTESIAN_POINT('Ctrl Pts',(372.865297253062,-17.8692137169407,2.50226015043363));
#38358=CARTESIAN_POINT('Ctrl Pts',(372.853230241241,-17.8701765391318,2.51200422578053));
#38359=CARTESIAN_POINT('Ctrl Pts',(372.847449555383,-17.8706350439528,2.51663926958221));
#38360=CARTESIAN_POINT('Ctrl Pts',(372.833571569182,-17.8717294124365,2.52768843928296));
#38361=CARTESIAN_POINT('Ctrl Pts',(372.82545925588,-17.8723639495244,2.5340836979523));
#38362=CARTESIAN_POINT('Ctrl Pts',(372.796073368577,-17.8746444658048,2.5570215226785));
#38363=CARTESIAN_POINT('Ctrl Pts',(372.774622596909,-17.8762753201882,2.57333662368372));
#38364=CARTESIAN_POINT('Ctrl Pts',(372.612968721112,-17.888336173369,2.69311711966996));
#38365=CARTESIAN_POINT('Ctrl Pts',(372.464767953331,-17.8981305986617,2.78534127973496));
#38366=CARTESIAN_POINT('Ctrl Pts',(372.30982061364,-17.9078850417037,2.86513684952479));
#38367=CARTESIAN_POINT('Origin',(370.834317853224,2.31077344927308,0.));
#38368=CARTESIAN_POINT('',(372.309820886087,-19.4026365087528,2.86513670921869));
#38369=CARTESIAN_POINT('',(372.309820613636,-19.1541342831958,2.86513684952678));
#38370=CARTESIAN_POINT('',(372.309820613641,2.31077344927308,2.86513684952399));
#38371=CARTESIAN_POINT('',(367.611567987131,-18.5635425847965,-0.000929030908117072));
#38372=CARTESIAN_POINT('Ctrl Pts',(372.309820886087,-19.4026365087528,2.86513670921864));
#38373=CARTESIAN_POINT('Ctrl Pts',(372.451012724632,-19.3937337882005,2.79242500044792));
#38374=CARTESIAN_POINT('Ctrl Pts',(372.586752355134,-19.3849172730876,2.70931674540583));
#38375=CARTESIAN_POINT('Ctrl Pts',(372.815210811217,-19.3688610084774,2.54502313882603));
#38376=CARTESIAN_POINT('Ctrl Pts',(372.910361849359,-19.3617482119209,2.46801867475545));
#38377=CARTESIAN_POINT('Ctrl Pts',(373.021643049223,-19.3527361787373,2.36696242610841));
#38378=CARTESIAN_POINT('Ctrl Pts',(373.042138607321,-19.3510455136871,2.34785648676577));
#38379=CARTESIAN_POINT('Ctrl Pts',(373.074094496837,-19.3483587261884,2.31727877877292));
#38380=CARTESIAN_POINT('Ctrl Pts',(373.085722132557,-19.3473702012269,2.30598332774414));
#38381=CARTESIAN_POINT('Ctrl Pts',(373.107191031656,-19.3455243189301,2.2848105989877));
#38382=CARTESIAN_POINT('Ctrl Pts',(373.117054408305,-19.3446679781463,2.27495621252225));
#38383=CARTESIAN_POINT('Ctrl Pts',(373.138807804842,-19.3427606244533,2.25293873228251));
#38384=CARTESIAN_POINT('Ctrl Pts',(373.150666038243,-19.3417082534954,2.24074495124684));
#38385=CARTESIAN_POINT('Ctrl Pts',(373.184952854174,-19.3386279334484,2.20492491418085));
#38386=CARTESIAN_POINT('Ctrl Pts',(373.207119888148,-19.3365888506403,2.18105230629932));
#38387=CARTESIAN_POINT('Ctrl Pts',(373.374045670421,-19.320858601998,1.99572591721334));
#38388=CARTESIAN_POINT('Ctrl Pts',(373.502512692134,-19.3064876522737,1.82039679920618));
#38389=CARTESIAN_POINT('Ctrl Pts',(373.723426328483,-19.2770668591204,1.44469973170487));
#38390=CARTESIAN_POINT('Ctrl Pts',(373.814927445316,-19.2620962467399,1.24502418872069));
#38391=CARTESIAN_POINT('Ctrl Pts',(373.893612733978,-19.2464190764061,1.01364323459907));
#38392=CARTESIAN_POINT('Ctrl Pts',(373.901477011672,-19.244809285654,0.989592119636126));
#38393=CARTESIAN_POINT('Ctrl Pts',(373.912059238191,-19.2425834688701,0.955890125530128));
#38394=CARTESIAN_POINT('Ctrl Pts',(373.915016437398,-19.2419545122697,0.946316122941213));
#38395=CARTESIAN_POINT('Ctrl Pts',(373.920058452308,-19.240870113285,0.929718340331362));
#38396=CARTESIAN_POINT('Ctrl Pts',(373.922164038936,-19.2404134876832,0.922701020433811));
#38397=CARTESIAN_POINT('Ctrl Pts',(373.926568669735,-19.2394503017213,0.907837702013906));
#38398=CARTESIAN_POINT('Ctrl Pts',(373.928861822364,-19.2389440987316,0.899990017253865));
#38399=CARTESIAN_POINT('Ctrl Pts',(373.934486774089,-19.2376902726851,0.880464476330244));
#38400=CARTESIAN_POINT('Ctrl Pts',(373.9377825179,-19.2369447150209,0.868776218601778));
#38401=CARTESIAN_POINT('Ctrl Pts',(373.949995254367,-19.2341388635721,0.824507645660303));
#38402=CARTESIAN_POINT('Ctrl Pts',(373.958466258092,-19.2321026690729,0.791805200823067));
#38403=CARTESIAN_POINT('Ctrl Pts',(374.019849171622,-19.2165686833898,0.538492662821227));
#38404=CARTESIAN_POINT('Ctrl Pts',(374.049853280193,-19.2040927502311,0.312957572843277));
#38405=CARTESIAN_POINT('Ctrl Pts',(374.061302742344,-19.1800861437778,-0.115356820233256));
#38406=CARTESIAN_POINT('Ctrl Pts',(374.047777092144,-19.1686545390522,-0.316865296403728));
#38407=CARTESIAN_POINT('Ctrl Pts',(374.011122748232,-19.1549482976994,-0.542941502003293));
#38408=CARTESIAN_POINT('Ctrl Pts',(374.00637102757,-19.1532910734376,-0.570046843804094));
#38409=CARTESIAN_POINT('Ctrl Pts',(373.998021505317,-19.1505590735351,-0.614332758561281));
#38410=CARTESIAN_POINT('Ctrl Pts',(373.994629364478,-19.14949082033,-0.631551003009051));
#38411=CARTESIAN_POINT('Ctrl Pts',(373.98828245973,-19.1475634457108,-0.662435120398092));
#38412=CARTESIAN_POINT('Ctrl Pts',(373.985379052945,-19.146705982806,-0.6761111844239));
#38413=CARTESIAN_POINT('Ctrl Pts',(373.979001449076,-19.1448723303964,-0.705218280905172));
#38414=CARTESIAN_POINT('Ctrl Pts',(373.975502462,-19.1438953663188,-0.720643449346488));
#38415=CARTESIAN_POINT('Ctrl Pts',(373.965731718371,-19.1412429513149,-0.762293808155959));
#38416=CARTESIAN_POINT('Ctrl Pts',(373.959244249751,-19.1395606184977,-0.788466606828006));
#38417=CARTESIAN_POINT('Ctrl Pts',(373.922779956108,-19.13050262772,-0.928051814776708));
#38418=CARTESIAN_POINT('Ctrl Pts',(373.886959379672,-19.1229398109753,-1.03983293588876));
#38419=CARTESIAN_POINT('Ctrl Pts',(373.754895207958,-19.0985562013961,-1.38576945027254));
#38420=CARTESIAN_POINT('Ctrl Pts',(373.637153655961,-19.0811581811182,-1.61065830930062));
#38421=CARTESIAN_POINT('Ctrl Pts',(373.44450385867,-19.0584512783996,-1.89231031788687));
#38422=CARTESIAN_POINT('Ctrl Pts',(373.39169191851,-19.0526656454684,-1.96309707654296));
#38423=CARTESIAN_POINT('Ctrl Pts',(373.326144741747,-19.0460539147674,-2.04381077121446));
#38424=CARTESIAN_POINT('Ctrl Pts',(373.316165237461,-19.0450617888305,-2.05591762849249));
#38425=CARTESIAN_POINT('Ctrl Pts',(373.299758726256,-19.043454818925,-2.07552799275485));
#38426=CARTESIAN_POINT('Ctrl Pts',(373.293385063146,-19.0428363497616,-2.08307551718272));
#38427=CARTESIAN_POINT('Ctrl Pts',(373.281898610934,-19.0417323109011,-2.09655128159395));
#38428=CARTESIAN_POINT('Ctrl Pts',(373.276798847984,-19.0412458277008,-2.10249029391497));
#38429=CARTESIAN_POINT('Ctrl Pts',(373.265563755886,-19.0401821437575,-2.11547825488287));
#38430=CARTESIAN_POINT('Ctrl Pts',(373.259419392365,-19.0396056198209,-2.12251912031126));
#38431=CARTESIAN_POINT('Ctrl Pts',(373.241676882191,-19.0379553595244,-2.14267275191081));
#38432=CARTESIAN_POINT('Ctrl Pts',(373.230002200027,-19.0368871168533,-2.15571810726184));
#38433=CARTESIAN_POINT('Ctrl Pts',(373.143088779976,-19.0290577347666,-2.25125749716476));
#38434=CARTESIAN_POINT('Ctrl Pts',(373.063706306622,-19.0225792061031,-2.32989615295844));
#38435=CARTESIAN_POINT('Ctrl Pts',(372.808883642388,-19.0031350986898,-2.55735412958696));
#38436=CARTESIAN_POINT('Ctrl Pts',(372.621485887732,-18.9905755990178,-2.69165490894473));
#38437=CARTESIAN_POINT('Ctrl Pts',(372.321198736284,-18.970837643492,-2.86156501591225));
#38438=CARTESIAN_POINT('Ctrl Pts',(372.218053772718,-18.9641281173776,-2.91284051630096));
#38439=CARTESIAN_POINT('Ctrl Pts',(372.087115555339,-18.9555733123906,-2.96940629667062));
#38440=CARTESIAN_POINT('Ctrl Pts',(372.061698465615,-18.9539112481575,-2.98000211379355));
#38441=CARTESIAN_POINT('Ctrl Pts',(372.02120966583,-18.9512599228766,-2.99627512649834));
#38442=CARTESIAN_POINT('Ctrl Pts',(372.006225461719,-18.9502779229291,-3.00216744219175));
#38443=CARTESIAN_POINT('Ctrl Pts',(371.978177691622,-18.9484380422996,-3.01295483478988));
#38444=CARTESIAN_POINT('Ctrl Pts',(371.965125229587,-18.9475811235609,-3.01787786933896));
#38445=CARTESIAN_POINT('Ctrl Pts',(371.935958556905,-18.9456645265899,-3.02866296352277));
#38446=CARTESIAN_POINT('Ctrl Pts',(371.919828785115,-18.9446034248848,-3.03448143595878));
#38447=CARTESIAN_POINT('Ctrl Pts',(371.872285082879,-18.9414718888481,-3.05120423971157));
#38448=CARTESIAN_POINT('Ctrl Pts',(371.840748675907,-18.9393897481342,-3.06175115716176));
#38449=CARTESIAN_POINT('Ctrl Pts',(371.768692498686,-18.9346196367783,-3.08461582866832));
#38450=CARTESIAN_POINT('Ctrl Pts',(371.728082439077,-18.9319221939621,-3.09662645229191));
#38451=CARTESIAN_POINT('Ctrl Pts',(371.59157180186,-18.9228230751304,-3.1340911978803));
#38452=CARTESIAN_POINT('Ctrl Pts',(371.494741135868,-18.916315005331,-3.1559149669713));
#38453=CARTESIAN_POINT('Ctrl Pts',(371.21833626417,-18.8976325265469,-3.20493309143997));
#38454=CARTESIAN_POINT('Ctrl Pts',(371.037252906775,-18.8852520378186,-3.22147140152816));
#38455=CARTESIAN_POINT('Ctrl Pts',(370.733215797561,-18.8648209650685,-3.22349381551713));
#38456=CARTESIAN_POINT('Ctrl Pts',(370.61071602129,-18.8566933440213,-3.21731918924799));
#38457=CARTESIAN_POINT('Ctrl Pts',(370.472258998816,-18.8478264833585,-3.20239122272093));
#38458=CARTESIAN_POINT('Ctrl Pts',(370.455677750087,-18.846769915271,-3.20047306770233));
#38459=CARTESIAN_POINT('Ctrl Pts',(370.429117818178,-18.8450868107117,-3.19719125135016));
#38460=CARTESIAN_POINT('Ctrl Pts',(370.419129569491,-18.8444559706803,-3.19590952024229));
#38461=CARTESIAN_POINT('Ctrl Pts',(370.401359706475,-18.8433376245148,-3.19354450839424));
#38462=CARTESIAN_POINT('Ctrl Pts',(370.393575852172,-18.8428491144423,-3.19247956566053));
#38463=CARTESIAN_POINT('Ctrl Pts',(370.376802560894,-18.8417994218955,-3.19012222243118));
#38464=CARTESIAN_POINT('Ctrl Pts',(370.367814661835,-18.8412387777074,-3.18882028561105));
#38465=CARTESIAN_POINT('Ctrl Pts',(370.342733350662,-18.8396790742257,-3.18507883441596));
#38466=CARTESIAN_POINT('Ctrl Pts',(370.32665248204,-18.8386846082506,-3.18255532566717));
#38467=CARTESIAN_POINT('Ctrl Pts',(370.229873136762,-18.8327292903931,-3.16661590043902));
#38468=CARTESIAN_POINT('Ctrl Pts',(370.14968326247,-18.8279190792379,-3.15025198162497));
#38469=CARTESIAN_POINT('Ctrl Pts',(369.845512685463,-18.8098557518665,-3.07601556310163));
#38470=CARTESIAN_POINT('Ctrl Pts',(369.627374552892,-18.7972409607748,-2.99715007174537));
#38471=CARTESIAN_POINT('Ctrl Pts',(369.291045897363,-18.7760218895102,-2.83282257705658));
#38472=CARTESIAN_POINT('Ctrl Pts',(369.166880637706,-18.7677595215318,-2.76156080301757));
#38473=CARTESIAN_POINT('Ctrl Pts',(369.025851502575,-18.7576093992297,-2.6676331572469));
#38474=CARTESIAN_POINT('Ctrl Pts',(369.004018422764,-18.7560153103336,-2.6527007247544));
#38475=CARTESIAN_POINT('Ctrl Pts',(368.9682753094,-18.7533664469392,-2.62760337206058));
#38476=CARTESIAN_POINT('Ctrl Pts',(368.954258317529,-18.7523175272013,-2.61759247793402));
#38477=CARTESIAN_POINT('Ctrl Pts',(368.929308441917,-18.7504318771016,-2.59946956482081));
#38478=CARTESIAN_POINT('Ctrl Pts',(368.918345362037,-18.7495967877095,-2.59139967577723));
#38479=CARTESIAN_POINT('Ctrl Pts',(368.906962012131,-18.7487227603054,-2.58290870354206));
#38480=CARTESIAN_POINT('Ctrl Pts',(368.906490250812,-18.7486865254295,-2.58255661010685));
#38481=CARTESIAN_POINT('Ctrl Pts',(368.905613988974,-18.7486191986383,-2.58190224863651));
#38482=CARTESIAN_POINT('Ctrl Pts',(368.905209462892,-18.7485881080562,-2.58160001468823));
#38483=CARTESIAN_POINT('Ctrl Pts',(368.9044546884,-18.7485300813512,-2.58103582285306));
#38484=CARTESIAN_POINT('Ctrl Pts',(368.904104422185,-18.7485031461553,-2.58077388866856));
#38485=CARTESIAN_POINT('Ctrl Pts',(368.903448392035,-18.7484526850307,-2.58028309148791));
#38486=CARTESIAN_POINT('Ctrl Pts',(368.903142615232,-18.7484291597506,-2.58005424527035));
#38487=CARTESIAN_POINT('Ctrl Pts',(368.902568042002,-18.7483849444246,-2.57962406992362));
#38488=CARTESIAN_POINT('Ctrl Pts',(368.9022992368,-18.7483642548975,-2.57942275346145));
#38489=CARTESIAN_POINT('Ctrl Pts',(368.901792714676,-18.748325260987,-2.57904327990657));
#38490=CARTESIAN_POINT('Ctrl Pts',(368.90155499064,-18.7483069569418,-2.57886513175161));
#38491=CARTESIAN_POINT('Ctrl Pts',(368.901105939673,-18.7482723753281,-2.57852852021724));
#38492=CARTESIAN_POINT('Ctrl Pts',(368.900894607248,-18.7482560980041,-2.57837006346816));
#38493=CARTESIAN_POINT('Ctrl Pts',(368.900494552842,-18.7482252800931,-2.57807002640754));
#38494=CARTESIAN_POINT('Ctrl Pts',(368.900305826744,-18.7482107396987,-2.57792845121671));
#38495=CARTESIAN_POINT('Ctrl Pts',(368.899947889935,-18.7481831586558,-2.57765987911257));
#38496=CARTESIAN_POINT('Ctrl Pts',(368.899778676684,-18.7481701182055,-2.57753288663675));
#38497=CARTESIAN_POINT('Ctrl Pts',(368.899457211003,-18.7481453413187,-2.5772915810855));
#38498=CARTESIAN_POINT('Ctrl Pts',(368.899304956129,-18.7481336050015,-2.57717727112944));
#38499=CARTESIAN_POINT('Ctrl Pts',(368.89901527509,-18.7481112729191,-2.57695974417649));
#38500=CARTESIAN_POINT('Ctrl Pts',(368.898877847376,-18.7481006772771,-2.57685652992174));
#38501=CARTESIAN_POINT('Ctrl Pts',(368.898616029925,-18.7480804891817,-2.57665986074643));
#38502=CARTESIAN_POINT('Ctrl Pts',(368.898491637807,-18.7480708967376,-2.57656640714193));
#38503=CARTESIAN_POINT('Ctrl Pts',(368.898108635053,-18.7480413589492,-2.57627862053249));
#38504=CARTESIAN_POINT('Ctrl Pts',(368.897850047608,-18.7480214124823,-2.57608425812408));
#38505=CARTESIAN_POINT('Ctrl Pts',(368.89733741382,-18.7479818623205,-2.57569882573889));
#38506=CARTESIAN_POINT('Ctrl Pts',(368.897083366226,-18.7479622586594,-2.57550775691557));
#38507=CARTESIAN_POINT('Ctrl Pts',(368.896579405829,-18.747923363138,-2.5751286122862));
#38508=CARTESIAN_POINT('Ctrl Pts',(368.896329492229,-18.7479040713328,-2.5749405377555));
#38509=CARTESIAN_POINT('Ctrl Pts',(368.895833420362,-18.7478657705733,-2.57456710167071));
#38510=CARTESIAN_POINT('Ctrl Pts',(368.895587261517,-18.7478467616786,-2.57438174135701));
#38511=CARTESIAN_POINT('Ctrl Pts',(368.88109967745,-18.7467277978641,-2.56346917505674));
#38512=CARTESIAN_POINT('Ctrl Pts',(368.866947726395,-18.7456232277403,-2.55262418252919));
#38513=CARTESIAN_POINT('Ctrl Pts',(368.83742363808,-18.7432941879183,-2.52960777178642));
#38514=CARTESIAN_POINT('Ctrl Pts',(368.822071171902,-18.7420687941547,-2.51741241193527));
#38515=CARTESIAN_POINT('Ctrl Pts',(368.781567216631,-18.7387972120977,-2.48463050636741));
#38516=CARTESIAN_POINT('Ctrl Pts',(368.756614762325,-18.7367414637005,-2.46380268530472));
#38517=CARTESIAN_POINT('Ctrl Pts',(368.61527695233,-18.724860872279,-2.3421539067914));
#38518=CARTESIAN_POINT('Ctrl Pts',(368.505935845111,-18.7147194559581,-2.23348462200715));
#38519=CARTESIAN_POINT('Ctrl Pts',(368.30260347148,-18.6939576492595,-2.00018232824538));
#38520=CARTESIAN_POINT('Ctrl Pts',(368.209040508131,-18.6833611218842,-1.87569309738877));
#38521=CARTESIAN_POINT('Ctrl Pts',(368.09206976599,-18.6688697463246,-1.69406445937904));
#38522=CARTESIAN_POINT('Ctrl Pts',(368.060744999295,-18.6648401083185,-1.64227684914999));
#38523=CARTESIAN_POINT('Ctrl Pts',(368.001643120891,-18.6569691725492,-1.53804698891253));
#38524=CARTESIAN_POINT('Ctrl Pts',(367.973817935267,-18.6531271520189,-1.48565672741149));
#38525=CARTESIAN_POINT('Ctrl Pts',(367.940584569664,-18.648384611323,-1.41868389269732));
#38526=CARTESIAN_POINT('Ctrl Pts',(367.93381589388,-18.6474099657379,-1.40479347587154));
#38527=CARTESIAN_POINT('Ctrl Pts',(367.923305677577,-18.6458832307948,-1.38282497376202));
#38528=CARTESIAN_POINT('Ctrl Pts',(367.919497357666,-18.645327177658,-1.37477935611536));
#38529=CARTESIAN_POINT('Ctrl Pts',(367.912375506448,-18.6442820383655,-1.35957080279077));
#38530=CARTESIAN_POINT('Ctrl Pts',(367.909054980676,-18.6437925478035,-1.35241153994755));
#38531=CARTESIAN_POINT('Ctrl Pts',(367.90135947377,-18.6426528381987,-1.33565859392353));
#38532=CARTESIAN_POINT('Ctrl Pts',(367.897005239223,-18.642003887901,-1.32605556068822));
#38533=CARTESIAN_POINT('Ctrl Pts',(367.883044313809,-18.639909234041,-1.29485929749686));
#38534=CARTESIAN_POINT('Ctrl Pts',(367.873627746383,-18.638474570192,-1.27318116163881));
#38535=CARTESIAN_POINT('Ctrl Pts',(367.824298493661,-18.6308284758156,-1.15611126230261));
#38536=CARTESIAN_POINT('Ctrl Pts',(367.788752120352,-18.6248410324956,-1.05893498910157));
#38537=CARTESIAN_POINT('Ctrl Pts',(367.716819209143,-18.6111043507131,-0.828471602173698));
#38538=CARTESIAN_POINT('Ctrl Pts',(367.684204119844,-18.603446239682,-0.694225362277117));
#38539=CARTESIAN_POINT('Ctrl Pts',(367.627921477791,-18.5852416036501,-0.374248736269292));
#38540=CARTESIAN_POINT('Ctrl Pts',(367.611621845575,-18.5746522845756,-0.187760588864271));
#38541=CARTESIAN_POINT('Ctrl Pts',(367.611567987131,-18.5635425847965,-0.000929030908117072));
#38542=CARTESIAN_POINT('Ctrl Pts',(367.611567986386,-18.5635424308017,-0.000926441180962114));
#38543=CARTESIAN_POINT('Ctrl Pts',(367.611561433042,-18.5621868546136,0.0218702425262871));
#38544=CARTESIAN_POINT('Ctrl Pts',(367.611796764245,-18.5608243144971,0.0446660322138806));
#38545=CARTESIAN_POINT('Ctrl Pts',(367.61269974216,-18.5582319726971,0.0877961717655694));
#38546=CARTESIAN_POINT('Ctrl Pts',(367.613318130634,-18.557003728493,0.108130382418844));
#38547=CARTESIAN_POINT('Ctrl Pts',(367.614679704908,-18.5549312730263,0.142262623923747));
#38548=CARTESIAN_POINT('Ctrl Pts',(367.615319194447,-18.5540902943665,0.156064364308312));
#38549=CARTESIAN_POINT('Ctrl Pts',(367.61675120443,-18.5524310824112,0.183195869062681));
#38550=CARTESIAN_POINT('Ctrl Pts',(367.617537861165,-18.5516130484395,0.196525672863026));
#38551=CARTESIAN_POINT('Ctrl Pts',(367.619385569006,-18.5498691035744,0.224841430668591));
#38552=CARTESIAN_POINT('Ctrl Pts',(367.620468613133,-18.5489425221585,0.239825584186962));
#38553=CARTESIAN_POINT('Ctrl Pts',(367.623500696627,-18.5465687318471,0.278055582785385));
#38554=CARTESIAN_POINT('Ctrl Pts',(367.625597407924,-18.5451169289521,0.301288529800636));
#38555=CARTESIAN_POINT('Ctrl Pts',(367.634766644662,-18.5394181927076,0.391890462042314));
#38556=CARTESIAN_POINT('Ctrl Pts',(367.643709849647,-18.535113288941,0.459048509102686));
#38557=CARTESIAN_POINT('Ctrl Pts',(367.702634207896,-18.5118308696448,0.815320799879443));
#38558=CARTESIAN_POINT('Ctrl Pts',(367.789806455443,-18.4916843078721,1.096852948199));
#38559=CARTESIAN_POINT('Ctrl Pts',(367.943811114952,-18.4673246458672,1.42692731569131));
#38560=CARTESIAN_POINT('Ctrl Pts',(367.97592467792,-18.4626269686303,1.49021490732091));
#38561=CARTESIAN_POINT('Ctrl Pts',(368.023604689163,-18.4561974305674,1.57695742094196));
#38562=CARTESIAN_POINT('Ctrl Pts',(368.037426676502,-18.454390931036,1.60134414030576));
#38563=CARTESIAN_POINT('Ctrl Pts',(368.062136589854,-18.4512633521572,1.64364467950337));
#38564=CARTESIAN_POINT('Ctrl Pts',(368.072884228646,-18.449934882808,1.66163810144827));
#38565=CARTESIAN_POINT('Ctrl Pts',(368.089041425074,-18.4479856094687,1.68809827325241));
#38566=CARTESIAN_POINT('Ctrl Pts',(368.094316023043,-18.4473565693565,1.69664622832731));
#38567=CARTESIAN_POINT('Ctrl Pts',(368.1037781462,-18.4462412448989,1.71182122852219));
#38568=CARTESIAN_POINT('Ctrl Pts',(368.107949970904,-18.4457539646683,1.71845779250366));
#38569=CARTESIAN_POINT('Ctrl Pts',(368.117079464797,-18.4446972959236,1.73286411596574));
#38570=CARTESIAN_POINT('Ctrl Pts',(368.122046262031,-18.4441285174633,1.7406278535319));
#38571=CARTESIAN_POINT('Ctrl Pts',(368.135965458597,-18.4425510721127,1.76218109323868));
#38572=CARTESIAN_POINT('Ctrl Pts',(368.144990314941,-18.4415470612145,1.7759237790307));
#38573=CARTESIAN_POINT('Ctrl Pts',(368.195802701521,-18.4359938776332,1.85202316421997));
#38574=CARTESIAN_POINT('Ctrl Pts',(368.23965709356,-18.4315699553687,1.91297920298884));
#38575=CARTESIAN_POINT('Ctrl Pts',(368.401466650583,-18.416271043705,2.12207277266602));
#38576=CARTESIAN_POINT('Ctrl Pts',(368.530303687065,-18.4058363291721,2.26130186850869));
#38577=CARTESIAN_POINT('Ctrl Pts',(368.76506159713,-18.3880595930074,2.47397106897141));
#38578=CARTESIAN_POINT('Ctrl Pts',(368.864481723045,-18.3808423235635,2.55383952574365));
#38579=CARTESIAN_POINT('Ctrl Pts',(369.008987276482,-18.3705178542385,2.65645788274047));
#38580=CARTESIAN_POINT('Ctrl Pts',(369.050273954255,-18.3675862744025,2.68435973652801));
#38581=CARTESIAN_POINT('Ctrl Pts',(369.114335635373,-18.3630536493607,2.72552227684239));
#38582=CARTESIAN_POINT('Ctrl Pts',(369.136654906391,-18.361477398524,2.73948005466697));
#38583=CARTESIAN_POINT('Ctrl Pts',(369.178400984181,-18.3585329351248,2.76488066665537));
#38584=CARTESIAN_POINT('Ctrl Pts',(369.197781820261,-18.3571674309792,2.77639614451246));
#38585=CARTESIAN_POINT('Ctrl Pts',(369.229977469707,-18.3549006999941,2.79507154085188));
#38586=CARTESIAN_POINT('Ctrl Pts',(369.242723427475,-18.3540037472758,2.8023490427497));
#38587=CARTESIAN_POINT('Ctrl Pts',(369.267507338053,-18.3522602727361,2.81627617472115));
#38588=CARTESIAN_POINT('Ctrl Pts',(369.279539035871,-18.3514141529309,2.82293632633563));
#38589=CARTESIAN_POINT('Ctrl Pts',(369.307936984545,-18.3494175477101,2.83841940127925));
#38590=CARTESIAN_POINT('Ctrl Pts',(369.32433755661,-18.3482648086236,2.84717802998766));
#38591=CARTESIAN_POINT('Ctrl Pts',(369.377943257472,-18.344497671982,2.87521240007685));
#38592=CARTESIAN_POINT('Ctrl Pts',(369.415447475562,-18.3418629653338,2.89390391937879));
#38593=CARTESIAN_POINT('Ctrl Pts',(369.632398845651,-18.3266205429553,2.9967979491953));
#38594=CARTESIAN_POINT('Ctrl Pts',(369.818919170711,-18.3134720320422,3.06502033581282));
#38595=CARTESIAN_POINT('Ctrl Pts',(370.173215382734,-18.2887448091165,3.15870080076113));
#38596=CARTESIAN_POINT('Ctrl Pts',(370.33906170517,-18.277275715564,3.18891391318488));
#38597=CARTESIAN_POINT('Ctrl Pts',(370.553584288714,-18.2630369163046,3.21084803578277));
#38598=CARTESIAN_POINT('Ctrl Pts',(370.600758455413,-18.2599434255684,3.21462391396209));
#38599=CARTESIAN_POINT('Ctrl Pts',(370.679137643247,-18.2548835773616,3.21916284300575));
#38600=CARTESIAN_POINT('Ctrl Pts',(370.710300239197,-18.2528927647022,3.22051395074741));
#38601=CARTESIAN_POINT('Ctrl Pts',(370.753248562283,-18.2501822523067,3.22175169337876));
#38602=CARTESIAN_POINT('Ctrl Pts',(370.765020262515,-18.2494427652063,3.22202638998329));
#38603=CARTESIAN_POINT('Ctrl Pts',(370.784892882518,-18.2482004856959,3.22238116259231));
#38604=CARTESIAN_POINT('Ctrl Pts',(370.792993010989,-18.247695840565,3.22249522066432));
#38605=CARTESIAN_POINT('Ctrl Pts',(370.808489848256,-18.2467337532987,3.22265499026134));
#38606=CARTESIAN_POINT('Ctrl Pts',(370.815886377183,-18.2462760205163,3.22270578169746));
#38607=CARTESIAN_POINT('Ctrl Pts',(370.833577585122,-18.2451845671903,3.22276635704575));
#38608=CARTESIAN_POINT('Ctrl Pts',(370.843872339146,-18.2445521597513,3.22275228005189));
#38609=CARTESIAN_POINT('Ctrl Pts',(370.880897287609,-18.2422869478081,3.22252423631014));
#38610=CARTESIAN_POINT('Ctrl Pts',(370.907625469464,-18.2406690065501,3.22202703215624));
#38611=CARTESIAN_POINT('Ctrl Pts',(371.12069639972,-18.2278873277165,3.21541056377437));
#38612=CARTESIAN_POINT('Ctrl Pts',(371.306218928516,-18.217454329542,3.19346284536564));
#38613=CARTESIAN_POINT('Ctrl Pts',(371.656424393001,-18.1974514474449,3.12082644107492));
#38614=CARTESIAN_POINT('Ctrl Pts',(371.820985622986,-18.1879091679197,3.07276729050772));
#38615=CARTESIAN_POINT('Ctrl Pts',(372.036481249505,-18.1745712257921,2.99072772526386));
#38616=CARTESIAN_POINT('Ctrl Pts',(372.091421869898,-18.1710951728397,2.96805290603718));
#38617=CARTESIAN_POINT('Ctrl Pts',(372.185238398458,-18.1650044255871,2.92626118903604));
#38618=CARTESIAN_POINT('Ctrl Pts',(372.224414434892,-18.162412947782,2.90785523919848));
#38619=CARTESIAN_POINT('Ctrl Pts',(372.278808144101,-18.1587413231323,2.88094920614493));
#38620=CARTESIAN_POINT('Ctrl Pts',(372.294346657032,-18.1576839085395,2.87310570647248));
#38621=CARTESIAN_POINT('Ctrl Pts',(372.309820613645,-18.1566220988445,2.86513684952223));
#38622=CARTESIAN_POINT('Ctrl Pts',(372.30982061364,-17.9078850417037,2.86513684952479));
#38623=CARTESIAN_POINT('Ctrl Pts',(372.309665113799,-17.9078948309285,2.86521692962436));
#38624=CARTESIAN_POINT('Ctrl Pts',(372.309509607163,-17.9079046201015,2.86529699720688));
#38625=CARTESIAN_POINT('Ctrl Pts',(372.149417046826,-17.9179819848434,2.94770930247267));
#38626=CARTESIAN_POINT('Ctrl Pts',(371.982871800774,-17.9279809453626,3.01650382468275));
#38627=CARTESIAN_POINT('Ctrl Pts',(371.753260760495,-17.9419028595915,3.08956185831615));
#38628=CARTESIAN_POINT('Ctrl Pts',(371.694542374156,-17.9454722331597,3.10642264911262));
#38629=CARTESIAN_POINT('Ctrl Pts',(371.592564343319,-17.9517121204166,3.13259221355794));
#38630=CARTESIAN_POINT('Ctrl Pts',(371.549526047059,-17.9543578076374,3.14269767417157));
#38631=CARTESIAN_POINT('Ctrl Pts',(371.487509907703,-17.9581935631353,3.15591929908358));
#38632=CARTESIAN_POINT('Ctrl Pts',(371.468689690302,-17.9593606681352,3.1597561345731));
#38633=CARTESIAN_POINT('Ctrl Pts',(371.435886103649,-17.9614007117614,3.16613884521319));
#38634=CARTESIAN_POINT('Ctrl Pts',(371.421917974562,-17.9622712005717,3.16876089888251));
#38635=CARTESIAN_POINT('Ctrl Pts',(371.39313609342,-17.9640688050595,3.17396689533857));
#38636=CARTESIAN_POINT('Ctrl Pts',(371.378320707143,-17.964996250804,3.17653971500232));
#38637=CARTESIAN_POINT('Ctrl Pts',(371.340448066994,-17.9673727748034,3.18284390426041));
#38638=CARTESIAN_POINT('Ctrl Pts',(371.317367569864,-17.9688264610973,3.18642841396283));
#38639=CARTESIAN_POINT('Ctrl Pts',(371.227210481178,-17.9745268940078,3.19942819398872));
#38640=CARTESIAN_POINT('Ctrl Pts',(371.159886665819,-17.9788315789448,3.20697820851767));
#38641=CARTESIAN_POINT('Ctrl Pts',(370.815643716397,-18.001098327878,3.23463218450161));
#38642=CARTESIAN_POINT('Ctrl Pts',(370.537223214437,-18.020088317223,3.22100630659121));
#38643=CARTESIAN_POINT('Ctrl Pts',(370.146169707613,-18.046764492343,3.15070108530287));
#38644=CARTESIAN_POINT('Ctrl Pts',(370.029537896644,-18.0546979102241,3.12294743593051));
#38645=CARTESIAN_POINT('Ctrl Pts',(369.897695638997,-18.0634488910075,3.08369447031538));
#38646=CARTESIAN_POINT('Ctrl Pts',(369.880721713374,-18.0645712465194,3.07848780958138));
#38647=CARTESIAN_POINT('Ctrl Pts',(369.85482649867,-18.0662760110946,3.07030985909656));
#38648=CARTESIAN_POINT('Ctrl Pts',(369.845874053369,-18.0668640028922,3.06743945405717));
#38649=CARTESIAN_POINT('Ctrl Pts',(369.829487334403,-18.0679375815943,3.06210622289666));
#38650=CARTESIAN_POINT('Ctrl Pts',(369.822049468652,-18.0684238373718,3.05965547275575));
#38651=CARTESIAN_POINT('Ctrl Pts',(369.805297842416,-18.0695166868434,3.0540680997207));
#38652=CARTESIAN_POINT('Ctrl Pts',(369.795989460649,-18.070122363661,3.05091597647042));
#38653=CARTESIAN_POINT('Ctrl Pts',(369.772030001172,-18.0716776090082,3.04268016254921));
#38654=CARTESIAN_POINT('Ctrl Pts',(369.757400747259,-18.0726235924178,3.0375331472809));
#38655=CARTESIAN_POINT('Ctrl Pts',(369.662971002363,-18.0787097385326,3.00354192872578));
#38656=CARTESIAN_POINT('Ctrl Pts',(369.58429179907,-18.0836880693738,2.97165863517123));
#38657=CARTESIAN_POINT('Ctrl Pts',(369.301497498598,-18.101553134999,2.84383836348255));
#38658=CARTESIAN_POINT('Ctrl Pts',(369.106343100387,-18.1138663872354,2.72966475108411));
#38659=CARTESIAN_POINT('Ctrl Pts',(368.846833302129,-18.1321226613698,2.53877252164653));
#38660=CARTESIAN_POINT('Ctrl Pts',(368.771591027677,-18.1376693027145,2.47802678712066));
#38661=CARTESIAN_POINT('Ctrl Pts',(368.66801894127,-18.1457782277218,2.38641969792796));
#38662=CARTESIAN_POINT('Ctrl Pts',(368.637380281222,-18.1482405403667,2.35824405694403));
#38663=CARTESIAN_POINT('Ctrl Pts',(368.583582762035,-18.1526868667367,2.30681283219935));
#38664=CARTESIAN_POINT('Ctrl Pts',(368.560216953395,-18.1546614824959,2.28378170403739));
#38665=CARTESIAN_POINT('Ctrl Pts',(368.525238962124,-18.1576868485972,2.24823562316858));
#38666=CARTESIAN_POINT('Ctrl Pts',(368.51336744887,-18.1587261971525,2.23597807361711));
#38667=CARTESIAN_POINT('Ctrl Pts',(368.491965269601,-18.1606232678165,2.21352584863382));
#38668=CARTESIAN_POINT('Ctrl Pts',(368.482402358576,-18.1614795652237,2.20336238619958));
#38669=CARTESIAN_POINT('Ctrl Pts',(368.461889109813,-18.1633353932994,2.18127519986581));
#38670=CARTESIAN_POINT('Ctrl Pts',(368.450962043675,-18.1643358817287,2.16933047503538));
#38671=CARTESIAN_POINT('Ctrl Pts',(368.421455852697,-18.1670705190176,2.1365842831454));
#38672=CARTESIAN_POINT('Ctrl Pts',(368.403056359257,-18.1688121087645,2.11562352556677));
#38673=CARTESIAN_POINT('Ctrl Pts',(368.306814269867,-18.1781198292555,2.00307053172437));
#38674=CARTESIAN_POINT('Ctrl Pts',(368.233878107522,-18.1858820255865,1.90742579353446));
#38675=CARTESIAN_POINT('Ctrl Pts',(368.038700649009,-18.2088312948118,1.6194154133175));
#38676=CARTESIAN_POINT('Ctrl Pts',(367.931289971958,-18.2244287289647,1.41788424658226));
#38677=CARTESIAN_POINT('Ctrl Pts',(367.818581118882,-18.2445786758436,1.13878095402693));
#38678=CARTESIAN_POINT('Ctrl Pts',(367.793459975509,-18.2494373953493,1.06989477207599));
#38679=CARTESIAN_POINT('Ctrl Pts',(367.757477377276,-18.2569732341094,0.959681058240468));
#38680=CARTESIAN_POINT('Ctrl Pts',(367.74505088434,-18.2597116941447,0.91889338381017));
#38681=CARTESIAN_POINT('Ctrl Pts',(367.729827255088,-18.263245777266,0.865119224278525));
#38682=CARTESIAN_POINT('Ctrl Pts',(367.726296365582,-18.264079579731,0.852347108118338));
#38683=CARTESIAN_POINT('Ctrl Pts',(367.720651109441,-18.2654358849767,0.831425190664511));
#38684=CARTESIAN_POINT('Ctrl Pts',(367.718489765131,-18.2659610186009,0.823288387078938));
#38685=CARTESIAN_POINT('Ctrl Pts',(367.714333907342,-18.2669822266133,0.807392051567859));
#38686=CARTESIAN_POINT('Ctrl Pts',(367.712336411367,-18.267478460698,0.799633432242072));
#38687=CARTESIAN_POINT('Ctrl Pts',(367.70749135303,-18.2686957545412,0.780519474099676));
#38688=CARTESIAN_POINT('Ctrl Pts',(367.704676656848,-18.2694149447895,0.769155773254699));
#38689=CARTESIAN_POINT('Ctrl Pts',(367.696714052944,-18.2714856751083,0.736241051033128));
#38690=CARTESIAN_POINT('Ctrl Pts',(367.691726280864,-18.2728285961033,0.714651497305161));
#38691=CARTESIAN_POINT('Ctrl Pts',(367.637064029954,-18.2881130404458,0.466399380181343));
#38692=CARTESIAN_POINT('Ctrl Pts',(367.611779436814,-18.3008908155179,0.23502725988353));
#38693=CARTESIAN_POINT('Ctrl Pts',(367.611379681676,-18.3255973486856,-0.20626324314669));
#38694=CARTESIAN_POINT('Ctrl Pts',(367.631555742899,-18.337433932554,-0.414938720819074));
#38695=CARTESIAN_POINT('Ctrl Pts',(367.677080944046,-18.3515927856995,-0.647089576842867));
#38696=CARTESIAN_POINT('Ctrl Pts',(367.682702210047,-18.3532446356701,-0.673935151891065));
#38697=CARTESIAN_POINT('Ctrl Pts',(367.692476436401,-18.3559699765553,-0.717814267250105));
#38698=CARTESIAN_POINT('Ctrl Pts',(367.69642702409,-18.357037006491,-0.734891785432829));
#38699=CARTESIAN_POINT('Ctrl Pts',(367.703780437963,-18.3589636254771,-0.765538194276729));
#38700=CARTESIAN_POINT('Ctrl Pts',(367.707132691253,-18.3598215695404,-0.779118853732655));
#38701=CARTESIAN_POINT('Ctrl Pts',(367.714472005468,-18.3616578356588,-0.808041278383915));
#38702=CARTESIAN_POINT('Ctrl Pts',(367.718484043535,-18.3626369449096,-0.823376267203227));
#38703=CARTESIAN_POINT('Ctrl Pts',(367.729658053295,-18.3652992007026,-0.864834548370007));
#38704=CARTESIAN_POINT('Ctrl Pts',(367.737036386613,-18.3669893090864,-0.890897701181946));
#38705=CARTESIAN_POINT('Ctrl Pts',(367.77861296461,-18.3761657200652,-1.03099913954588));
#38706=CARTESIAN_POINT('Ctrl Pts',(367.818778224723,-18.3838450610775,-1.1431564164714));
#38707=CARTESIAN_POINT('Ctrl Pts',(367.92576857589,-18.4019802522657,-1.39672974376027));
#38708=CARTESIAN_POINT('Ctrl Pts',(367.996863543076,-18.4125367849318,-1.53602052723518));
#38709=CARTESIAN_POINT('Ctrl Pts',(368.164581427382,-18.4344365281345,-1.81292713735376));
#38710=CARTESIAN_POINT('Ctrl Pts',(368.262449119488,-18.4457477161982,-1.94928172049029));
#38711=CARTESIAN_POINT('Ctrl Pts',(368.387856699903,-18.4582471133576,-2.09801608158198));
#38712=CARTESIAN_POINT('Ctrl Pts',(368.405484750028,-18.4599635201717,-2.11839881049245));
#38713=CARTESIAN_POINT('Ctrl Pts',(368.43022149595,-18.4623138789628,-2.14628631961244));
#38714=CARTESIAN_POINT('Ctrl Pts',(368.437113180321,-18.4629625962881,-2.15398097109664));
#38715=CARTESIAN_POINT('Ctrl Pts',(368.449011575299,-18.4640719807624,-2.16713784060525));
#38716=CARTESIAN_POINT('Ctrl Pts',(368.454000295682,-18.4645339561658,-2.17261611601515));
#38717=CARTESIAN_POINT('Ctrl Pts',(368.464482605557,-18.4654979690725,-2.18404763675884));
#38718=CARTESIAN_POINT('Ctrl Pts',(368.469979807997,-18.465999707135,-2.18999744072849));
#38719=CARTESIAN_POINT('Ctrl Pts',(368.483506308833,-18.4672251578462,-2.20452732564601));
#38720=CARTESIAN_POINT('Ctrl Pts',(368.491560313153,-18.4679470117112,-2.21308444600156));
#38721=CARTESIAN_POINT('Ctrl Pts',(368.52102611119,-18.4705605420995,-2.2440497876282));
#38722=CARTESIAN_POINT('Ctrl Pts',(368.542714810309,-18.4724321883214,-2.26619367841296));
#38723=CARTESIAN_POINT('Ctrl Pts',(368.598021606244,-18.477086712869,-2.32105510469655));
#38724=CARTESIAN_POINT('Ctrl Pts',(368.632041603794,-18.4798436267073,-2.35335876140487));
#38725=CARTESIAN_POINT('Ctrl Pts',(368.916620752167,-18.5021729162937,-2.61200285310076));
#38726=CARTESIAN_POINT('Ctrl Pts',(369.200622905637,-18.5201530414036,-2.7984285062356));
#38727=CARTESIAN_POINT('Ctrl Pts',(369.565603648433,-18.5436123541569,-2.96317697938668));
#38728=CARTESIAN_POINT('Ctrl Pts',(369.623523868706,-18.5473359423497,-2.98731161669759));
#38729=CARTESIAN_POINT('Ctrl Pts',(369.703294904873,-18.5524832993742,-3.01785010980724));
#38730=CARTESIAN_POINT('Ctrl Pts',(369.72456561599,-18.5538575878478,-3.02573662544653));
#38731=CARTESIAN_POINT('Ctrl Pts',(369.758534281309,-18.5560558247618,-3.03792477658731));
#38732=CARTESIAN_POINT('Ctrl Pts',(369.771179124183,-18.5568748915467,-3.0423729679479));
#38733=CARTESIAN_POINT('Ctrl Pts',(369.797197935718,-18.5585620087448,-3.05134382698736));
#38734=CARTESIAN_POINT('Ctrl Pts',(369.810574591674,-18.5594303267327,-3.05585775162006));
#38735=CARTESIAN_POINT('Ctrl Pts',(369.8416458933,-18.5614496421438,-3.06611578874955));
#38736=CARTESIAN_POINT('Ctrl Pts',(369.859361342558,-18.5626027495016,-3.07179482210187));
#38737=CARTESIAN_POINT('Ctrl Pts',(369.916068229302,-18.5663000293194,-3.0894333660342));
#38738=CARTESIAN_POINT('Ctrl Pts',(369.955236696981,-18.5688631758737,-3.10080585829091));
#38739=CARTESIAN_POINT('Ctrl Pts',(370.047705068625,-18.5749385952949,-3.12576109332134));
#38740=CARTESIAN_POINT('Ctrl Pts',(370.101156486561,-18.5784693867073,-3.13872839241657));
#38741=CARTESIAN_POINT('Ctrl Pts',(370.301185206125,-18.5917525497531,-3.18186712662266));
#38742=CARTESIAN_POINT('Ctrl Pts',(370.44946400873,-18.6017490176813,-3.20318402681224));
#38743=CARTESIAN_POINT('Ctrl Pts',(370.816286029456,-18.6265796853989,-3.23007780540514));
#38744=CARTESIAN_POINT('Ctrl Pts',(371.034971459471,-18.641488490177,-3.22389199146721));
#38745=CARTESIAN_POINT('Ctrl Pts',(371.276436450036,-18.657110023523,-3.19237967185828));
#38746=CARTESIAN_POINT('Ctrl Pts',(371.301468994018,-18.6587187303267,-3.1888127455819));
#38747=CARTESIAN_POINT('Ctrl Pts',(371.336403339736,-18.6609462851765,-3.18341467630133));
#38748=CARTESIAN_POINT('Ctrl Pts',(371.346341737351,-18.6615780120427,-3.18183129431249));
#38749=CARTESIAN_POINT('Ctrl Pts',(371.36351657664,-18.6626660902676,-3.17901245055126));
#38750=CARTESIAN_POINT('Ctrl Pts',(371.370756447126,-18.6631236411341,-3.17779878015446));
#38751=CARTESIAN_POINT('Ctrl Pts',(371.386046544524,-18.6640875033625,-3.17518185094773));
#38752=CARTESIAN_POINT('Ctrl Pts',(371.394095698605,-18.6645934638954,-3.17377269220271));
#38753=CARTESIAN_POINT('Ctrl Pts',(371.414052800967,-18.6658445502377,-3.17020053419664));
#38754=CARTESIAN_POINT('Ctrl Pts',(371.425954229934,-18.666587634076,-3.16800101723802));
#38755=CARTESIAN_POINT('Ctrl Pts',(371.470694266014,-18.6693706961138,-3.15947163921331));
#38756=CARTESIAN_POINT('Ctrl Pts',(371.503447330943,-18.6713870877218,-3.15269756240237));
#38757=CARTESIAN_POINT('Ctrl Pts',(371.751828510616,-18.6865586707859,-3.09728130408462));
#38758=CARTESIAN_POINT('Ctrl Pts',(371.962070051936,-18.6987409357764,-3.02707402774668));
#38759=CARTESIAN_POINT('Ctrl Pts',(372.352928981711,-18.7227647890337,-2.85011954174657));
#38760=CARTESIAN_POINT('Ctrl Pts',(372.533598432476,-18.7345362428666,-2.74623216680772));
#38761=CARTESIAN_POINT('Ctrl Pts',(372.725346998694,-18.748621901833,-2.60976611878067));
#38762=CARTESIAN_POINT('Ctrl Pts',(372.747497224853,-18.7502744011564,-2.59357187017878));
#38763=CARTESIAN_POINT('Ctrl Pts',(372.783456926749,-18.7530005964673,-2.56657004566426));
#38764=CARTESIAN_POINT('Ctrl Pts',(372.797390028108,-18.7540678244717,-2.5559289005277));
#38765=CARTESIAN_POINT('Ctrl Pts',(372.822282936842,-18.7559946587017,-2.53659379284251));
#38766=CARTESIAN_POINT('Ctrl Pts',(372.833274344976,-18.7568526183678,-2.52794109462594));
#38767=CARTESIAN_POINT('Ctrl Pts',(372.856598039331,-18.758688762904,-2.50933289959637));
#38768=CARTESIAN_POINT('Ctrl Pts',(372.868913878038,-18.7596677338427,-2.49935746814898));
#38769=CARTESIAN_POINT('Ctrl Pts',(372.90207007223,-18.7623292222263,-2.47209455469661));
#38770=CARTESIAN_POINT('Ctrl Pts',(372.922766586904,-18.764018694681,-2.45463491001722));
#38771=CARTESIAN_POINT('Ctrl Pts',(373.033142588268,-18.7731842611679,-2.35911486843591));
#38772=CARTESIAN_POINT('Ctrl Pts',(373.118660443868,-18.7808528455383,-2.27640646205571));
#38773=CARTESIAN_POINT('Ctrl Pts',(373.305207014915,-18.7989474736678,-2.07486939361421));
#38774=CARTESIAN_POINT('Ctrl Pts',(373.402574731008,-18.809473232447,-1.95305556505446));
#38775=CARTESIAN_POINT('Ctrl Pts',(373.585977416438,-18.8313858387925,-1.68605348148778));
#38776=CARTESIAN_POINT('Ctrl Pts',(373.670217151245,-18.842740940469,-1.5401599097305));
#38777=CARTESIAN_POINT('Ctrl Pts',(373.754294437162,-18.8552801028434,-1.36403086282793));
#38778=CARTESIAN_POINT('Ctrl Pts',(373.76559610371,-18.8569962599118,-1.3395713395968));
#38779=CARTESIAN_POINT('Ctrl Pts',(373.780804619568,-18.859346339912,-1.30554202755263));
#38780=CARTESIAN_POINT('Ctrl Pts',(373.784973832728,-18.8599950236202,-1.29609164312704));
#38781=CARTESIAN_POINT('Ctrl Pts',(373.792055556113,-18.8611043657702,-1.27982816758715));
#38782=CARTESIAN_POINT('Ctrl Pts',(373.794990108312,-18.8615663322498,-1.27302484587574));
#38783=CARTESIAN_POINT('Ctrl Pts',(373.801083928449,-18.8625303438933,-1.25876218471752));
#38784=CARTESIAN_POINT('Ctrl Pts',(373.804238569916,-18.8630320895178,-1.25130097144065));
#38785=CARTESIAN_POINT('Ctrl Pts',(373.81190061876,-18.8642575872455,-1.23298683544353));
#38786=CARTESIAN_POINT('Ctrl Pts',(373.816376916963,-18.8649794802337,-1.2221208664844));
#38787=CARTESIAN_POINT('Ctrl Pts',(373.832443764382,-18.8675933147685,-1.18250557092711));
#38788=CARTESIAN_POINT('Ctrl Pts',(373.843679227197,-18.8694652199086,-1.1536128841999));
#38789=CARTESIAN_POINT('Ctrl Pts',(373.870867137919,-18.874120522916,-1.08059566270273));
#38790=CARTESIAN_POINT('Ctrl Pts',(373.886276581807,-18.8768779451818,-1.03627549390567));
#38791=CARTESIAN_POINT('Ctrl Pts',(374.004679216291,-18.899221434189,-0.670142569164643));
#38792=CARTESIAN_POINT('Ctrl Pts',(374.057448020884,-18.9172134657338,-0.334296922208163));
#38793=CARTESIAN_POINT('Ctrl Pts',(374.056995052279,-18.9406778914367,0.0661883945450329));
#38794=CARTESIAN_POINT('Ctrl Pts',(374.055103692997,-18.9443902411663,0.12871300483197));
#38795=CARTESIAN_POINT('Ctrl Pts',(374.050050778173,-18.9495244073616,0.213758549730239));
#38796=CARTESIAN_POINT('Ctrl Pts',(374.048468449479,-18.950897077887,0.236361728238311));
#38797=CARTESIAN_POINT('Ctrl Pts',(374.045571318633,-18.9530933734128,0.272301823266245));
#38798=CARTESIAN_POINT('Ctrl Pts',(374.044411427091,-18.9539121325887,0.285650731774019));
#38799=CARTESIAN_POINT('Ctrl Pts',(374.041858333086,-18.9555990980942,0.313051132780387));
#38800=CARTESIAN_POINT('Ctrl Pts',(374.040455961039,-18.9564675750236,0.32710146013089));
#38801=CARTESIAN_POINT('Ctrl Pts',(374.036990322945,-18.9584880814232,0.35965721796383));
#38802=CARTESIAN_POINT('Ctrl Pts',(374.034858936996,-18.9596422287215,0.378154744137123));
#38803=CARTESIAN_POINT('Ctrl Pts',(374.027536839797,-18.9633462670263,0.437196544117848));
#38804=CARTESIAN_POINT('Ctrl Pts',(374.021735194516,-18.9659152298723,0.477659669921169));
#38805=CARTESIAN_POINT('Ctrl Pts',(374.006300666022,-18.972006853065,0.572437432523947));
#38806=CARTESIAN_POINT('Ctrl Pts',(373.996040010534,-18.9755481659373,0.626635459845248));
#38807=CARTESIAN_POINT('Ctrl Pts',(373.952642131851,-18.9888903769495,0.827514792632508));
#38808=CARTESIAN_POINT('Ctrl Pts',(373.910646173259,-18.9989377589264,0.972071278230671));
#38809=CARTESIAN_POINT('Ctrl Pts',(373.783738820259,-19.0237446769951,1.31687400168511));
#38810=CARTESIAN_POINT('Ctrl Pts',(373.68836220749,-19.0385733831318,1.51250972265325));
#38811=CARTESIAN_POINT('Ctrl Pts',(373.560684429104,-19.0541283304377,1.71862893220527));
#38812=CARTESIAN_POINT('Ctrl Pts',(373.547081764963,-19.055741244464,1.7400207367515));
#38813=CARTESIAN_POINT('Ctrl Pts',(373.527721860386,-19.0579736367487,1.76968751828831));
#38814=CARTESIAN_POINT('Ctrl Pts',(373.522176469462,-19.0586060650166,1.77809873844025));
#38815=CARTESIAN_POINT('Ctrl Pts',(373.512520851668,-19.0596950191552,1.79259593588793));
#38816=CARTESIAN_POINT('Ctrl Pts',(373.508429135349,-19.0601527489896,1.79869406615128));
#38817=CARTESIAN_POINT('Ctrl Pts',(373.499742239819,-19.0611165967424,1.81154550655377));
#38818=CARTESIAN_POINT('Ctrl Pts',(373.495142164213,-19.0616223660171,1.81829543021478));
#38819=CARTESIAN_POINT('Ctrl Pts',(373.483671561335,-19.0628723146617,1.83499007896691));
#38820=CARTESIAN_POINT('Ctrl Pts',(373.476770574373,-19.0636144602543,1.84491389713835));
#38821=CARTESIAN_POINT('Ctrl Pts',(373.450630588182,-19.0663898340582,1.88205637645325));
#38822=CARTESIAN_POINT('Ctrl Pts',(373.431024813298,-19.0683996436644,1.90901589648941));
#38823=CARTESIAN_POINT('Ctrl Pts',(373.279349867431,-19.0834558791109,2.11091970121108));
#38824=CARTESIAN_POINT('Ctrl Pts',(373.130143250801,-19.0955446718493,2.27230581699969));
#38825=CARTESIAN_POINT('Ctrl Pts',(372.808198637967,-19.1195735167413,2.55616863627562));
#38826=CARTESIAN_POINT('Ctrl Pts',(372.637536906503,-19.131451436681,2.67928884237165));
#38827=CARTESIAN_POINT('Ctrl Pts',(372.432425920222,-19.1456571967526,2.79873550709));
#38828=CARTESIAN_POINT('Ctrl Pts',(372.408549803685,-19.1473090589213,2.81223461481011));
#38829=CARTESIAN_POINT('Ctrl Pts',(372.369137319987,-19.1500344158585,2.8338585034132));
#38830=CARTESIAN_POINT('Ctrl Pts',(372.353701512038,-19.1511014495157,2.84216433222546));
#38831=CARTESIAN_POINT('Ctrl Pts',(372.328763936574,-19.1528250819395,2.85532174488835));
#38832=CARTESIAN_POINT('Ctrl Pts',(372.319304375368,-19.153478853133,2.86025285363061));
#38833=CARTESIAN_POINT('Ctrl Pts',(372.309820613636,-19.1541342831958,2.86513684952685));
#38834=CARTESIAN_POINT('Origin',(370.834317853224,2.31077344927308,0.));
#38835=CARTESIAN_POINT('',(372.309820629953,-20.6514935740585,2.86513684112382));
#38836=CARTESIAN_POINT('',(372.309820109182,-20.4075893673376,2.8651371093129));
#38837=CARTESIAN_POINT('',(372.309820613641,2.31077344927308,2.86513684952399));
#38838=CARTESIAN_POINT('Ctrl Pts',(372.309820629953,-20.6514935740584,2.86513684112379));
#38839=CARTESIAN_POINT('Ctrl Pts',(372.324583288222,-20.6503904433452,2.85753429210912));
#38840=CARTESIAN_POINT('Ctrl Pts',(372.339291174212,-20.64929025969,2.84981559336732));
#38841=CARTESIAN_POINT('Ctrl Pts',(372.395235037442,-20.6451027812944,2.81990206143058));
#38842=CARTESIAN_POINT('Ctrl Pts',(372.436043231241,-20.6420424298463,2.79692444492251));
#38843=CARTESIAN_POINT('Ctrl Pts',(372.50296861048,-20.6370307707822,2.75729578544244));
#38844=CARTESIAN_POINT('Ctrl Pts',(372.529371715499,-20.6350555600094,2.74114355089575));
#38845=CARTESIAN_POINT('Ctrl Pts',(372.565463786448,-20.6323625883558,2.71834308507967));
#38846=CARTESIAN_POINT('Ctrl Pts',(372.575354284503,-20.6316253643962,2.71201908645424));
#38847=CARTESIAN_POINT('Ctrl Pts',(372.592005262767,-20.6303857832336,2.70124379535853));
#38848=CARTESIAN_POINT('Ctrl Pts',(372.598783874991,-20.6298815911851,2.69682085699796));
#38849=CARTESIAN_POINT('Ctrl Pts',(372.611731474634,-20.628919503314,2.68830303380777));
#38850=CARTESIAN_POINT('Ctrl Pts',(372.617903088859,-20.6284613225708,2.6842123785172));
#38851=CARTESIAN_POINT('Ctrl Pts',(372.632645542387,-20.6273676840638,2.67436752374572));
#38852=CARTESIAN_POINT('Ctrl Pts',(372.641203001412,-20.6267335513693,2.66859329941169));
#38853=CARTESIAN_POINT('Ctrl Pts',(372.671987988741,-20.6244542021076,2.64760487159186));
#38854=CARTESIAN_POINT('Ctrl Pts',(372.694053005574,-20.6228240976427,2.63215279832257));
#38855=CARTESIAN_POINT('Ctrl Pts',(372.852746208518,-20.6111063275073,2.51802843755481));
#38856=CARTESIAN_POINT('Ctrl Pts',(372.981658347962,-20.6016124942679,2.40903775557397));
#38857=CARTESIAN_POINT('Ctrl Pts',(373.212009111439,-20.5834632775565,2.18103062259949));
#38858=CARTESIAN_POINT('Ctrl Pts',(373.314485233728,-20.5748212028382,2.06375335691227));
#38859=CARTESIAN_POINT('Ctrl Pts',(373.479586857849,-20.5591386133118,1.84466338293518));
#38860=CARTESIAN_POINT('Ctrl Pts',(373.545776542936,-20.5522167406175,1.74591476204762));
#38861=CARTESIAN_POINT('Ctrl Pts',(373.620161257533,-20.5434636516853,1.62047099395734));
#38862=CARTESIAN_POINT('Ctrl Pts',(373.633668206809,-20.5418295046034,1.59702449753135));
#38863=CARTESIAN_POINT('Ctrl Pts',(373.654610207764,-20.539222026732,1.55958950508434));
#38864=CARTESIAN_POINT('Ctrl Pts',(373.662240300058,-20.5382557035163,1.54571116646521));
#38865=CARTESIAN_POINT('Ctrl Pts',(373.676411466993,-20.5364296071305,1.51947913406856));
#38866=CARTESIAN_POINT('Ctrl Pts',(373.68297508463,-20.5355706619534,1.50713798853662));
#38867=CARTESIAN_POINT('Ctrl Pts',(373.697583134365,-20.5336287872889,1.47923506137128));
#38868=CARTESIAN_POINT('Ctrl Pts',(373.705581334097,-20.5325442593025,1.46364969886281));
#38869=CARTESIAN_POINT('Ctrl Pts',(373.725769468597,-20.5297509313047,1.42350857973443));
#38870=CARTESIAN_POINT('Ctrl Pts',(373.737773660644,-20.5280357343837,1.39886147290829));
#38871=CARTESIAN_POINT('Ctrl Pts',(373.839337072564,-20.5130371168941,1.18338986790783));
#38872=CARTESIAN_POINT('Ctrl Pts',(373.910272372336,-20.4991075794542,0.984391604116014));
#38873=CARTESIAN_POINT('Ctrl Pts',(374.000455015869,-20.4739811563885,0.622824594982));
#38874=CARTESIAN_POINT('Ctrl Pts',(374.027745360789,-20.462948082131,0.462987970792784));
#38875=CARTESIAN_POINT('Ctrl Pts',(374.050544783541,-20.4467955758357,0.220575524284215));
#38876=CARTESIAN_POINT('Ctrl Pts',(374.055097362522,-20.4414673146229,0.139107810831596));
#38877=CARTESIAN_POINT('Ctrl Pts',(374.056844418894,-20.4352547762159,0.0412869601068374));
#38878=CARTESIAN_POINT('Ctrl Pts',(374.05701174876,-20.4342280325143,0.0250232089321368));
#38879=CARTESIAN_POINT('Ctrl Pts',(374.057080624951,-20.4326383995095,-0.000320171998430622));
#38880=CARTESIAN_POINT('Ctrl Pts',(374.057066935641,-20.432071001271,-0.00939903622049846));
#38881=CARTESIAN_POINT('Ctrl Pts',(374.05696983288,-20.4310165860551,-0.0263345968753181));
#38882=CARTESIAN_POINT('Ctrl Pts',(374.056896055615,-20.4305290674782,-0.0341909936959644));
#38883=CARTESIAN_POINT('Ctrl Pts',(374.056662107682,-20.4294200938858,-0.0521205993707929));
#38884=CARTESIAN_POINT('Ctrl Pts',(374.056483435635,-20.4287996723389,-0.0621933839278968));
#38885=CARTESIAN_POINT('Ctrl Pts',(374.055882932423,-20.4271571080255,-0.0889667388121332));
#38886=CARTESIAN_POINT('Ctrl Pts',(374.055378469183,-20.4261393677661,-0.105665393491946));
#38887=CARTESIAN_POINT('Ctrl Pts',(374.050054104149,-20.4176494938012,-0.245799076200485));
#38888=CARTESIAN_POINT('Ctrl Pts',(374.03827014266,-20.4105226904863,-0.36888150311233));
#38889=CARTESIAN_POINT('Ctrl Pts',(373.990329562263,-20.3926913286214,-0.679875734584698));
#38890=CARTESIAN_POINT('Ctrl Pts',(373.944470335683,-20.382179002354,-0.865791504826672));
#38891=CARTESIAN_POINT('Ctrl Pts',(373.83705695062,-20.3634010670208,-1.17863396699224));
#38892=CARTESIAN_POINT('Ctrl Pts',(373.783174619783,-20.3553183756282,-1.30761503569664));
#38893=CARTESIAN_POINT('Ctrl Pts',(373.708566707221,-20.3452554309117,-1.45794591329469));
#38894=CARTESIAN_POINT('Ctrl Pts',(373.695699934448,-20.3435536084455,-1.4830392002752));
#38895=CARTESIAN_POINT('Ctrl Pts',(373.67497940397,-20.3408629295831,-1.52217549880286));
#38896=CARTESIAN_POINT('Ctrl Pts',(373.667346766217,-20.3398818787172,-1.5363344227502));
#38897=CARTESIAN_POINT('Ctrl Pts',(373.652896706246,-20.3380428590516,-1.56266613556717));
#38898=CARTESIAN_POINT('Ctrl Pts',(373.64610558809,-20.3371858442013,-1.57485298561577));
#38899=CARTESIAN_POINT('Ctrl Pts',(373.630781533879,-20.3352678448751,-1.60193732210998));
#38900=CARTESIAN_POINT('Ctrl Pts',(373.622208301866,-20.3342054270773,-1.61681140808226));
#38901=CARTESIAN_POINT('Ctrl Pts',(373.60021940518,-20.3315066862081,-1.65426600255352));
#38902=CARTESIAN_POINT('Ctrl Pts',(373.586645979849,-20.3298646790583,-1.67675198526912));
#38903=CARTESIAN_POINT('Ctrl Pts',(373.500103992828,-20.3195395445211,-1.81623639875334));
#38904=CARTESIAN_POINT('Ctrl Pts',(373.419973531792,-20.3105927746075,-1.9286021818012));
#38905=CARTESIAN_POINT('Ctrl Pts',(373.198073387264,-20.2872801811893,-2.20098828315791));
#38906=CARTESIAN_POINT('Ctrl Pts',(373.047132238567,-20.2726627443467,-2.35268630125291));
#38907=CARTESIAN_POINT('Ctrl Pts',(372.828364666454,-20.2537219734903,-2.53274125151364));
#38908=CARTESIAN_POINT('Ctrl Pts',(372.772974775291,-20.2490970432678,-2.57538569581566));
#38909=CARTESIAN_POINT('Ctrl Pts',(372.693713943368,-20.2427568278717,-2.63240073959923));
#38910=CARTESIAN_POINT('Ctrl Pts',(372.670979839837,-20.2409689473225,-2.64831273262103));
#38911=CARTESIAN_POINT('Ctrl Pts',(372.630854178683,-20.2378703786869,-2.67563210694264));
#38912=CARTESIAN_POINT('Ctrl Pts',(372.613552694506,-20.2365524781537,-2.68716828138095));
#38913=CARTESIAN_POINT('Ctrl Pts',(372.587756552771,-20.2346156582034,-2.7040100842197));
#38914=CARTESIAN_POINT('Ctrl Pts',(372.579347262632,-20.2339886496511,-2.70944462487207));
#38915=CARTESIAN_POINT('Ctrl Pts',(372.564311214331,-20.2328755128736,-2.7190626957432));
#38916=CARTESIAN_POINT('Ctrl Pts',(372.557694395383,-20.2323884045542,-2.72326132991864));
#38917=CARTESIAN_POINT('Ctrl Pts',(372.543242262024,-20.2313304719903,-2.73235801173618));
#38918=CARTESIAN_POINT('Ctrl Pts',(372.535401176276,-20.230760270171,-2.73724651288528));
#38919=CARTESIAN_POINT('Ctrl Pts',(372.513461790462,-20.2291750622415,-2.75079387286468));
#38920=CARTESIAN_POINT('Ctrl Pts',(372.499317448713,-20.2281647859198,-2.75937813041033));
#38921=CARTESIAN_POINT('Ctrl Pts',(372.419144689466,-20.2225004318338,-2.8071943727758));
#38922=CARTESIAN_POINT('Ctrl Pts',(372.351791083465,-20.2179775971129,-2.84416830470394));
#38923=CARTESIAN_POINT('Ctrl Pts',(372.262992842847,-20.2122307012515,-2.88886064756223));
#38924=CARTESIAN_POINT('Ctrl Pts',(372.242703963854,-20.2109318217702,-2.89880607574419));
#38925=CARTESIAN_POINT('Ctrl Pts',(372.152136628291,-20.2051894355994,-2.94202605078323));
#38926=CARTESIAN_POINT('Ctrl Pts',(372.080769921292,-20.200811677939,-2.9729651324264));
#38927=CARTESIAN_POINT('Ctrl Pts',(371.832996847688,-20.1859001877882,-3.06988801276916));
#38928=CARTESIAN_POINT('Ctrl Pts',(371.651977109528,-20.1754685757687,-3.12297961441169));
#38929=CARTESIAN_POINT('Ctrl Pts',(371.404535398339,-20.1609166793302,-3.17255024325987));
#38930=CARTESIAN_POINT('Ctrl Pts',(371.34135098151,-20.1571787823768,-3.18325930020289));
#38931=CARTESIAN_POINT('Ctrl Pts',(371.232490240739,-20.1506715972725,-3.19838669300094));
#38932=CARTESIAN_POINT('Ctrl Pts',(371.186960858635,-20.1479302173056,-3.20372615604336));
#38933=CARTESIAN_POINT('Ctrl Pts',(371.121947881511,-20.1439808191757,-3.20994794684186));
#38934=CARTESIAN_POINT('Ctrl Pts',(371.102544953445,-20.1427977389029,-3.21162747708565));
#38935=CARTESIAN_POINT('Ctrl Pts',(371.068921453156,-20.1407394726026,-3.21423113024819));
#38936=CARTESIAN_POINT('Ctrl Pts',(371.054707632188,-20.1398668716245,-3.21523699636672));
#38937=CARTESIAN_POINT('Ctrl Pts',(371.025588030514,-20.1380738748322,-3.2171036969262));
#38938=CARTESIAN_POINT('Ctrl Pts',(371.010682022249,-20.1371532108741,-3.21795527399319));
#38939=CARTESIAN_POINT('Ctrl Pts',(370.972904651007,-20.1348124512563,-3.2198502200869));
#38940=CARTESIAN_POINT('Ctrl Pts',(370.950027386388,-20.1333880101405,-3.22075348339693));
#38941=CARTESIAN_POINT('Ctrl Pts',(370.862856605748,-20.1279329819469,-3.22326531046257));
#38942=CARTESIAN_POINT('Ctrl Pts',(370.798533274687,-20.1238506028816,-3.22319286401706));
#38943=CARTESIAN_POINT('Ctrl Pts',(370.452629574746,-20.1015777275565,-3.21244814636443));
#38944=CARTESIAN_POINT('Ctrl Pts',(370.17339313524,-20.0823066110808,-3.16680231692582));
#38945=CARTESIAN_POINT('Ctrl Pts',(369.825493601141,-20.057908035134,-3.06187307237525));
#38946=CARTESIAN_POINT('Ctrl Pts',(369.748190429484,-20.0524724400234,-3.03531250696704));
#38947=CARTESIAN_POINT('Ctrl Pts',(369.629179937456,-20.0441609566835,-2.98929181104623));
#38948=CARTESIAN_POINT('Ctrl Pts',(369.58673964208,-20.0412088073997,-2.97182974545993));
#38949=CARTESIAN_POINT('Ctrl Pts',(369.532224073778,-20.0374452087341,-2.94802547686855));
#38950=CARTESIAN_POINT('Ctrl Pts',(369.519798107862,-20.0365893079822,-2.94250578200464));
#38951=CARTESIAN_POINT('Ctrl Pts',(369.499669342575,-20.0352064603573,-2.93341149719189));
#38952=CARTESIAN_POINT('Ctrl Pts',(369.491945234246,-20.034676685613,-2.92988488077386));
#38953=CARTESIAN_POINT('Ctrl Pts',(369.477008568169,-20.0336540439749,-2.9229937401109));
#38954=CARTESIAN_POINT('Ctrl Pts',(369.469794439684,-20.0331609671482,-2.91963298297711));
#38955=CARTESIAN_POINT('Ctrl Pts',(369.453857423651,-20.0320734047485,-2.91213663041633));
#38956=CARTESIAN_POINT('Ctrl Pts',(369.445140444403,-20.0314796853285,-2.9079884601214));
#38957=CARTESIAN_POINT('Ctrl Pts',(369.414272193598,-20.029380817066,-2.89312863421641));
#38958=CARTESIAN_POINT('Ctrl Pts',(369.39222446503,-20.0278882790643,-2.882202233137));
#38959=CARTESIAN_POINT('Ctrl Pts',(369.160005631377,-20.0122155176577,-2.76378742624917));
#38960=CARTESIAN_POINT('Ctrl Pts',(368.962095480527,-19.999236407559,-2.63375365515045));
#38961=CARTESIAN_POINT('Ctrl Pts',(368.621799398861,-19.9745009324386,-2.35225682265025));
#38962=CARTESIAN_POINT('Ctrl Pts',(368.476362989442,-19.962856822136,-2.20644138951225));
#38963=CARTESIAN_POINT('Ctrl Pts',(368.326596185414,-19.9487476522049,-2.02444152885311));
#38964=CARTESIAN_POINT('Ctrl Pts',(368.307716960025,-19.9469254568871,-2.00082965282536));
#38965=CARTESIAN_POINT('Ctrl Pts',(368.27903925908,-19.9440870192184,-1.96390981840097));
#38966=CARTESIAN_POINT('Ctrl Pts',(368.269005965348,-19.9430800944763,-1.95078583411237));
#38967=CARTESIAN_POINT('Ctrl Pts',(368.251526324454,-19.9413009462858,-1.92755365391943));
#38968=CARTESIAN_POINT('Ctrl Pts',(368.24403725733,-19.9405304179593,-1.91747792615612));
#38969=CARTESIAN_POINT('Ctrl Pts',(368.227071474119,-19.9387657040422,-1.8943715272601));
#38970=CARTESIAN_POINT('Ctrl Pts',(368.217633283635,-19.9377700528415,-1.88131310867088));
#38971=CARTESIAN_POINT('Ctrl Pts',(368.192302682442,-19.9350594124727,-1.8457070060361));
#38972=CARTESIAN_POINT('Ctrl Pts',(368.176601492659,-19.9333371906028,-1.82302555811161));
#38973=CARTESIAN_POINT('Ctrl Pts',(368.096537895935,-19.9243306158851,-1.70413523511091));
#38974=CARTESIAN_POINT('Ctrl Pts',(368.037108747733,-19.9168651079502,-1.60472176121304));
#38975=CARTESIAN_POINT('Ctrl Pts',(367.875961596529,-19.8941001017526,-1.29889422203756));
#38976=CARTESIAN_POINT('Ctrl Pts',(367.790851163987,-19.8783552716304,-1.0845698119118));
#38977=CARTESIAN_POINT('Ctrl Pts',(367.699573020366,-19.8555214847328,-0.756172554428587));
#38978=CARTESIAN_POINT('Ctrl Pts',(367.675401654138,-19.8481967618234,-0.647823872396063));
#38979=CARTESIAN_POINT('Ctrl Pts',(367.653944128462,-19.8400291793497,-0.521196874538539));
#38980=CARTESIAN_POINT('Ctrl Pts',(367.651163459427,-19.8389242235019,-0.503935857255061));
#38981=CARTESIAN_POINT('Ctrl Pts',(367.647112956313,-19.8372405672459,-0.477419878440386));
#38982=CARTESIAN_POINT('Ctrl Pts',(367.645742711021,-19.8366564851984,-0.468180908321821));
#38983=CARTESIAN_POINT('Ctrl Pts',(367.643297812703,-19.8355870139964,-0.451187265802331));
#38984=CARTESIAN_POINT('Ctrl Pts',(367.642211249176,-19.8351009850683,-0.443434638433489));
#38985=CARTESIAN_POINT('Ctrl Pts',(367.639816647838,-19.8340048924913,-0.425884155100602));
#38986=CARTESIAN_POINT('Ctrl Pts',(367.638525430672,-19.8333957760794,-0.41608420154635));
#38987=CARTESIAN_POINT('Ctrl Pts',(367.635298956339,-19.8318249115421,-0.390694800896339));
#38988=CARTESIAN_POINT('Ctrl Pts',(367.633432530947,-19.830866873789,-0.375096662570071));
#38989=CARTESIAN_POINT('Ctrl Pts',(367.621818520877,-19.8245547031182,-0.27162794779574));
#38990=CARTESIAN_POINT('Ctrl Pts',(367.615575338699,-19.8193763009762,-0.183393693137639));
#38991=CARTESIAN_POINT('Ctrl Pts',(367.612059119699,-19.812522347707,-0.064170820373583));
#38992=CARTESIAN_POINT('Ctrl Pts',(367.61159246942,-19.8107618795412,-0.0333228726335784));
#38993=CARTESIAN_POINT('Ctrl Pts',(367.611365393164,-19.7939561659989,0.262665895764635));
#38994=CARTESIAN_POINT('Ctrl Pts',(367.643879954345,-19.7795271327586,0.526807229265741));
#38995=CARTESIAN_POINT('Ctrl Pts',(367.727498015159,-19.7595540549841,0.860211327451352));
#38996=CARTESIAN_POINT('Ctrl Pts',(367.749395193941,-19.7549171119708,0.935704950494251));
#38997=CARTESIAN_POINT('Ctrl Pts',(367.781754144639,-19.7487086465045,1.03372130521205));
#38998=CARTESIAN_POINT('Ctrl Pts',(367.789748227104,-19.7472178308891,1.05703390297856));
#38999=CARTESIAN_POINT('Ctrl Pts',(367.803140493652,-19.7447865904906,1.09467610087256));
#39000=CARTESIAN_POINT('Ctrl Pts',(367.808374903739,-19.7438516044097,1.10906321045882));
#39001=CARTESIAN_POINT('Ctrl Pts',(367.818623883133,-19.7420494110642,1.13662044129997));
#39002=CARTESIAN_POINT('Ctrl Pts',(367.82362272606,-19.7411827458648,1.14979606455863));
#39003=CARTESIAN_POINT('Ctrl Pts',(367.835377841904,-19.7391725523392,1.18017712122158));
#39004=CARTESIAN_POINT('Ctrl Pts',(367.84219599776,-19.7380269675883,1.19735792818893));
#39005=CARTESIAN_POINT('Ctrl Pts',(367.864300968917,-19.7343755915541,1.25169135355113));
#39006=CARTESIAN_POINT('Ctrl Pts',(367.880134398117,-19.7318514714104,1.28861608597521));
#39007=CARTESIAN_POINT('Ctrl Pts',(367.965273786669,-19.7187233157166,1.47734575648011));
#39008=CARTESIAN_POINT('Ctrl Pts',(368.0455947568,-19.7077453239286,1.6238760508442));
#39009=CARTESIAN_POINT('Ctrl Pts',(368.205904771585,-19.6880831628653,1.86908292525594));
#39010=CARTESIAN_POINT('Ctrl Pts',(368.281061349241,-19.6795146878501,1.97050917442894));
#39011=CARTESIAN_POINT('Ctrl Pts',(368.452653694803,-19.6614781278235,2.17572537289477));
#39012=CARTESIAN_POINT('Ctrl Pts',(368.550390997389,-19.6520451176192,2.27811153420839));
#39013=CARTESIAN_POINT('Ctrl Pts',(368.668218219015,-19.6418564832114,2.38630979085417));
#39014=CARTESIAN_POINT('Ctrl Pts',(368.681997526511,-19.6406819886341,2.39874535793091));
#39015=CARTESIAN_POINT('Ctrl Pts',(368.703130056975,-19.6389074733238,2.41748835592149));
#39016=CARTESIAN_POINT('Ctrl Pts',(368.710405290203,-19.6383013140247,2.42388258879763));
#39017=CARTESIAN_POINT('Ctrl Pts',(368.723607269034,-19.6372100758334,2.43538078420053));
#39018=CARTESIAN_POINT('Ctrl Pts',(368.729523824179,-19.6367241802063,2.44049602190619));
#39019=CARTESIAN_POINT('Ctrl Pts',(368.7426786172,-19.6356507974017,2.45178575303565));
#39020=CARTESIAN_POINT('Ctrl Pts',(368.749925593552,-19.6350640731383,2.45794975247521));
#39021=CARTESIAN_POINT('Ctrl Pts',(368.771201559347,-19.6333545932458,2.47588450354414));
#39022=CARTESIAN_POINT('Ctrl Pts',(368.785303971363,-19.6322379607947,2.48756810250515));
#39023=CARTESIAN_POINT('Ctrl Pts',(368.912946411962,-19.6222702335846,2.59149558261916));
#39024=CARTESIAN_POINT('Ctrl Pts',(369.032559796952,-19.6139059631413,2.67604116914777));
#39025=CARTESIAN_POINT('Ctrl Pts',(369.358668816137,-19.5923961636063,2.8747275213872));
#39026=CARTESIAN_POINT('Ctrl Pts',(369.572636943486,-19.5794631856752,2.97485406524251));
#39027=CARTESIAN_POINT('Ctrl Pts',(369.870788610753,-19.5611693233384,3.07636746945026));
#39028=CARTESIAN_POINT('Ctrl Pts',(369.946887712082,-19.556484341736,3.09917596190114));
#39029=CARTESIAN_POINT('Ctrl Pts',(370.047690384361,-19.5502204166709,3.12537146155126));
#39030=CARTESIAN_POINT('Ctrl Pts',(370.071703779854,-19.548724045934,3.13131749755412));
#39031=CARTESIAN_POINT('Ctrl Pts',(370.110704966837,-19.5462859811946,3.14049947741603));
#39032=CARTESIAN_POINT('Ctrl Pts',(370.125651853903,-19.5453497836919,3.14390602049039));
#39033=CARTESIAN_POINT('Ctrl Pts',(370.154377861132,-19.5435467851678,3.15023770190342));
#39034=CARTESIAN_POINT('Ctrl Pts',(370.168152997817,-19.5426805379087,3.1531794028812));
#39035=CARTESIAN_POINT('Ctrl Pts',(370.200004517233,-19.5406735690553,3.15976330883456));
#39036=CARTESIAN_POINT('Ctrl Pts',(370.218093623182,-19.5395308124168,3.16334083711164));
#39037=CARTESIAN_POINT('Ctrl Pts',(370.27544858307,-19.5358976308321,3.17417345409311));
#39038=CARTESIAN_POINT('Ctrl Pts',(370.314817868995,-19.5333891342309,3.1808538970289));
#39039=CARTESIAN_POINT('Ctrl Pts',(370.517265537148,-19.5204097959917,3.21134797236672));
#39040=CARTESIAN_POINT('Ctrl Pts',(370.681850536276,-19.5095746299259,3.22335504829115));
#39041=CARTESIAN_POINT('Ctrl Pts',(371.005336752247,-19.4878740285333,3.2221210794355));
#39042=CARTESIAN_POINT('Ctrl Pts',(371.163796609833,-19.4770561089891,3.20979035701147));
#39043=CARTESIAN_POINT('Ctrl Pts',(371.431353970829,-19.458913215028,3.16894223643924));
#39044=CARTESIAN_POINT('Ctrl Pts',(371.541063953601,-19.4515146343037,3.14629341435928));
#39045=CARTESIAN_POINT('Ctrl Pts',(371.665391850588,-19.4433339887412,3.11379308502182));
#39046=CARTESIAN_POINT('Ctrl Pts',(371.681368822718,-19.442286697041,3.10948485238336));
#39047=CARTESIAN_POINT('Ctrl Pts',(371.706973835975,-19.4406154671804,3.10236839437006));
#39048=CARTESIAN_POINT('Ctrl Pts',(371.716622951791,-19.4399873184542,3.09963801725236));
#39049=CARTESIAN_POINT('Ctrl Pts',(371.733804595024,-19.4388719425498,3.09468945414974));
#39050=CARTESIAN_POINT('Ctrl Pts',(371.741341938866,-19.4383837318602,3.09248872738467));
#39051=CARTESIAN_POINT('Ctrl Pts',(371.757607141006,-19.4373325908181,3.0876750882068));
#39052=CARTESIAN_POINT('Ctrl Pts',(371.766331991843,-19.4367702142016,3.08505270772787));
#39053=CARTESIAN_POINT('Ctrl Pts',(371.790740739503,-19.4352007158312,3.07760330496356));
#39054=CARTESIAN_POINT('Ctrl Pts',(371.806399314343,-19.4341982812127,3.07269336236137));
#39055=CARTESIAN_POINT('Ctrl Pts',(371.902341188907,-19.4280795719444,3.0418027544764));
#39056=CARTESIAN_POINT('Ctrl Pts',(371.981623171483,-19.4231237218335,3.01279454187252));
#39057=CARTESIAN_POINT('Ctrl Pts',(372.144736803546,-19.4129626901145,2.94573874203487));
#39058=CARTESIAN_POINT('Ctrl Pts',(372.228190025311,-19.4077836670407,2.90717539528309));
#39059=CARTESIAN_POINT('Ctrl Pts',(372.309820886087,-19.4026365087528,2.86513670921865));
#39060=CARTESIAN_POINT('',(367.611568037796,-19.5613959703564,-0.00109071397770461));
#39061=CARTESIAN_POINT('Ctrl Pts',(372.309820613636,-19.1541342831958,2.86513684952685));
#39062=CARTESIAN_POINT('Ctrl Pts',(372.306868563801,-19.154338301629,2.86665711117884));
#39063=CARTESIAN_POINT('Ctrl Pts',(372.303914169137,-19.1545424807628,2.86817280799209));
#39064=CARTESIAN_POINT('Ctrl Pts',(372.286842891529,-19.1557222807326,2.87689760560397));
#39065=CARTESIAN_POINT('Ctrl Pts',(372.272675520473,-19.1567013873833,2.88400693944335));
#39066=CARTESIAN_POINT('Ctrl Pts',(372.234157867628,-19.1593636287487,2.90298108729884));
#39067=CARTESIAN_POINT('Ctrl Pts',(372.209709935956,-19.1610537251766,2.91464368421585));
#39068=CARTESIAN_POINT('Ctrl Pts',(372.077029171251,-19.170229932089,2.97589641095051));
#39069=CARTESIAN_POINT('Ctrl Pts',(371.966270420312,-19.1779090706688,3.01976298846185));
#39070=CARTESIAN_POINT('Ctrl Pts',(371.705181375476,-19.1960434975514,3.10678403213363));
#39071=CARTESIAN_POINT('Ctrl Pts',(371.553629055342,-19.2065994500682,3.14532905088503));
#39072=CARTESIAN_POINT('Ctrl Pts',(371.234911433396,-19.2284994398373,3.20214398956842));
#39073=CARTESIAN_POINT('Ctrl Pts',(371.067871282371,-19.2398114594399,3.21864331106934));
#39074=CARTESIAN_POINT('Ctrl Pts',(370.873352244017,-19.2523116063804,3.22262625248144));
#39075=CARTESIAN_POINT('Ctrl Pts',(370.84640504265,-19.2540280054567,3.22283999864873));
#39076=CARTESIAN_POINT('Ctrl Pts',(370.809127970701,-19.2563783556098,3.22266810737568));
#39077=CARTESIAN_POINT('Ctrl Pts',(370.798798731968,-19.2570270718949,3.22257081525373));
#39078=CARTESIAN_POINT('Ctrl Pts',(370.781061466026,-19.2581364550607,3.22231845366809));
#39079=CARTESIAN_POINT('Ctrl Pts',(370.773653253057,-19.2585984301872,3.22218749742093));
#39080=CARTESIAN_POINT('Ctrl Pts',(370.758146765737,-19.2595624430543,3.22185988928937));
#39081=CARTESIAN_POINT('Ctrl Pts',(370.750048691387,-19.260064181351,3.22165825172853));
#39082=CARTESIAN_POINT('Ctrl Pts',(370.730205278945,-19.2612896335181,3.22108929076979));
#39083=CARTESIAN_POINT('Ctrl Pts',(370.718460878824,-19.2620114885945,3.22068825232257));
#39084=CARTESIAN_POINT('Ctrl Pts',(370.675749817811,-19.2646250284017,3.21899585580073));
#39085=CARTESIAN_POINT('Ctrl Pts',(370.644798918115,-19.2664966826415,3.21732200378132));
#39086=CARTESIAN_POINT('Ctrl Pts',(370.567079628982,-19.2711512312952,3.21199337808265));
#39087=CARTESIAN_POINT('Ctrl Pts',(370.520356822767,-19.2739081608776,3.20776349441411));
#39088=CARTESIAN_POINT('Ctrl Pts',(370.138209401912,-19.2962378896698,3.16473681101626));
#39089=CARTESIAN_POINT('Ctrl Pts',(369.810690838872,-19.3142183830495,3.0744680851715));
#39090=CARTESIAN_POINT('Ctrl Pts',(369.446006032172,-19.3376778537739,2.90906223356186));
#39091=CARTESIAN_POINT('Ctrl Pts',(369.389648081856,-19.3414010942409,2.88148941811556));
#39092=CARTESIAN_POINT('Ctrl Pts',(369.314056166936,-19.3465480431571,2.84173126140242));
#39093=CARTESIAN_POINT('Ctrl Pts',(369.294091585639,-19.3479222816126,2.83096011295208));
#39094=CARTESIAN_POINT('Ctrl Pts',(369.262513704432,-19.3501204585051,2.81349052874243));
#39095=CARTESIAN_POINT('Ctrl Pts',(369.250825385868,-19.3509395157766,2.80692871922191));
#39096=CARTESIAN_POINT('Ctrl Pts',(369.227155683611,-19.3526093862186,2.79344568118483));
#39097=CARTESIAN_POINT('Ctrl Pts',(369.215177269395,-19.3534603533395,2.7865198318835));
#39098=CARTESIAN_POINT('Ctrl Pts',(369.187673174213,-19.3554281337958,2.77037990221073));
#39099=CARTESIAN_POINT('Ctrl Pts',(369.172179690717,-19.3565468800844,2.76111213263311));
#39100=CARTESIAN_POINT('Ctrl Pts',(369.139744408855,-19.3589109716653,2.74133831938517));
#39101=CARTESIAN_POINT('Ctrl Pts',(369.122820633625,-19.3601573102741,2.73080430977802));
#39102=CARTESIAN_POINT('Ctrl Pts',(369.077890326319,-19.3635010200687,2.70225623105007));
#39103=CARTESIAN_POINT('Ctrl Pts',(369.050064021607,-19.3656085054049,2.68396433053046));
#39104=CARTESIAN_POINT('Ctrl Pts',(368.879690998772,-19.3787435614883,2.56814747924556));
#39105=CARTESIAN_POINT('Ctrl Pts',(368.744911698469,-19.3901742471553,2.45973866842112));
#39106=CARTESIAN_POINT('Ctrl Pts',(368.466698470098,-19.415961837233,2.19652714471642));
#39107=CARTESIAN_POINT('Ctrl Pts',(368.328429068574,-19.4303616533602,2.03737099911767));
#39108=CARTESIAN_POINT('Ctrl Pts',(368.179494482557,-19.447138021473,1.82762972744126));
#39109=CARTESIAN_POINT('Ctrl Pts',(368.153174945853,-19.4501592887267,1.78879590508509));
#39110=CARTESIAN_POINT('Ctrl Pts',(368.119978809347,-19.4540320448328,1.73743604769735));
#39111=CARTESIAN_POINT('Ctrl Pts',(368.112325789226,-19.4549294039006,1.72542159660882));
#39112=CARTESIAN_POINT('Ctrl Pts',(368.100159844046,-19.4563627899728,1.70603990841662));
#39113=CARTESIAN_POINT('Ctrl Pts',(368.095596544341,-19.4569020230972,1.69870473734099));
#39114=CARTESIAN_POINT('Ctrl Pts',(368.086871297713,-19.4579360016838,1.68455298847506));
#39115=CARTESIAN_POINT('Ctrl Pts',(368.08270515164,-19.4584310055976,1.67773921928313));
#39116=CARTESIAN_POINT('Ctrl Pts',(368.072792092752,-19.459612108242,1.66139007581286));
#39117=CARTESIAN_POINT('Ctrl Pts',(368.067069116106,-19.4602966600066,1.6518401693799));
#39118=CARTESIAN_POINT('Ctrl Pts',(368.047620411075,-19.4626329618374,1.6190014439291));
#39119=CARTESIAN_POINT('Ctrl Pts',(368.034137851771,-19.4642698374452,1.59556898258199));
#39120=CARTESIAN_POINT('Ctrl Pts',(368.001899206718,-19.468233904188,1.53787119067329));
#39121=CARTESIAN_POINT('Ctrl Pts',(367.983467789884,-19.4705439558542,1.50342853917158));
#39122=CARTESIAN_POINT('Ctrl Pts',(367.91124321529,-19.4798137931502,1.36235610529661));
#39123=CARTESIAN_POINT('Ctrl Pts',(367.86276681526,-19.4865572697705,1.25310337091742));
#39124=CARTESIAN_POINT('Ctrl Pts',(367.738655482965,-19.5062050327462,0.925390214173588));
#39125=CARTESIAN_POINT('Ctrl Pts',(367.680312770581,-19.5189718213504,0.701224908475511));
#39126=CARTESIAN_POINT('Ctrl Pts',(367.637213578117,-19.5361834239919,0.410597412293125));
#39127=CARTESIAN_POINT('Ctrl Pts',(367.629816262804,-19.5399128189062,0.348187819863735));
#39128=CARTESIAN_POINT('Ctrl Pts',(367.622238257198,-19.5450658167484,0.263014439344415));
#39129=CARTESIAN_POINT('Ctrl Pts',(367.620466919147,-19.5464397530616,0.240403951145996));
#39130=CARTESIAN_POINT('Ctrl Pts',(367.618028679303,-19.5486375673944,0.204404405759115));
#39131=CARTESIAN_POINT('Ctrl Pts',(367.617206395823,-19.5494565672057,0.191026368648337));
#39132=CARTESIAN_POINT('Ctrl Pts',(367.615724633287,-19.5511044386181,0.164185626947726));
#39133=CARTESIAN_POINT('Ctrl Pts',(367.615066113935,-19.5519333231276,0.150723142999138));
#39134=CARTESIAN_POINT('Ctrl Pts',(367.613908855636,-19.5536096990944,0.123575763942133));
#39135=CARTESIAN_POINT('Ctrl Pts',(367.613412851242,-19.5544572586867,0.109891037489478));
#39136=CARTESIAN_POINT('Ctrl Pts',(367.612530157003,-19.5562933996043,0.0803346467455371));
#39137=CARTESIAN_POINT('Ctrl Pts',(367.612173507387,-19.557282899167,0.0644625091245308));
#39138=CARTESIAN_POINT('Ctrl Pts',(367.61168447067,-19.5593120843888,0.032029723451429));
#39139=CARTESIAN_POINT('Ctrl Pts',(367.611562433136,-19.5603520594605,0.0154694610957346));
#39140=CARTESIAN_POINT('Ctrl Pts',(367.611568037796,-19.5613959703564,-0.00109071397770461));
#39141=CARTESIAN_POINT('Ctrl Pts',(367.61156803705,-19.5613958313854,-0.00108850939768229));
#39142=CARTESIAN_POINT('Ctrl Pts',(367.611585009097,-19.5645634070565,-0.0513376498611552));
#39143=CARTESIAN_POINT('Ctrl Pts',(367.612777200739,-19.5677668500842,-0.10157770103759));
#39144=CARTESIAN_POINT('Ctrl Pts',(367.626998441497,-19.5872241200623,-0.403227078336578));
#39145=CARTESIAN_POINT('Ctrl Pts',(367.66827534513,-19.6043279925662,-0.652401396010281));
#39146=CARTESIAN_POINT('Ctrl Pts',(367.7786981762,-19.6311772852115,-1.03475273693346));
#39147=CARTESIAN_POINT('Ctrl Pts',(367.828824469343,-19.6409513883906,-1.17240952248012));
#39148=CARTESIAN_POINT('Ctrl Pts',(367.895565317816,-19.651433745654,-1.32294626623134));
#39149=CARTESIAN_POINT('Ctrl Pts',(367.903134556563,-19.6525926603946,-1.33963345938175));
#39150=CARTESIAN_POINT('Ctrl Pts',(367.914852287953,-19.6543411352039,-1.36489157306516));
#39151=CARTESIAN_POINT('Ctrl Pts',(367.918896975249,-19.6549367151184,-1.37350984807355));
#39152=CARTESIAN_POINT('Ctrl Pts',(367.926336632082,-19.6560176775914,-1.38918106995364));
#39153=CARTESIAN_POINT('Ctrl Pts',(367.929719120598,-19.6565037901847,-1.39623960441441));
#39154=CARTESIAN_POINT('Ctrl Pts',(367.937348660056,-19.6575883984911,-1.41201311537138));
#39155=CARTESIAN_POINT('Ctrl Pts',(367.941609331193,-19.6581860431998,-1.42072128034461));
#39156=CARTESIAN_POINT('Ctrl Pts',(367.954150849471,-19.6599223661703,-1.44606392042762));
#39157=CARTESIAN_POINT('Ctrl Pts',(367.962536500583,-19.6610547756491,-1.46264648198441));
#39158=CARTESIAN_POINT('Ctrl Pts',(368.036875327732,-19.6708570192796,-1.60654667233671));
#39159=CARTESIAN_POINT('Ctrl Pts',(368.111122418866,-19.6790616618526,-1.72942007047729));
#39160=CARTESIAN_POINT('Ctrl Pts',(368.35406351278,-19.7029510255846,-2.07680744285875));
#39161=CARTESIAN_POINT('Ctrl Pts',(368.544113137892,-19.7182955623904,-2.284676478965));
#39162=CARTESIAN_POINT('Ctrl Pts',(368.783521402744,-19.7368044940429,-2.48624352627725));
#39163=CARTESIAN_POINT('Ctrl Pts',(368.808687217269,-19.7387395349292,-2.50678945455595));
#39164=CARTESIAN_POINT('Ctrl Pts',(368.849531102628,-19.7418662105282,-2.5391186427375));
#39165=CARTESIAN_POINT('Ctrl Pts',(368.865013959996,-19.7430483310722,-2.5511456402404));
#39166=CARTESIAN_POINT('Ctrl Pts',(368.894571255231,-19.7452997871051,-2.57367617952947));
#39167=CARTESIAN_POINT('Ctrl Pts',(368.908623734446,-19.7463679930637,-2.58420743816429));
#39168=CARTESIAN_POINT('Ctrl Pts',(368.923020921186,-19.747460375822,-2.59481438719899));
#39169=CARTESIAN_POINT('Ctrl Pts',(368.923280502528,-19.7474800708206,-2.59500557045182));
#39170=CARTESIAN_POINT('Ctrl Pts',(368.923802633112,-19.7475196846589,-2.59539000200284));
#39171=CARTESIAN_POINT('Ctrl Pts',(368.924065183248,-19.7475396035514,-2.59558324960454));
#39172=CARTESIAN_POINT('Ctrl Pts',(368.924443840134,-19.7475683301349,-2.5958618679334));
#39173=CARTESIAN_POINT('Ctrl Pts',(368.924559923217,-19.7475771365773,-2.59594727065917));
#39174=CARTESIAN_POINT('Ctrl Pts',(368.924800958579,-19.7475954220328,-2.59612457629137));
#39175=CARTESIAN_POINT('Ctrl Pts',(368.924925911978,-19.7476049011099,-2.59621647812081));
#39176=CARTESIAN_POINT('Ctrl Pts',(368.925185691327,-19.7476246078851,-2.59640751403123));
#39177=CARTESIAN_POINT('Ctrl Pts',(368.925320517877,-19.7476348356036,-2.59650664627378));
#39178=CARTESIAN_POINT('Ctrl Pts',(368.925601203812,-19.7476561276013,-2.59671298905518));
#39179=CARTESIAN_POINT('Ctrl Pts',(368.925747065573,-19.7476671920303,-2.59682019858774));
#39180=CARTESIAN_POINT('Ctrl Pts',(368.926051182247,-19.747690260543,-2.59704368725327));
#39181=CARTESIAN_POINT('Ctrl Pts',(368.926209438383,-19.7477022646824,-2.59715996393718));
#39182=CARTESIAN_POINT('Ctrl Pts',(368.926539942212,-19.7477273337446,-2.59740275090876));
#39183=CARTESIAN_POINT('Ctrl Pts',(368.926712191508,-19.7477403987438,-2.59752925826852));
#39184=CARTESIAN_POINT('Ctrl Pts',(368.937671468353,-19.7485716344314,-2.60557654887377));
#39185=CARTESIAN_POINT('Ctrl Pts',(368.94850758579,-19.7493923913792,-2.61342998528496));
#39186=CARTESIAN_POINT('Ctrl Pts',(368.97216676901,-19.7511821096357,-2.6303531296322));
#39187=CARTESIAN_POINT('Ctrl Pts',(368.98500780431,-19.7521520344117,-2.63939700993301));
#39188=CARTESIAN_POINT('Ctrl Pts',(369.019627670078,-19.7547634145558,-2.66340294915108));
#39189=CARTESIAN_POINT('Ctrl Pts',(369.0415248915,-19.7564113849455,-2.6781913785143));
#39190=CARTESIAN_POINT('Ctrl Pts',(369.143440881046,-19.7640661878629,-2.74521102102542));
#39191=CARTESIAN_POINT('Ctrl Pts',(369.225568902198,-19.7701937221241,-2.79413175576221));
#39192=CARTESIAN_POINT('Ctrl Pts',(369.527797089775,-19.7926043616879,-2.95641298873467));
#39193=CARTESIAN_POINT('Ctrl Pts',(369.758600723709,-19.8095442447405,-3.04797974859762));
#39194=CARTESIAN_POINT('Ctrl Pts',(370.109681646012,-19.8339313546563,-3.14237161758454));
#39195=CARTESIAN_POINT('Ctrl Pts',(370.223360936712,-19.841611452251,-3.16643877024317));
#39196=CARTESIAN_POINT('Ctrl Pts',(370.355541697904,-19.8501205690991,-3.18703662900512));
#39197=CARTESIAN_POINT('Ctrl Pts',(370.373003618394,-19.851236254454,-3.18961099367103));
#39198=CARTESIAN_POINT('Ctrl Pts',(370.39977619719,-19.8529330309967,-3.19333353771929));
#39199=CARTESIAN_POINT('Ctrl Pts',(370.409071869014,-19.8535196267109,-3.19458469790623));
#39200=CARTESIAN_POINT('Ctrl Pts',(370.426139965871,-19.8545918716988,-3.19680617528343));
#39201=CARTESIAN_POINT('Ctrl Pts',(370.433910469346,-19.8550781785161,-3.19778874215249));
#39202=CARTESIAN_POINT('Ctrl Pts',(370.451464628769,-19.8561726547757,-3.19994344609137));
#39203=CARTESIAN_POINT('Ctrl Pts',(370.461250115588,-19.8567798945841,-3.20109904857294));
#39204=CARTESIAN_POINT('Ctrl Pts',(370.486534691424,-19.8583418772711,-3.20396747517877));
#39205=CARTESIAN_POINT('Ctrl Pts',(370.5020413892,-19.8592929828154,-3.20561274691841));
#39206=CARTESIAN_POINT('Ctrl Pts',(370.603799126536,-19.8654930779212,-3.21566298835883));
#39207=CARTESIAN_POINT('Ctrl Pts',(370.690355141666,-19.8705732047546,-3.22069943406989));
#39208=CARTESIAN_POINT('Ctrl Pts',(371.063649729496,-19.8920464373321,-3.22733777508927));
#39209=CARTESIAN_POINT('Ctrl Pts',(371.349684506944,-19.9075115236879,-3.19416930597227));
#39210=CARTESIAN_POINT('Ctrl Pts',(371.71432318891,-19.9292753464472,-3.10156718149705));
#39211=CARTESIAN_POINT('Ctrl Pts',(371.800110644108,-19.9345406849459,-3.07593409277145));
#39212=CARTESIAN_POINT('Ctrl Pts',(371.908227008078,-19.9414178771559,-3.03866010010499));
#39213=CARTESIAN_POINT('Ctrl Pts',(371.931643750064,-19.9429220731663,-3.03028247859762));
#39214=CARTESIAN_POINT('Ctrl Pts',(371.969368109949,-19.9453702030028,-3.01629153130544));
#39215=CARTESIAN_POINT('Ctrl Pts',(371.983736922314,-19.9463085617691,-3.01084530952918));
#39216=CARTESIAN_POINT('Ctrl Pts',(372.011204387882,-19.9481138993346,-3.00020901717105));
#39217=CARTESIAN_POINT('Ctrl Pts',(372.024309058994,-19.9489803094843,-2.99503538916531));
#39218=CARTESIAN_POINT('Ctrl Pts',(372.054163799418,-19.9509659881961,-2.9830220864592));
#39219=CARTESIAN_POINT('Ctrl Pts',(372.070890922978,-19.9520871066675,-2.97612700040191));
#39220=CARTESIAN_POINT('Ctrl Pts',(372.123555899257,-19.9556445835641,-2.9538973367222));
#39221=CARTESIAN_POINT('Ctrl Pts',(372.159272326135,-19.9580982242592,-2.93805031346501));
#39222=CARTESIAN_POINT('Ctrl Pts',(372.433251001694,-19.9772472490339,-2.81047691871032));
#39223=CARTESIAN_POINT('Ctrl Pts',(372.657266714198,-19.9949613950613,-2.67061301510547));
#39224=CARTESIAN_POINT('Ctrl Pts',(372.955891055772,-20.0209421681235,-2.4289324677483));
#39225=CARTESIAN_POINT('Ctrl Pts',(373.045670720648,-20.029108080863,-2.34748967144073));
#39226=CARTESIAN_POINT('Ctrl Pts',(373.158292218291,-20.0396443879272,-2.23311711524096));
#39227=CARTESIAN_POINT('Ctrl Pts',(373.185411852564,-20.0422058564334,-2.20454670814433));
#39228=CARTESIAN_POINT('Ctrl Pts',(373.230365388343,-20.0464831161929,-2.15541499266873));
#39229=CARTESIAN_POINT('Ctrl Pts',(373.248474554539,-20.0482151911012,-2.13511243647799));
#39230=CARTESIAN_POINT('Ctrl Pts',(373.273648468843,-20.0506328592559,-2.10615960508946));
#39231=CARTESIAN_POINT('Ctrl Pts',(373.280928112895,-20.051333181227,-2.09769882975));
#39232=CARTESIAN_POINT('Ctrl Pts',(373.293344167969,-20.0525294442645,-2.08311569631408));
#39233=CARTESIAN_POINT('Ctrl Pts',(373.298501995548,-20.0530269298298,-2.07701178116447));
#39234=CARTESIAN_POINT('Ctrl Pts',(373.308492631924,-20.0539915173376,-2.0650989859083));
#39235=CARTESIAN_POINT('Ctrl Pts',(373.31332774562,-20.0544588028548,-2.0592922602964));
#39236=CARTESIAN_POINT('Ctrl Pts',(373.326501800481,-20.055733430506,-2.04335725019007));
#39237=CARTESIAN_POINT('Ctrl Pts',(373.334799496513,-20.0565378408961,-2.03319483672731));
#39238=CARTESIAN_POINT('Ctrl Pts',(373.366790327903,-20.0596466179166,-1.99352273093183));
#39239=CARTESIAN_POINT('Ctrl Pts',(373.390026032369,-20.0619207088804,-1.96364602190412));
#39240=CARTESIAN_POINT('Ctrl Pts',(373.543470241788,-20.0771022234632,-1.75900670530429));
#39241=CARTESIAN_POINT('Ctrl Pts',(373.656202001614,-20.0891068632888,-1.57181541419065));
#39242=CARTESIAN_POINT('Ctrl Pts',(373.835241957669,-20.1126175572737,-1.19217400150092));
#39243=CARTESIAN_POINT('Ctrl Pts',(373.903964903389,-20.1240487436974,-1.00203633652997));
#39244=CARTESIAN_POINT('Ctrl Pts',(373.962489932576,-20.138023789715,-0.775683997800598));
#39245=CARTESIAN_POINT('Ctrl Pts',(373.970054333592,-20.1399549687382,-0.744515168821039));
#39246=CARTESIAN_POINT('Ctrl Pts',(373.980895132226,-20.1429272757765,-0.696746032019548));
#39247=CARTESIAN_POINT('Ctrl Pts',(373.984508224294,-20.1439576168608,-0.680223650647294));
#39248=CARTESIAN_POINT('Ctrl Pts',(373.990584454607,-20.1457624449378,-0.651350364426154));
#39249=CARTESIAN_POINT('Ctrl Pts',(373.993105578386,-20.1465350601005,-0.639011937670078));
#39250=CARTESIAN_POINT('Ctrl Pts',(373.998630227968,-20.1482834177722,-0.61114236534025));
#39251=CARTESIAN_POINT('Ctrl Pts',(374.001591831354,-20.1492604753915,-0.595603331819884));
#39252=CARTESIAN_POINT('Ctrl Pts',(374.009287361599,-20.1519113522302,-0.553544815837882));
#39253=CARTESIAN_POINT('Ctrl Pts',(374.013803291285,-20.1535920322722,-0.526987211053909));
#39254=CARTESIAN_POINT('Ctrl Pts',(374.033834216395,-20.1616918993334,-0.399539619430839));
#39255=CARTESIAN_POINT('Ctrl Pts',(374.044881567072,-20.1682498748797,-0.298016500369266));
#39256=CARTESIAN_POINT('Ctrl Pts',(374.052182099146,-20.1761072188326,-0.178290132968703));
#39257=CARTESIAN_POINT('Ctrl Pts',(374.053122306004,-20.1772829238742,-0.160423048926655));
#39258=CARTESIAN_POINT('Ctrl Pts',(374.064047482659,-20.1935617809217,0.0863312633924986));
#39259=CARTESIAN_POINT('Ctrl Pts',(374.049744285065,-20.2092512515646,0.315631722763584));
#39260=CARTESIAN_POINT('Ctrl Pts',(373.99880818053,-20.2295533026651,0.614500249161861));
#39261=CARTESIAN_POINT('Ctrl Pts',(373.983840463085,-20.2344675414593,0.687108649114254));
#39262=CARTESIAN_POINT('Ctrl Pts',(373.959583204317,-20.2411624303431,0.787189303701725));
#39263=CARTESIAN_POINT('Ctrl Pts',(373.952408095704,-20.2430239041147,0.815146536385452));
#39264=CARTESIAN_POINT('Ctrl Pts',(373.93924937225,-20.2462371288764,0.863699936251745));
#39265=CARTESIAN_POINT('Ctrl Pts',(373.933434039182,-20.2475968030059,0.88433943766575));
#39266=CARTESIAN_POINT('Ctrl Pts',(373.924565255301,-20.2495830654088,0.914653711071972));
#39267=CARTESIAN_POINT('Ctrl Pts',(373.921671569227,-20.2502183283875,0.924374088810376));
#39268=CARTESIAN_POINT('Ctrl Pts',(373.916456119987,-20.2513407275249,0.94159594525245));
#39269=CARTESIAN_POINT('Ctrl Pts',(373.914152775887,-20.2518289056371,0.949102772740537));
#39270=CARTESIAN_POINT('Ctrl Pts',(373.909103105037,-20.2528830239978,0.965348184213942));
#39271=CARTESIAN_POINT('Ctrl Pts',(373.906346953022,-20.253448386996,0.974083505853382));
#39272=CARTESIAN_POINT('Ctrl Pts',(373.89862162327,-20.2550061329951,0.998209153985737));
#39273=CARTESIAN_POINT('Ctrl Pts',(373.89357370679,-20.2559940490821,1.0135742486666));
#39274=CARTESIAN_POINT('Ctrl Pts',(373.865786598802,-20.2612779666433,1.09605486608285));
#39275=CARTESIAN_POINT('Ctrl Pts',(373.840952392484,-20.2654626067173,1.16244973322412));
#39276=CARTESIAN_POINT('Ctrl Pts',(373.727204371436,-20.2827778366572,1.43845409343994));
#39277=CARTESIAN_POINT('Ctrl Pts',(373.618399207126,-20.2952104635624,1.63916107061131));
#39278=CARTESIAN_POINT('Ctrl Pts',(373.399719065697,-20.317000973493,1.95699615120404));
#39279=CARTESIAN_POINT('Ctrl Pts',(373.300643129428,-20.3260984230423,2.0804681736899));
#39280=CARTESIAN_POINT('Ctrl Pts',(373.173155089046,-20.3373085061491,2.21738557800843));
#39281=CARTESIAN_POINT('Ctrl Pts',(373.153109544783,-20.3390576450781,2.23833943479634));
#39282=CARTESIAN_POINT('Ctrl Pts',(373.121383707644,-20.3418068997686,2.27061927087443));
#39283=CARTESIAN_POINT('Ctrl Pts',(373.109895474686,-20.3427986333407,2.28213246094062));
#39284=CARTESIAN_POINT('Ctrl Pts',(373.089388160715,-20.3445625464153,2.30237551450739));
#39285=CARTESIAN_POINT('Ctrl Pts',(373.080404241571,-20.345333151517,2.31114063409223));
#39286=CARTESIAN_POINT('Ctrl Pts',(373.059580003881,-20.3471146207233,2.33122160263012));
#39287=CARTESIAN_POINT('Ctrl Pts',(373.047704245605,-20.3481270768203,2.34250004523115));
#39288=CARTESIAN_POINT('Ctrl Pts',(373.014763623252,-20.3509261840192,2.37330971176742));
#39289=CARTESIAN_POINT('Ctrl Pts',(372.993523188709,-20.3527208692228,2.39265019954587));
#39290=CARTESIAN_POINT('Ctrl Pts',(372.870477583172,-20.3630624541511,2.50171657938173));
#39291=CARTESIAN_POINT('Ctrl Pts',(372.763357000183,-20.3718623029062,2.58521409458497));
#39292=CARTESIAN_POINT('Ctrl Pts',(372.541704365468,-20.3896579703631,2.7365231665723));
#39293=CARTESIAN_POINT('Ctrl Pts',(372.427652359241,-20.398622957923,2.80445528357387));
#39294=CARTESIAN_POINT('Ctrl Pts',(372.309820109182,-20.4075893673377,2.8651371093129));
#39295=CARTESIAN_POINT('Origin',(370.834317853224,2.31077344927308,0.));
#39296=CARTESIAN_POINT('',(372.30982061585,-21.9062759889522,2.86513684838664));
#39297=CARTESIAN_POINT('',(372.309820475366,-21.6596622257337,2.86513692073375));
#39298=CARTESIAN_POINT('',(372.309820613641,2.31077344927308,2.86513684952399));
#39299=CARTESIAN_POINT('',(367.611568348902,-21.0592932850034,0.00244209184973706));
#39300=CARTESIAN_POINT('Ctrl Pts',(372.30982061585,-21.9062759889522,2.86513684838664));
#39301=CARTESIAN_POINT('Ctrl Pts',(372.382893739272,-21.9009851307799,2.82750527921983));
#39302=CARTESIAN_POINT('Ctrl Pts',(372.454498104907,-21.8956052014087,2.78709322077374));
#39303=CARTESIAN_POINT('Ctrl Pts',(372.643036039748,-21.8809245436686,2.67096329734966));
#39304=CARTESIAN_POINT('Ctrl Pts',(372.756730764924,-21.8715042487675,2.59033412028013));
#39305=CARTESIAN_POINT('Ctrl Pts',(372.992754913673,-21.8509453041641,2.39883245921991));
#39306=CARTESIAN_POINT('Ctrl Pts',(373.112529794808,-21.8398349848028,2.28539020326298));
#39307=CARTESIAN_POINT('Ctrl Pts',(373.241267734201,-21.8275119410745,2.14323148975206));
#39308=CARTESIAN_POINT('Ctrl Pts',(373.259168824634,-21.825789189413,2.12295709471688));
#39309=CARTESIAN_POINT('Ctrl Pts',(373.283557373645,-21.8234320747738,2.09462411971231));
#39310=CARTESIAN_POINT('Ctrl Pts',(373.290263880839,-21.8227828268609,2.08675670540548));
#39311=CARTESIAN_POINT('Ctrl Pts',(373.301711062041,-21.8216729911173,2.07319637109261));
#39312=CARTESIAN_POINT('Ctrl Pts',(373.306470127899,-21.821211090369,2.06751918333684));
#39313=CARTESIAN_POINT('Ctrl Pts',(373.316385616803,-21.8202477730655,2.05560760685672));
#39314=CARTESIAN_POINT('Ctrl Pts',(373.32153819584,-21.8197466524052,2.04937014357779));
#39315=CARTESIAN_POINT('Ctrl Pts',(373.334098144096,-21.8185236280619,2.03404853617821));
#39316=CARTESIAN_POINT('Ctrl Pts',(373.341479639451,-21.8178035696857,2.02494314431389));
#39317=CARTESIAN_POINT('Ctrl Pts',(373.36809420745,-21.8152018021794,1.99174429399388));
#39318=CARTESIAN_POINT('Ctrl Pts',(373.387031673304,-21.8133398976859,1.9674146125055));
#39319=CARTESIAN_POINT('Ctrl Pts',(373.433696964172,-21.8087140916263,1.9056535049467));
#39320=CARTESIAN_POINT('Ctrl Pts',(373.460968504656,-21.8059757569823,1.86788485355934));
#39321=CARTESIAN_POINT('Ctrl Pts',(373.674415499764,-21.7841374308493,1.55835553292629));
#39322=CARTESIAN_POINT('Ctrl Pts',(373.818745390186,-21.7665685501627,1.26010196384501));
#39323=CARTESIAN_POINT('Ctrl Pts',(373.935770583654,-21.743276557568,0.87860648371622));
#39324=CARTESIAN_POINT('Ctrl Pts',(373.954014280031,-21.7391577740338,0.81145027923866));
#39325=CARTESIAN_POINT('Ctrl Pts',(373.975514623449,-21.7335486833004,0.720803071599567));
#39326=CARTESIAN_POINT('Ctrl Pts',(373.980707263015,-21.7321203770548,0.697787828764224));
#39327=CARTESIAN_POINT('Ctrl Pts',(373.988803968052,-21.729765840041,0.659971473455969));
#39328=CARTESIAN_POINT('Ctrl Pts',(373.99185771668,-21.728844413903,0.645203063365475));
#39329=CARTESIAN_POINT('Ctrl Pts',(373.997580810329,-21.7270503467114,0.616511155613441));
#39330=CARTESIAN_POINT('Ctrl Pts',(374.000262160511,-21.7261781116167,0.602590386367526));
#39331=CARTESIAN_POINT('Ctrl Pts',(374.006329523518,-21.7241274254506,0.569931657583617));
#39332=CARTESIAN_POINT('Ctrl Pts',(374.009641460587,-21.7229466497956,0.551180636789482));
#39333=CARTESIAN_POINT('Ctrl Pts',(374.019939258384,-21.7190636850927,0.489702182951094));
#39334=CARTESIAN_POINT('Ctrl Pts',(374.026230077136,-21.7163397283381,0.446864663107874));
#39335=CARTESIAN_POINT('Ctrl Pts',(374.039106885686,-21.7098118446127,0.344933548992318));
#39336=CARTESIAN_POINT('Ctrl Pts',(374.044924051041,-21.7059854387018,0.285760423490181));
#39337=CARTESIAN_POINT('Ctrl Pts',(374.061138257654,-21.6909603051318,0.0555898186995252));
#39338=CARTESIAN_POINT('Ctrl Pts',(374.059531536481,-21.6794413151913,-0.11595420880175));
#39339=CARTESIAN_POINT('Ctrl Pts',(374.027741857847,-21.6552554987378,-0.472081490288715));
#39340=CARTESIAN_POINT('Ctrl Pts',(373.995122248821,-21.6426216504934,-0.655854882085085));
#39341=CARTESIAN_POINT('Ctrl Pts',(373.939868985894,-21.6289359167833,-0.861617495075068));
#39342=CARTESIAN_POINT('Ctrl Pts',(373.93261301436,-21.6272329183293,-0.887355479899007));
#39343=CARTESIAN_POINT('Ctrl Pts',(373.922120499917,-21.624897879142,-0.922875061892184));
#39344=CARTESIAN_POINT('Ctrl Pts',(373.919156382567,-21.6242513141715,-0.932735128224145));
#39345=CARTESIAN_POINT('Ctrl Pts',(373.913981590629,-21.6231448559065,-0.949654432522006));
#39346=CARTESIAN_POINT('Ctrl Pts',(373.911793792372,-21.6226836669908,-0.95672050426103));
#39347=CARTESIAN_POINT('Ctrl Pts',(373.907159147995,-21.6217204478724,-0.971508908189923));
#39348=CARTESIAN_POINT('Ctrl Pts',(373.904707487191,-21.6212187214428,-0.979229635483536));
#39349=CARTESIAN_POINT('Ctrl Pts',(373.898621306252,-21.6199919345615,-0.998148544096804));
#39350=CARTESIAN_POINT('Ctrl Pts',(373.894954439373,-21.6192687460855,-1.00933634920738));
#39351=CARTESIAN_POINT('Ctrl Pts',(373.881353361476,-21.6166426321991,-1.05007822699854));
#39352=CARTESIAN_POINT('Ctrl Pts',(373.871051368315,-21.6147600002147,-1.07950886690085));
#39353=CARTESIAN_POINT('Ctrl Pts',(373.844051325317,-21.6100718599456,-1.153195077101));
#39354=CARTESIAN_POINT('Ctrl Pts',(373.826802764311,-21.6072928093812,-1.19724223146323));
#39355=CARTESIAN_POINT('Ctrl Pts',(373.743840534152,-21.5947860480074,-1.39609232393525));
#39356=CARTESIAN_POINT('Ctrl Pts',(373.667038647829,-21.5854568700873,-1.54599383128619));
#39357=CARTESIAN_POINT('Ctrl Pts',(373.474834770935,-21.5649387033559,-1.85827679800381));
#39358=CARTESIAN_POINT('Ctrl Pts',(373.355403183912,-21.5537459110768,-2.01733453960356));
#39359=CARTESIAN_POINT('Ctrl Pts',(373.194022509707,-21.5394817795497,-2.1953724807785));
#39360=CARTESIAN_POINT('Ctrl Pts',(373.165337585478,-21.5369761814856,-2.22580618226301));
#39361=CARTESIAN_POINT('Ctrl Pts',(373.123066223026,-21.5333209376364,-2.26894107782471));
#39362=CARTESIAN_POINT('Ctrl Pts',(373.109948608228,-21.5321916293128,-2.28209714065851));
#39363=CARTESIAN_POINT('Ctrl Pts',(373.086637466069,-21.5301930227709,-2.30507576610511));
#39364=CARTESIAN_POINT('Ctrl Pts',(373.07649151796,-21.5293258519542,-2.314946041049));
#39365=CARTESIAN_POINT('Ctrl Pts',(373.05536479639,-21.527525521149,-2.33522954834881));
#39366=CARTESIAN_POINT('Ctrl Pts',(373.044375059447,-21.5265919654709,-2.34563289966435));
#39367=CARTESIAN_POINT('Ctrl Pts',(373.015889384619,-21.5241794408812,-2.37222074242629));
#39368=CARTESIAN_POINT('Ctrl Pts',(372.998286686673,-21.5226955807195,-2.38828901857445));
#39369=CARTESIAN_POINT('Ctrl Pts',(372.921664932002,-21.5162649514294,-2.45668913343389));
#39370=CARTESIAN_POINT('Ctrl Pts',(372.860917992413,-21.5112371224128,-2.50703599290373));
#39371=CARTESIAN_POINT('Ctrl Pts',(372.688807686359,-21.4971721451186,-2.63933487575649));
#39372=CARTESIAN_POINT('Ctrl Pts',(372.573931444021,-21.4879731843749,-2.71642388056084));
#39373=CARTESIAN_POINT('Ctrl Pts',(372.265505218993,-21.4639351193716,-2.89579112272621));
#39374=CARTESIAN_POINT('Ctrl Pts',(372.065839911069,-21.4489636306048,-2.98617912766259));
#39375=CARTESIAN_POINT('Ctrl Pts',(371.823438085971,-21.4324033428029,-3.06743059300092));
#39376=CARTESIAN_POINT('Ctrl Pts',(371.788119572725,-21.4300299111857,-3.07859575624792));
#39377=CARTESIAN_POINT('Ctrl Pts',(371.740151602604,-21.4268666415602,-3.09285496532919));
#39378=CARTESIAN_POINT('Ctrl Pts',(371.727665915429,-21.4260487326176,-3.09648443743946));
#39379=CARTESIAN_POINT('Ctrl Pts',(371.70791578232,-21.4247639375077,-3.10209621234038));
#39380=CARTESIAN_POINT('Ctrl Pts',(371.700665929133,-21.4242942225412,-3.10412874514725));
#39381=CARTESIAN_POINT('Ctrl Pts',(371.685700193208,-21.4233286217651,-3.10826794920499));
#39382=CARTESIAN_POINT('Ctrl Pts',(371.677983541762,-21.4228329515048,-3.11037131866956));
#39383=CARTESIAN_POINT('Ctrl Pts',(371.659416643566,-21.4216454903862,-3.11535801908702));
#39384=CARTESIAN_POINT('Ctrl Pts',(371.648558882816,-21.4209552947868,-3.11821345570626));
#39385=CARTESIAN_POINT('Ctrl Pts',(371.610921949337,-21.4185767153969,-3.12790144183443));
#39386=CARTESIAN_POINT('Ctrl Pts',(371.584069128766,-21.4169039483204,-3.13444644125051));
#39387=CARTESIAN_POINT('Ctrl Pts',(371.517929230512,-21.4128358232616,-3.14966847619807));
#39388=CARTESIAN_POINT('Ctrl Pts',(371.478556738527,-21.4104588124242,-3.15795702530659));
#39389=CARTESIAN_POINT('Ctrl Pts',(371.315701905379,-21.4007722869956,-3.18906785778866));
#39390=CARTESIAN_POINT('Ctrl Pts',(371.191085156325,-21.3936997307683,-3.20540264040855));
#39391=CARTESIAN_POINT('Ctrl Pts',(370.810274280389,-21.3723146336441,-3.23282918036115));
#39392=CARTESIAN_POINT('Ctrl Pts',(370.553470253751,-21.3581235225349,-3.22069446487603));
#39393=CARTESIAN_POINT('Ctrl Pts',(370.261634682643,-21.3405327747065,-3.17170779038807));
#39394=CARTESIAN_POINT('Ctrl Pts',(370.222575659103,-21.3381497694521,-3.16440635836082));
#39395=CARTESIAN_POINT('Ctrl Pts',(370.16583240598,-21.334641606644,-3.15270934337757));
#39396=CARTESIAN_POINT('Ctrl Pts',(370.148033716792,-21.3335345274922,-3.14888282728821));
#39397=CARTESIAN_POINT('Ctrl Pts',(370.116512346005,-21.3315616330043,-3.14182614687594));
#39398=CARTESIAN_POINT('Ctrl Pts',(370.102776540251,-21.3306977695544,-3.13865633366134));
#39399=CARTESIAN_POINT('Ctrl Pts',(370.074182053584,-21.3288905632669,-3.13185967997858));
#39400=CARTESIAN_POINT('Ctrl Pts',(370.059327540076,-21.3279467293159,-3.12821698266401));
#39401=CARTESIAN_POINT('Ctrl Pts',(370.020673401817,-21.3254773557378,-3.11844580493747));
#39402=CARTESIAN_POINT('Ctrl Pts',(369.996917305815,-21.323946476853,-3.11215067133646));
#39403=CARTESIAN_POINT('Ctrl Pts',(369.889954933388,-21.316992183378,-3.08249333949358));
#39404=CARTESIAN_POINT('Ctrl Pts',(369.807643391858,-21.3114703644308,-3.05606344806941));
#39405=CARTESIAN_POINT('Ctrl Pts',(369.575826971805,-21.2954197566551,-2.97120554285046));
#39406=CARTESIAN_POINT('Ctrl Pts',(369.429499346165,-21.284664937349,-2.90488153345523));
#39407=CARTESIAN_POINT('Ctrl Pts',(369.11149405211,-21.2601675761501,-2.73107902149694));
#39408=CARTESIAN_POINT('Ctrl Pts',(368.943740585815,-21.2464177428291,-2.61775577757414));
#39409=CARTESIAN_POINT('Ctrl Pts',(368.767527892904,-21.23177269076,-2.47288862052929));
#39410=CARTESIAN_POINT('Ctrl Pts',(368.74756646452,-21.2301109829521,-2.4560675096459));
#39411=CARTESIAN_POINT('Ctrl Pts',(368.720093728711,-21.2278228102019,-2.43234000342293));
#39412=CARTESIAN_POINT('Ctrl Pts',(368.712408119311,-21.2271825544836,-2.42563818996595));
#39413=CARTESIAN_POINT('Ctrl Pts',(368.69922169994,-21.226084022486,-2.41402906234032));
#39414=CARTESIAN_POINT('Ctrl Pts',(368.693705733471,-21.2256244910883,-2.40913919335098));
#39415=CARTESIAN_POINT('Ctrl Pts',(368.682144539781,-21.2246614106808,-2.39881921366845));
#39416=CARTESIAN_POINT('Ctrl Pts',(368.676102995784,-21.2241581842561,-2.39338509692603));
#39417=CARTESIAN_POINT('Ctrl Pts',(368.661773560249,-21.2229645668032,-2.38039799008005));
#39418=CARTESIAN_POINT('Ctrl Pts',(368.653504318056,-21.2222757065406,-2.37282439922897));
#39419=CARTESIAN_POINT('Ctrl Pts',(368.624143689053,-21.2198289604591,-2.3456505968525));
#39420=CARTESIAN_POINT('Ctrl Pts',(368.603274947239,-21.218088224308,-2.32581044810955));
#39421=CARTESIAN_POINT('Ctrl Pts',(368.551816569861,-21.2137831490516,-2.2755583292685));
#39422=CARTESIAN_POINT('Ctrl Pts',(368.52156562114,-21.211240699703,-2.2448062901687));
#39423=CARTESIAN_POINT('Ctrl Pts',(368.394585416592,-21.2004690777782,-2.11043009073927));
#39424=CARTESIAN_POINT('Ctrl Pts',(368.304126810216,-21.192534540594,-2.00108687043521));
#39425=CARTESIAN_POINT('Ctrl Pts',(368.084885354961,-21.171584562775,-1.6973371141667));
#39426=CARTESIAN_POINT('Ctrl Pts',(367.969490619708,-21.1585948572441,-1.49435027826096));
#39427=CARTESIAN_POINT('Ctrl Pts',(367.860599430131,-21.1423225627907,-1.24290540008052));
#39428=CARTESIAN_POINT('Ctrl Pts',(367.844953337446,-21.1398532728638,-1.2047882193159));
#39429=CARTESIAN_POINT('Ctrl Pts',(367.823358438197,-21.136241530456,-1.1491658145845));
#39430=CARTESIAN_POINT('Ctrl Pts',(367.816822325723,-21.135118732656,-1.13189195061084));
#39431=CARTESIAN_POINT('Ctrl Pts',(367.80554584632,-21.1331276924466,-1.10129812426441));
#39432=CARTESIAN_POINT('Ctrl Pts',(367.800743940264,-21.1322615258602,-1.08800125591406));
#39433=CARTESIAN_POINT('Ctrl Pts',(367.790968401941,-21.1304593578306,-1.06036411310029));
#39434=CARTESIAN_POINT('Ctrl Pts',(367.786008287192,-21.1295229335788,-1.04601946064155));
#39435=CARTESIAN_POINT('Ctrl Pts',(367.773453935209,-21.1270945200379,-1.0088645146689));
#39436=CARTESIAN_POINT('Ctrl Pts',(367.766013386807,-21.1255975157025,-0.986003643311825));
#39437=CARTESIAN_POINT('Ctrl Pts',(367.734650087054,-21.1190252202562,-0.885846593204056));
#39438=CARTESIAN_POINT('Ctrl Pts',(367.713389119955,-21.1138643575451,-0.807753937092196));
#39439=CARTESIAN_POINT('Ctrl Pts',(367.63939699187,-21.0926491166726,-0.48910608461047));
#39440=CARTESIAN_POINT('Ctrl Pts',(367.611382556567,-21.0758721219843,-0.243702563233693));
#39441=CARTESIAN_POINT('Ctrl Pts',(367.611568775535,-21.05929280343,0.00243818631688326));
#39442=CARTESIAN_POINT('Ctrl Pts',(367.611568778454,-21.0592925437503,0.00244204158639814));
#39443=CARTESIAN_POINT('Ctrl Pts',(367.611670430483,-21.050256619999,0.136591675607924));
#39444=CARTESIAN_POINT('Ctrl Pts',(367.62014819537,-21.0413230654388,0.270622973866999));
#39445=CARTESIAN_POINT('Ctrl Pts',(367.638663870236,-21.0319058275821,0.417250911136126));
#39446=CARTESIAN_POINT('Ctrl Pts',(367.640454036196,-21.0310429050257,0.430739636842257));
#39447=CARTESIAN_POINT('Ctrl Pts',(367.643579511215,-21.0296122624237,0.453198214792116));
#39448=CARTESIAN_POINT('Ctrl Pts',(367.644867327215,-21.0290421005523,0.462174356468439));
#39449=CARTESIAN_POINT('Ctrl Pts',(367.6472756725,-21.0280100508083,0.478471047067952));
#39450=CARTESIAN_POINT('Ctrl Pts',(367.648383576089,-21.0275474804427,0.485793360354128));
#39451=CARTESIAN_POINT('Ctrl Pts',(367.650717386335,-21.0265977187514,0.500866454061022));
#39452=CARTESIAN_POINT('Ctrl Pts',(367.65194634415,-21.0261107391561,0.508616473974502));
#39453=CARTESIAN_POINT('Ctrl Pts',(367.654828402712,-21.0249980982769,0.526371758319217));
#39454=CARTESIAN_POINT('Ctrl Pts',(367.656500428208,-21.024373509503,0.536373762997258));
#39455=CARTESIAN_POINT('Ctrl Pts',(367.661027934047,-21.0227353673763,0.562692666414876));
#39456=CARTESIAN_POINT('Ctrl Pts',(367.663962092744,-21.021726069586,0.578995963941172));
#39457=CARTESIAN_POINT('Ctrl Pts',(367.68778355975,-21.013916876501,0.705743217318074));
#39458=CARTESIAN_POINT('Ctrl Pts',(367.714312587374,-21.0074021149789,0.815060843580679));
#39459=CARTESIAN_POINT('Ctrl Pts',(367.782839169424,-20.9937891359949,1.04436530684944));
#39460=CARTESIAN_POINT('Ctrl Pts',(367.82632540199,-20.9867338571666,1.16370290727211));
#39461=CARTESIAN_POINT('Ctrl Pts',(367.929724673882,-20.9721630238219,1.40258692280196));
#39462=CARTESIAN_POINT('Ctrl Pts',(367.990259540533,-20.9646549665396,1.52159144867606));
#39463=CARTESIAN_POINT('Ctrl Pts',(368.102808468552,-20.9518257330537,1.71253146110584));
#39464=CARTESIAN_POINT('Ctrl Pts',(368.150728051799,-20.9466312456677,1.78668723258931));
#39465=CARTESIAN_POINT('Ctrl Pts',(368.215899938985,-20.939835450195,1.87899375779051));
#39466=CARTESIAN_POINT('Ctrl Pts',(368.230404543994,-20.9383386375002,1.89904326999987));
#39467=CARTESIAN_POINT('Ctrl Pts',(368.254267323612,-20.9359000297585,1.93124102367045));
#39468=CARTESIAN_POINT('Ctrl Pts',(368.263484005647,-20.9349637358191,1.94349323185903));
#39469=CARTESIAN_POINT('Ctrl Pts',(368.281335083599,-20.9331606726499,1.96687440764748));
#39470=CARTESIAN_POINT('Ctrl Pts',(368.289955721355,-20.9322944581095,1.97801347047114));
#39471=CARTESIAN_POINT('Ctrl Pts',(368.309836724503,-20.9303068393581,2.00335747225589));
#39472=CARTESIAN_POINT('Ctrl Pts',(368.321144391136,-20.9291835658514,2.01752453736189));
#39473=CARTESIAN_POINT('Ctrl Pts',(368.357345939766,-20.925609548994,2.06210384959962));
#39474=CARTESIAN_POINT('Ctrl Pts',(368.382676164423,-20.9231412833028,2.09215557668116));
#39475=CARTESIAN_POINT('Ctrl Pts',(368.58026508161,-20.9041225305542,2.31805794850113));
#39476=CARTESIAN_POINT('Ctrl Pts',(368.775150148223,-20.8865738677939,2.4927745435859));
#39477=CARTESIAN_POINT('Ctrl Pts',(369.089422744843,-20.8606466927883,2.71228561740984));
#39478=CARTESIAN_POINT('Ctrl Pts',(369.193876847071,-20.8523760208687,2.77670831094918));
#39479=CARTESIAN_POINT('Ctrl Pts',(369.336650652102,-20.8417200867529,2.85388931128534));
#39480=CARTESIAN_POINT('Ctrl Pts',(369.371894699906,-20.839139731914,2.87210899074695));
#39481=CARTESIAN_POINT('Ctrl Pts',(369.431832853633,-20.8348456873779,2.9017049800208));
#39482=CARTESIAN_POINT('Ctrl Pts',(369.456350127994,-20.8331152513396,2.91342771089651));
#39483=CARTESIAN_POINT('Ctrl Pts',(369.49062373296,-20.8307351075431,2.92928588543748));
#39484=CARTESIAN_POINT('Ctrl Pts',(369.500255817856,-20.8300704288418,2.93368508545387));
#39485=CARTESIAN_POINT('Ctrl Pts',(369.517288916468,-20.8289026962187,2.94136326596961));
#39486=CARTESIAN_POINT('Ctrl Pts',(369.52468090525,-20.8283984600167,2.94466197588536));
#39487=CARTESIAN_POINT('Ctrl Pts',(369.53885744033,-20.8274363726568,2.95092437904478));
#39488=CARTESIAN_POINT('Ctrl Pts',(369.545639852613,-20.8269782360171,2.95389258192722));
#39489=CARTESIAN_POINT('Ctrl Pts',(369.561901299952,-20.8258848123245,2.96094244905693));
#39490=CARTESIAN_POINT('Ctrl Pts',(369.571389899842,-20.8252508491641,2.96500203422523));
#39491=CARTESIAN_POINT('Ctrl Pts',(369.605693814825,-20.8229729183033,2.97948400672942));
#39492=CARTESIAN_POINT('Ctrl Pts',(369.630620727352,-20.8213440375405,2.98964133477149));
#39493=CARTESIAN_POINT('Ctrl Pts',(369.805844891081,-20.8100577578687,3.05849550205809));
#39494=CARTESIAN_POINT('Ctrl Pts',(369.960255472456,-20.8009436427681,3.10615176418349));
#39495=CARTESIAN_POINT('Ctrl Pts',(370.300729940333,-20.7813725874012,3.18381565404969));
#39496=CARTESIAN_POINT('Ctrl Pts',(370.487148977787,-20.7709650589865,3.20949655035878));
#39497=CARTESIAN_POINT('Ctrl Pts',(370.738651487676,-20.7564438916969,3.22196527997086));
#39498=CARTESIAN_POINT('Ctrl Pts',(370.802640332434,-20.752710726408,3.22322945611918));
#39499=CARTESIAN_POINT('Ctrl Pts',(370.912411778464,-20.7462110384625,3.22212908513293));
#39500=CARTESIAN_POINT('Ctrl Pts',(370.958185007214,-20.743472334966,3.22069419776701));
#39501=CARTESIAN_POINT('Ctrl Pts',(371.023351284055,-20.7395261251584,3.21726015717407));
#39502=CARTESIAN_POINT('Ctrl Pts',(371.042782067425,-20.738343500531,3.21605957696625));
#39503=CARTESIAN_POINT('Ctrl Pts',(371.076412864168,-20.7362857701199,3.21367555545438));
#39504=CARTESIAN_POINT('Ctrl Pts',(371.090618249888,-20.7354132456086,3.21257383828616));
#39505=CARTESIAN_POINT('Ctrl Pts',(371.119695797588,-20.7336201697358,3.2101246050641));
#39506=CARTESIAN_POINT('Ctrl Pts',(371.134566814587,-20.7326993486106,3.20876784769503));
#39507=CARTESIAN_POINT('Ctrl Pts',(371.172224359961,-20.7303577092353,3.20506808986542));
#39508=CARTESIAN_POINT('Ctrl Pts',(371.194996036016,-20.7289325389667,3.20258543569505));
#39509=CARTESIAN_POINT('Ctrl Pts',(371.281677495565,-20.7234715341142,3.19219889111599));
#39510=CARTESIAN_POINT('Ctrl Pts',(371.345368152211,-20.7193837624055,3.18262329706301));
#39511=CARTESIAN_POINT('Ctrl Pts',(371.722731983278,-20.6947005614426,3.11426923387221));
#39512=CARTESIAN_POINT('Ctrl Pts',(372.026377772473,-20.6726736702049,3.01110568884279));
#39513=CARTESIAN_POINT('Ctrl Pts',(372.309820629953,-20.6514935740584,2.86513684112378));
#39514=CARTESIAN_POINT('Ctrl Pts',(372.309820109182,-20.4075893673377,2.8651371093129));
#39515=CARTESIAN_POINT('Ctrl Pts',(372.236449403773,-20.4131724889653,2.90292191235081));
#39516=CARTESIAN_POINT('Ctrl Pts',(372.161612953962,-20.4187542681293,2.93789577972557));
#39517=CARTESIAN_POINT('Ctrl Pts',(372.020771392189,-20.4289722133308,2.99722782015865));
#39518=CARTESIAN_POINT('Ctrl Pts',(371.95519343297,-20.4336194577636,3.02236426609869));
#39519=CARTESIAN_POINT('Ctrl Pts',(371.849736759986,-20.4408671198182,3.05888127804711));
#39520=CARTESIAN_POINT('Ctrl Pts',(371.810371161769,-20.4435237400848,3.07166901593224));
#39521=CARTESIAN_POINT('Ctrl Pts',(371.758224777912,-20.4469691961886,3.08750472081901));
#39522=CARTESIAN_POINT('Ctrl Pts',(371.745658090238,-20.4477939288932,3.09123735626392));
#39523=CARTESIAN_POINT('Ctrl Pts',(371.72501383467,-20.4491392410567,3.09723240715502));
#39524=CARTESIAN_POINT('Ctrl Pts',(371.716949732103,-20.4496623725934,3.09954010870645));
#39525=CARTESIAN_POINT('Ctrl Pts',(371.701145527495,-20.4506828424217,3.10399611253002));
#39526=CARTESIAN_POINT('Ctrl Pts',(371.69340627628,-20.4511803197094,3.1061469969777));
#39527=CARTESIAN_POINT('Ctrl Pts',(371.676086654923,-20.4522887753341,3.11089076482974));
#39528=CARTESIAN_POINT('Ctrl Pts',(371.666502104897,-20.4528988818066,3.11346839449123));
#39529=CARTESIAN_POINT('Ctrl Pts',(371.633241857372,-20.455005117194,3.12224870853292));
#39530=CARTESIAN_POINT('Ctrl Pts',(371.609506856374,-20.4564889669916,3.12822611930707));
#39531=CARTESIAN_POINT('Ctrl Pts',(371.364224522508,-20.4716478690781,3.18703467440204));
#39532=CARTESIAN_POINT('Ctrl Pts',(371.137705945806,-20.4842078716369,3.21651620159829));
#39533=CARTESIAN_POINT('Ctrl Pts',(370.766279165288,-20.505002342164,3.22523484205441));
#39534=CARTESIAN_POINT('Ctrl Pts',(370.622555644941,-20.5130913865835,3.21899386683575));
#39535=CARTESIAN_POINT('Ctrl Pts',(370.399384112381,-20.5261329373996,3.19428957090933));
#39536=CARTESIAN_POINT('Ctrl Pts',(370.319400195146,-20.5309030228467,3.18237512441352));
#39537=CARTESIAN_POINT('Ctrl Pts',(370.216320540462,-20.5372148381288,3.16303257245616));
#39538=CARTESIAN_POINT('Ctrl Pts',(370.19273871102,-20.5386700068387,3.15833372039807));
#39539=CARTESIAN_POINT('Ctrl Pts',(370.154352735759,-20.5410579356198,3.15023739207248));
#39540=CARTESIAN_POINT('Ctrl Pts',(370.139515867155,-20.5419856254667,3.14699831190856));
#39541=CARTESIAN_POINT('Ctrl Pts',(370.110900722152,-20.543784168412,3.14053903276191));
#39542=CARTESIAN_POINT('Ctrl Pts',(370.097119647786,-20.5446545576779,3.13733271388021));
#39543=CARTESIAN_POINT('Ctrl Pts',(370.065378860911,-20.5466691750322,3.12972719018952));
#39544=CARTESIAN_POINT('Ctrl Pts',(370.047435137408,-20.5478154393323,3.12526399326896));
#39545=CARTESIAN_POINT('Ctrl Pts',(369.989563077295,-20.5515367178166,3.1103393089887));
#39546=CARTESIAN_POINT('Ctrl Pts',(369.949798330844,-20.5541313479689,3.09926543057856));
#39547=CARTESIAN_POINT('Ctrl Pts',(369.688723175139,-20.5714236508928,3.02112639715902));
#39548=CARTESIAN_POINT('Ctrl Pts',(369.475005077592,-20.5868816049001,2.93118153154803));
#39549=CARTESIAN_POINT('Ctrl Pts',(369.165913419395,-20.6107811429149,2.75997644837197));
#39550=CARTESIAN_POINT('Ctrl Pts',(369.062490420558,-20.6190603475817,2.69474914675987));
#39551=CARTESIAN_POINT('Ctrl Pts',(368.895026045517,-20.632716565347,2.57531341287178));
#39552=CARTESIAN_POINT('Ctrl Pts',(368.828938371322,-20.6381766613465,2.52419246057124));
#39553=CARTESIAN_POINT('Ctrl Pts',(368.75235390224,-20.6445212095048,2.46004304285685));
#39554=CARTESIAN_POINT('Ctrl Pts',(368.73988171435,-20.6455549995162,2.44943319002243));
#39555=CARTESIAN_POINT('Ctrl Pts',(368.720599432734,-20.6471533825058,2.43277515035024));
#39556=CARTESIAN_POINT('Ctrl Pts',(368.713733399541,-20.647722558541,2.42679254838276));
#39557=CARTESIAN_POINT('Ctrl Pts',(368.700988921186,-20.6487789336027,2.41559247476848));
#39558=CARTESIAN_POINT('Ctrl Pts',(368.695104239349,-20.6492666462905,2.41038263607563));
#39559=CARTESIAN_POINT('Ctrl Pts',(368.681611122912,-20.6503848706486,2.3983485459287));
#39560=CARTESIAN_POINT('Ctrl Pts',(368.674016046234,-20.6510142731382,2.39150959100153));
#39561=CARTESIAN_POINT('Ctrl Pts',(368.654007394432,-20.6526727140554,2.37331978349067));
#39562=CARTESIAN_POINT('Ctrl Pts',(368.641649748008,-20.653697329528,2.36190751285045));
#39563=CARTESIAN_POINT('Ctrl Pts',(368.534295856988,-20.6626073761054,2.26119759097805));
#39564=CARTESIAN_POINT('Ctrl Pts',(368.444698779682,-20.6701077911428,2.16629740969664));
#39565=CARTESIAN_POINT('Ctrl Pts',(368.24170244363,-20.6880123158001,1.92331429889627));
#39566=CARTESIAN_POINT('Ctrl Pts',(368.134925767335,-20.6982667568535,1.77033230655128));
#39567=CARTESIAN_POINT('Ctrl Pts',(367.996436053644,-20.7140239887933,1.52998602980585));
#39568=CARTESIAN_POINT('Ctrl Pts',(367.954292124961,-20.7192692009857,1.4490964019836));
#39569=CARTESIAN_POINT('Ctrl Pts',(367.890408320602,-20.7281170015069,1.31265146894373));
#39570=CARTESIAN_POINT('Ctrl Pts',(367.866679033928,-20.7316550586823,1.25808441033854));
#39571=CARTESIAN_POINT('Ctrl Pts',(367.836433102605,-20.7365440122689,1.18290690545401));
#39572=CARTESIAN_POINT('Ctrl Pts',(367.828592408877,-20.7378503711747,1.16283973251491));
#39573=CARTESIAN_POINT('Ctrl Pts',(367.815757742447,-20.7400566375981,1.1289938711139));
#39574=CARTESIAN_POINT('Ctrl Pts',(367.810655419908,-20.7409528976578,1.11525682315256));
#39575=CARTESIAN_POINT('Ctrl Pts',(367.8007642724,-20.7427291241415,1.08805989106883));
#39576=CARTESIAN_POINT('Ctrl Pts',(367.795970906776,-20.7436089150044,1.07460200857527));
#39577=CARTESIAN_POINT('Ctrl Pts',(367.784544510618,-20.7457534041116,1.04183348526444));
#39578=CARTESIAN_POINT('Ctrl Pts',(367.778005279433,-20.7470211690814,1.02249101355206));
#39579=CARTESIAN_POINT('Ctrl Pts',(367.759958909582,-20.7506386124121,0.967391135818501));
#39580=CARTESIAN_POINT('Ctrl Pts',(367.748892823107,-20.7530025609021,0.93149380908082));
#39581=CARTESIAN_POINT('Ctrl Pts',(367.678401948528,-20.7691059141394,0.687773792393171));
#39582=CARTESIAN_POINT('Ctrl Pts',(367.639398211184,-20.7835044470568,0.474654693217188));
#39583=CARTESIAN_POINT('Ctrl Pts',(367.614988883063,-20.8040106317177,0.172232679670542));
#39584=CARTESIAN_POINT('Ctrl Pts',(367.611504123752,-20.8099302381019,0.0849412129632191));
#39585=CARTESIAN_POINT('Ctrl Pts',(367.611664143858,-20.8244823436421,-0.131334013137009));
#39586=CARTESIAN_POINT('Ctrl Pts',(367.619498885925,-20.8330526939712,-0.260176677917461));
#39587=CARTESIAN_POINT('Ctrl Pts',(367.637059308486,-20.8423358011356,-0.404892037900025));
#39588=CARTESIAN_POINT('Ctrl Pts',(367.639213326537,-20.8433993001567,-0.421552909710437));
#39589=CARTESIAN_POINT('Ctrl Pts',(367.642871577308,-20.845091512285,-0.448207926447213));
#39590=CARTESIAN_POINT('Ctrl Pts',(367.644292679191,-20.8457245970961,-0.458212912194987));
#39591=CARTESIAN_POINT('Ctrl Pts',(367.646903514384,-20.8468457447733,-0.475992915680618));
#39592=CARTESIAN_POINT('Ctrl Pts',(367.648074678532,-20.8473348264556,-0.483770461822187));
#39593=CARTESIAN_POINT('Ctrl Pts',(367.650657789762,-20.8483844177657,-0.50050817679968));
#39594=CARTESIAN_POINT('Ctrl Pts',(367.652079094575,-20.8489443980657,-0.509466703914104));
#39595=CARTESIAN_POINT('Ctrl Pts',(367.656145279662,-20.8504991640164,-0.534414926739518));
#39596=CARTESIAN_POINT('Ctrl Pts',(367.658873021496,-20.8514894075788,-0.550391103699132));
#39597=CARTESIAN_POINT('Ctrl Pts',(367.675838695875,-20.8573517055304,-0.645430537034827));
#39598=CARTESIAN_POINT('Ctrl Pts',(367.692909538148,-20.8620785845905,-0.723966327732457));
#39599=CARTESIAN_POINT('Ctrl Pts',(367.753466689018,-20.8761320040982,-0.959719535726872));
#39600=CARTESIAN_POINT('Ctrl Pts',(367.805963794626,-20.8851725494863,-1.11435345873297));
#39601=CARTESIAN_POINT('Ctrl Pts',(367.952696805268,-20.9061091157299,-1.45837945728222));
#39602=CARTESIAN_POINT('Ctrl Pts',(368.054286687824,-20.9180379973265,-1.64378262616659));
#39603=CARTESIAN_POINT('Ctrl Pts',(368.188723632344,-20.9323017221405,-1.8405708770611));
#39604=CARTESIAN_POINT('Ctrl Pts',(368.204484444029,-20.9339536948737,-1.86302069367058));
#39605=CARTESIAN_POINT('Ctrl Pts',(368.230783847336,-20.9366791972889,-1.89948295937156));
#39606=CARTESIAN_POINT('Ctrl Pts',(368.241153813833,-20.9377462646679,-1.91361570820506));
#39607=CARTESIAN_POINT('Ctrl Pts',(368.260005433912,-20.9396729243354,-1.93887307593593));
#39608=CARTESIAN_POINT('Ctrl Pts',(368.268445256511,-20.9405308713393,-1.95002847274029));
#39609=CARTESIAN_POINT('Ctrl Pts',(368.286602922103,-20.9423671144386,-1.97370652275852));
#39610=CARTESIAN_POINT('Ctrl Pts',(368.296341035147,-20.9433461975165,-1.98621309652278));
#39611=CARTESIAN_POINT('Ctrl Pts',(368.322968211011,-20.9460083081062,-2.01989458665303));
#39612=CARTESIAN_POINT('Ctrl Pts',(368.340032306862,-20.947698296167,-2.04092888359619));
#39613=CARTESIAN_POINT('Ctrl Pts',(368.43350445921,-20.9568726538298,-2.15322533921771));
#39614=CARTESIAN_POINT('Ctrl Pts',(368.514650339832,-20.9645499580092,-2.24040648040338));
#39615=CARTESIAN_POINT('Ctrl Pts',(368.712941883156,-20.9826774605727,-2.43110076573428));
#39616=CARTESIAN_POINT('Ctrl Pts',(368.833166472407,-20.993228157677,-2.53098266361671));
#39617=CARTESIAN_POINT('Ctrl Pts',(369.09656126622,-21.0151303726708,-2.71927181700343));
#39618=CARTESIAN_POINT('Ctrl Pts',(369.240395242531,-21.0264499172951,-2.80600401173764));
#39619=CARTESIAN_POINT('Ctrl Pts',(369.414427222154,-21.0389568559812,-2.89322556837779));
#39620=CARTESIAN_POINT('Ctrl Pts',(369.438667530525,-21.0406731912015,-2.90499636499687));
#39621=CARTESIAN_POINT('Ctrl Pts',(369.472401161234,-21.0430234700713,-2.92085726829929));
#39622=CARTESIAN_POINT('Ctrl Pts',(369.481770031706,-21.0436721777599,-2.92520745504079));
#39623=CARTESIAN_POINT('Ctrl Pts',(369.497894864518,-21.0447815501,-2.93260056167912));
#39624=CARTESIAN_POINT('Ctrl Pts',(369.504640634475,-21.0452435229423,-2.93566533441154));
#39625=CARTESIAN_POINT('Ctrl Pts',(369.518783580922,-21.0462075354752,-2.94203207999242));
#39626=CARTESIAN_POINT('Ctrl Pts',(369.52618271919,-21.0467092756968,-2.94532946445713));
#39627=CARTESIAN_POINT('Ctrl Pts',(369.544345745921,-21.0479347398582,-2.95334177052092));
#39628=CARTESIAN_POINT('Ctrl Pts',(369.555123274173,-21.0486566049195,-2.95802584335908));
#39629=CARTESIAN_POINT('Ctrl Pts',(369.594419237341,-21.0512702223882,-2.97484951436676));
#39630=CARTESIAN_POINT('Ctrl Pts',(369.623087795619,-21.0531419427455,-2.98663692464109));
#39631=CARTESIAN_POINT('Ctrl Pts',(369.695560182531,-21.0577966901896,-3.01521954617209));
#39632=CARTESIAN_POINT('Ctrl Pts',(369.73956997722,-21.0605537496065,-3.03147579037329));
#39633=CARTESIAN_POINT('Ctrl Pts',(370.103192032219,-21.0828871011326,-3.15683737291466));
#39634=CARTESIAN_POINT('Ctrl Pts',(370.437785774692,-21.1008706321102,-3.21604877209414));
#39635=CARTESIAN_POINT('Ctrl Pts',(370.838172825026,-21.1243314065514,-3.22335721264079));
#39636=CARTESIAN_POINT('Ctrl Pts',(370.900860905433,-21.1280517794558,-3.22267246688889));
#39637=CARTESIAN_POINT('Ctrl Pts',(370.986145765926,-21.1331953627915,-3.21925148555618));
#39638=CARTESIAN_POINT('Ctrl Pts',(371.008794598007,-21.1345691886592,-3.21810342710667));
#39639=CARTESIAN_POINT('Ctrl Pts',(371.044806860208,-21.1367668704605,-3.21589669917595));
#39640=CARTESIAN_POINT('Ctrl Pts',(371.058179321594,-21.1375858492668,-3.21499350486038));
#39641=CARTESIAN_POINT('Ctrl Pts',(371.085625750943,-21.1392729229095,-3.21296766769742));
#39642=CARTESIAN_POINT('Ctrl Pts',(371.099698735474,-21.1401412861844,-3.2118359034023));
#39643=CARTESIAN_POINT('Ctrl Pts',(371.132301692281,-21.1421609413787,-3.20899820138306));
#39644=CARTESIAN_POINT('Ctrl Pts',(371.150825088617,-21.1433143454845,-3.20722418478793));
#39645=CARTESIAN_POINT('Ctrl Pts',(371.209920565754,-21.14701355302,-3.20104758036026));
#39646=CARTESIAN_POINT('Ctrl Pts',(371.250423528438,-21.1495783583976,-3.1960348607383));
#39647=CARTESIAN_POINT('Ctrl Pts',(371.3453049054,-21.1556583981561,-3.18245805948559));
#39648=CARTESIAN_POINT('Ctrl Pts',(371.399579405198,-21.1591921892299,-3.17326738077384));
#39649=CARTESIAN_POINT('Ctrl Pts',(371.600641249979,-21.1724921674109,-3.13389841893385));
#39650=CARTESIAN_POINT('Ctrl Pts',(371.745490944,-21.182503129386,-3.0948870706698));
#39651=CARTESIAN_POINT('Ctrl Pts',(372.093012864535,-21.2073269502911,-2.97477314321546));
#39652=CARTESIAN_POINT('Ctrl Pts',(372.291202952998,-21.2222128514161,-2.88289574145071));
#39653=CARTESIAN_POINT('Ctrl Pts',(372.500376836419,-21.2378154055712,-2.75880504297725));
#39654=CARTESIAN_POINT('Ctrl Pts',(372.52198652861,-21.2394253638472,-2.7456387844639));
#39655=CARTESIAN_POINT('Ctrl Pts',(372.551974207059,-21.2416543578093,-2.726880186768));
#39656=CARTESIAN_POINT('Ctrl Pts',(372.560483819027,-21.2422862934715,-2.72150141791122));
#39657=CARTESIAN_POINT('Ctrl Pts',(372.575155610684,-21.2433746324087,-2.71213114799151));
#39658=CARTESIAN_POINT('Ctrl Pts',(372.581329554162,-21.243832236518,-2.70815833751388));
#39659=CARTESIAN_POINT('Ctrl Pts',(372.59434570188,-21.2447960942692,-2.69971966909606));
#39660=CARTESIAN_POINT('Ctrl Pts',(372.601184598619,-21.2453019977332,-2.69524882456415));
#39661=CARTESIAN_POINT('Ctrl Pts',(372.618107410608,-21.2465527447182,-2.68409365324746));
#39662=CARTESIAN_POINT('Ctrl Pts',(372.628170948985,-21.2472955487117,-2.67737838305814));
#39663=CARTESIAN_POINT('Ctrl Pts',(372.665882107389,-21.2500763154891,-2.65190613231603));
#39664=CARTESIAN_POINT('Ctrl Pts',(372.693276374765,-21.2520907419033,-2.63277556327152));
#39665=CARTESIAN_POINT('Ctrl Pts',(372.899156264197,-21.2672277725459,-2.48418499539591));
#39666=CARTESIAN_POINT('Ctrl Pts',(373.064252047781,-21.2793820431779,-2.33712451788103));
#39667=CARTESIAN_POINT('Ctrl Pts',(373.353765251096,-21.3034079003868,-2.02039636753664));
#39668=CARTESIAN_POINT('Ctrl Pts',(373.47918593318,-21.3152118239945,-1.85317939726525));
#39669=CARTESIAN_POINT('Ctrl Pts',(373.601825034779,-21.3293337978134,-1.65159739813631));
#39670=CARTESIAN_POINT('Ctrl Pts',(373.615781711854,-21.3309858033637,-1.62798301549597));
#39671=CARTESIAN_POINT('Ctrl Pts',(373.63816052682,-21.3337113489871,-1.5889905916598));
#39672=CARTESIAN_POINT('Ctrl Pts',(373.64676179006,-21.3347784264039,-1.57371659517667));
#39673=CARTESIAN_POINT('Ctrl Pts',(373.662002024521,-21.3367050970169,-1.5461291875673));
#39674=CARTESIAN_POINT('Ctrl Pts',(373.6686862832,-21.337563044849,-1.5338412012516));
#39675=CARTESIAN_POINT('Ctrl Pts',(373.682773574452,-21.3393992819088,-1.50753733253041));
#39676=CARTESIAN_POINT('Ctrl Pts',(373.690153602984,-21.3403783580614,-1.49350961189458));
#39677=CARTESIAN_POINT('Ctrl Pts',(373.709863151346,-21.3430404300869,-1.45536606315369));
#39678=CARTESIAN_POINT('Ctrl Pts',(373.721992411232,-21.3447303861658,-1.43114873944816));
#39679=CARTESIAN_POINT('Ctrl Pts',(373.785767105788,-21.3539041972888,-1.2997036919467));
#39680=CARTESIAN_POINT('Ctrl Pts',(373.831742132378,-21.3615809592628,-1.18984214288387));
#39681=CARTESIAN_POINT('Ctrl Pts',(373.923728905526,-21.3797064154961,-0.930601627656953));
#39682=CARTESIAN_POINT('Ctrl Pts',(373.965165288329,-21.3902555595844,-0.779915080146005));
#39683=CARTESIAN_POINT('Ctrl Pts',(374.028141953759,-21.4121584291594,-0.462315219347082));
#39684=CARTESIAN_POINT('Ctrl Pts',(374.047874504023,-21.4234801947338,-0.295486099095809));
#39685=CARTESIAN_POINT('Ctrl Pts',(374.055599306909,-21.4359891401719,-0.100942438561298));
#39686=CARTESIAN_POINT('Ctrl Pts',(374.056330712701,-21.4377054586117,-0.0740055626245434));
#39687=CARTESIAN_POINT('Ctrl Pts',(374.056875053357,-21.4400557187606,-0.0367334839249444));
#39688=CARTESIAN_POINT('Ctrl Pts',(374.056976238577,-21.4407044241994,-0.0264044523672441));
#39689=CARTESIAN_POINT('Ctrl Pts',(374.057064719241,-21.4418137937143,-0.00866582622766637));
#39690=CARTESIAN_POINT('Ctrl Pts',(374.057076125694,-21.4422757659688,-0.00125650916390129));
#39691=CARTESIAN_POINT('Ctrl Pts',(374.057046514133,-21.4432397784107,0.0142534064147461));
#39692=CARTESIAN_POINT('Ctrl Pts',(374.057000506907,-21.4437415191223,0.0223539007758042));
#39693=CARTESIAN_POINT('Ctrl Pts',(374.056812912081,-21.4449669864023,0.042204831239696));
#39694=CARTESIAN_POINT('Ctrl Pts',(374.05663759566,-21.4456888540699,0.0539549773240474));
#39695=CARTESIAN_POINT('Ctrl Pts',(374.055766103616,-21.4483024919377,0.0966922906082021));
#39696=CARTESIAN_POINT('Ctrl Pts',(374.054687163395,-21.4501742296776,0.127671047637771));
#39697=CARTESIAN_POINT('Ctrl Pts',(374.050852459734,-21.4548290294194,0.205482665572566));
#39698=CARTESIAN_POINT('Ctrl Pts',(374.047520731281,-21.4575861230028,0.252280995407905));
#39699=CARTESIAN_POINT('Ctrl Pts',(374.011835407342,-21.4799204293363,0.635263878207513));
#39700=CARTESIAN_POINT('Ctrl Pts',(373.927843709714,-21.4979047608619,0.964528905658023));
#39701=CARTESIAN_POINT('Ctrl Pts',(373.769441908256,-21.5213658788122,1.33232568326378));
#39702=CARTESIAN_POINT('Ctrl Pts',(373.742980822224,-21.5250854957027,1.38914502608119));
#39703=CARTESIAN_POINT('Ctrl Pts',(373.704713072962,-21.5302281916624,1.46542247897418));
#39704=CARTESIAN_POINT('Ctrl Pts',(373.694331252966,-21.5316019086747,1.48558240174572));
#39705=CARTESIAN_POINT('Ctrl Pts',(373.677476210964,-21.5337994598229,1.51748072318112));
#39706=CARTESIAN_POINT('Ctrl Pts',(373.671140885479,-21.5346184178957,1.52929142662923));
#39707=CARTESIAN_POINT('Ctrl Pts',(373.657980876679,-21.5363054812106,1.553461949206));
#39708=CARTESIAN_POINT('Ctrl Pts',(373.651148282713,-21.5371738550963,1.56581710907888));
#39709=CARTESIAN_POINT('Ctrl Pts',(373.635122181286,-21.539193590141,1.59435221385653));
#39710=CARTESIAN_POINT('Ctrl Pts',(373.625869344799,-21.5403470640137,1.61049809454227));
#39711=CARTESIAN_POINT('Ctrl Pts',(373.595877003629,-21.5440467250904,1.66179859367238));
#39712=CARTESIAN_POINT('Ctrl Pts',(373.574609932803,-21.5466119208011,1.6966386121425));
#39713=CARTESIAN_POINT('Ctrl Pts',(373.523117347707,-21.5526930479246,1.77749979454535));
#39714=CARTESIAN_POINT('Ctrl Pts',(373.492363533691,-21.5562275450168,1.82316779960588));
#39715=CARTESIAN_POINT('Ctrl Pts',(373.373573195683,-21.5695314832925,1.99016777537936));
#39716=CARTESIAN_POINT('Ctrl Pts',(373.27828293745,-21.5795458593314,2.10608918660309));
#39717=CARTESIAN_POINT('Ctrl Pts',(373.025590365263,-21.6043680783881,2.37315832507954));
#39718=CARTESIAN_POINT('Ctrl Pts',(372.860235300926,-21.6192485973552,2.51579566290711));
#39719=CARTESIAN_POINT('Ctrl Pts',(372.661009056787,-21.6348466845178,2.6551755634908));
#39720=CARTESIAN_POINT('Ctrl Pts',(372.640101685127,-21.6364569312988,2.66943868081069));
#39721=CARTESIAN_POINT('Ctrl Pts',(372.610644886824,-21.6386862569657,2.68902978557585));
#39722=CARTESIAN_POINT('Ctrl Pts',(372.602235833935,-21.639318240708,2.69456581619799));
#39723=CARTESIAN_POINT('Ctrl Pts',(372.587649792265,-21.640406639658,2.70407074168204));
#39724=CARTESIAN_POINT('Ctrl Pts',(372.581484985815,-21.6408642560052,2.70805806396937));
#39725=CARTESIAN_POINT('Ctrl Pts',(372.568431032926,-21.6418281126203,2.71643807146547));
#39726=CARTESIAN_POINT('Ctrl Pts',(372.56153870847,-21.6423340028603,2.72082569009355));
#39727=CARTESIAN_POINT('Ctrl Pts',(372.544400418106,-21.6435846714673,2.73164447171057));
#39728=CARTESIAN_POINT('Ctrl Pts',(372.53413466586,-21.6443274108694,2.73804432265444));
#39729=CARTESIAN_POINT('Ctrl Pts',(372.495389120594,-21.6471076486376,2.76189708060224));
#39730=CARTESIAN_POINT('Ctrl Pts',(372.466673517353,-21.6491216221936,2.77896535142017));
#39731=CARTESIAN_POINT('Ctrl Pts',(372.39558244711,-21.6540075646915,2.81973889580822));
#39732=CARTESIAN_POINT('Ctrl Pts',(372.35294581336,-21.6568525731455,2.84292801726746));
#39733=CARTESIAN_POINT('Ctrl Pts',(372.309820475366,-21.6596622257337,2.86513692073371));
#39734=CARTESIAN_POINT('Origin',(370.834317853224,2.31077344927308,0.));
#39735=CARTESIAN_POINT('',(372.309820652883,-23.1546465340815,2.86513682931516));
#39736=CARTESIAN_POINT('',(372.309820613641,-22.9071794904733,2.86513684952399));
#39737=CARTESIAN_POINT('',(372.309820613641,2.31077344927308,2.86513684952399));
#39738=CARTESIAN_POINT('Ctrl Pts',(372.309820652881,-23.1546465340816,2.86513682931627));
#39739=CARTESIAN_POINT('Ctrl Pts',(372.375818427643,-23.1504575899474,2.83114895814868));
#39740=CARTESIAN_POINT('Ctrl Pts',(372.440695164174,-23.1462298331336,2.79485332831167));
#39741=CARTESIAN_POINT('Ctrl Pts',(372.557946972649,-23.1383172123807,2.72381177552407));
#39742=CARTESIAN_POINT('Ctrl Pts',(372.610603706517,-23.1346570443842,2.6897687278091));
#39743=CARTESIAN_POINT('Ctrl Pts',(372.699363577078,-23.1282731428272,2.62864122470886));
#39744=CARTESIAN_POINT('Ctrl Pts',(372.735952986043,-23.1255758729175,2.60229394204416));
#39745=CARTESIAN_POINT('Ctrl Pts',(372.787437630317,-23.1216790267826,2.56355516601944));
#39746=CARTESIAN_POINT('Ctrl Pts',(372.802793534755,-23.1205034687938,2.55178279225814));
#39747=CARTESIAN_POINT('Ctrl Pts',(372.82925555013,-23.1184540105637,2.53111508787315));
#39748=CARTESIAN_POINT('Ctrl Pts',(372.84041058973,-23.1175826328585,2.52228307786803));
#39749=CARTESIAN_POINT('Ctrl Pts',(372.86318364494,-23.1157881871445,2.50400585935424));
#39750=CARTESIAN_POINT('Ctrl Pts',(372.8747950368,-23.1148648237785,2.49455298514946));
#39751=CARTESIAN_POINT('Ctrl Pts',(372.904144886064,-23.1125090853678,2.47031714470044));
#39752=CARTESIAN_POINT('Ctrl Pts',(372.921790878424,-23.1110722532151,2.45542400936769));
#39753=CARTESIAN_POINT('Ctrl Pts',(372.989068402243,-23.1055135279536,2.39739269569842));
#39754=CARTESIAN_POINT('Ctrl Pts',(373.0375324728,-23.1013372878133,2.35293136202504));
#39755=CARTESIAN_POINT('Ctrl Pts',(373.323772203477,-23.0755829695132,2.07373143717664));
#39756=CARTESIAN_POINT('Ctrl Pts',(373.525152884969,-23.052413081836,1.80473668543287));
#39757=CARTESIAN_POINT('Ctrl Pts',(373.703512244996,-23.0272813886519,1.46834187313638));
#39758=CARTESIAN_POINT('Ctrl Pts',(373.724516971627,-23.0242251842694,1.42655312337029));
#39759=CARTESIAN_POINT('Ctrl Pts',(373.757886841314,-23.019219553762,1.3563988761391));
#39760=CARTESIAN_POINT('Ctrl Pts',(373.770766007287,-23.017246292843,1.32828684473065));
#39761=CARTESIAN_POINT('Ctrl Pts',(373.787972682978,-23.0145555127484,1.28925498367497));
#39762=CARTESIAN_POINT('Ctrl Pts',(373.792647639179,-23.0138185706774,1.27849135851359));
#39763=CARTESIAN_POINT('Ctrl Pts',(373.800447197861,-23.0125793267435,1.26026178548212));
#39764=CARTESIAN_POINT('Ctrl Pts',(373.803602632893,-23.0120751922324,1.25280922704203));
#39765=CARTESIAN_POINT('Ctrl Pts',(373.809591347453,-23.0111131293128,1.23851525048463));
#39766=CARTESIAN_POINT('Ctrl Pts',(373.812429157636,-23.0106549165748,1.23167587143866));
#39767=CARTESIAN_POINT('Ctrl Pts',(373.819167917302,-23.0095610636028,1.21527539534458));
#39768=CARTESIAN_POINT('Ctrl Pts',(373.823046564516,-23.0089267498693,1.2057051416493));
#39769=CARTESIAN_POINT('Ctrl Pts',(373.836885267025,-23.0066457452285,1.17108211402457));
#39770=CARTESIAN_POINT('Ctrl Pts',(373.846577172637,-23.0050141972727,1.14592246363119));
#39771=CARTESIAN_POINT('Ctrl Pts',(373.915157645971,-22.9931914684596,0.961006218298169));
#39772=CARTESIAN_POINT('Ctrl Pts',(373.961626460669,-22.9836065499557,0.79690769540356));
#39773=CARTESIAN_POINT('Ctrl Pts',(374.025069682204,-22.9654332471019,0.478568227592113));
#39774=CARTESIAN_POINT('Ctrl Pts',(374.04432023341,-22.9568573415195,0.325280366040332));
#39775=CARTESIAN_POINT('Ctrl Pts',(374.058803532347,-22.9412698440434,0.0530398975333145));
#39776=CARTESIAN_POINT('Ctrl Pts',(374.058576340274,-22.9343739858897,-0.0653747579176822));
#39777=CARTESIAN_POINT('Ctrl Pts',(374.050300461851,-22.9256503207824,-0.210485047580604));
#39778=CARTESIAN_POINT('Ctrl Pts',(374.048422121928,-22.9240179561323,-0.237448471477331));
#39779=CARTESIAN_POINT('Ctrl Pts',(374.044906226568,-22.9214127076359,-0.280161489643905));
#39780=CARTESIAN_POINT('Ctrl Pts',(374.043491340748,-22.920446811544,-0.295928498657462));
#39781=CARTESIAN_POINT('Ctrl Pts',(374.040608501147,-22.9186211403665,-0.325596727179447));
#39782=CARTESIAN_POINT('Ctrl Pts',(374.039166151481,-22.9177621900321,-0.339500107667311));
#39783=CARTESIAN_POINT('Ctrl Pts',(374.03571157404,-22.9158197903486,-0.370813931734146));
#39784=CARTESIAN_POINT('Ctrl Pts',(374.033647689189,-22.9147347381789,-0.38821812028866));
#39785=CARTESIAN_POINT('Ctrl Pts',(374.027987994458,-22.9119390419953,-0.432829937472582));
#39786=CARTESIAN_POINT('Ctrl Pts',(374.024186473679,-22.9102219817883,-0.460009603363318));
#39787=CARTESIAN_POINT('Ctrl Pts',(373.988638411203,-22.8954139474487,-0.692482710099291));
#39788=CARTESIAN_POINT('Ctrl Pts',(373.937463810628,-22.8816968156054,-0.894274997482535));
#39789=CARTESIAN_POINT('Ctrl Pts',(373.816782650418,-22.8576410161071,-1.2301603058513));
#39790=CARTESIAN_POINT('Ctrl Pts',(373.756624185978,-22.8474794350743,-1.36693720205042));
#39791=CARTESIAN_POINT('Ctrl Pts',(373.657105453504,-22.8332101838817,-1.5563337026695));
#39792=CARTESIAN_POINT('Ctrl Pts',(373.625287475591,-22.8289384670155,-1.61269773980359));
#39793=CARTESIAN_POINT('Ctrl Pts',(373.578155401195,-22.8230342560931,-1.69061149148152));
#39794=CARTESIAN_POINT('Ctrl Pts',(373.564242233459,-22.8213387867928,-1.71298706281995));
#39795=CARTESIAN_POINT('Ctrl Pts',(373.539302933239,-22.8183847488793,-1.75201944196714));
#39796=CARTESIAN_POINT('Ctrl Pts',(373.528393580486,-22.8171198176635,-1.76874883198107));
#39797=CARTESIAN_POINT('Ctrl Pts',(373.511872204583,-22.8152455968796,-1.79357667339913));
#39798=CARTESIAN_POINT('Ctrl Pts',(373.50637765528,-22.8146289362175,-1.80175220496754));
#39799=CARTESIAN_POINT('Ctrl Pts',(373.49687378055,-22.8135738345459,-1.81575425496961));
#39800=CARTESIAN_POINT('Ctrl Pts',(373.492882677434,-22.8131341944013,-1.82159289066328));
#39801=CARTESIAN_POINT('Ctrl Pts',(373.483738390691,-22.8121347447722,-1.83487611313049));
#39802=CARTESIAN_POINT('Ctrl Pts',(373.478573039406,-22.8115757696153,-1.84231214780079));
#39803=CARTESIAN_POINT('Ctrl Pts',(373.464349945175,-22.8100515033805,-1.8626046500728));
#39804=CARTESIAN_POINT('Ctrl Pts',(373.455229189856,-22.8090903767888,-1.8754169338235));
#39805=CARTESIAN_POINT('Ctrl Pts',(373.408123192149,-22.8042062133094,-1.94057372394504));
#39806=CARTESIAN_POINT('Ctrl Pts',(373.368659580733,-22.8003755574656,-1.99183673121851));
#39807=CARTESIAN_POINT('Ctrl Pts',(373.179167820705,-22.7829637510526,-2.22322682239339));
#39808=CARTESIAN_POINT('Ctrl Pts',(373.011307588369,-22.7701791185087,-2.38784271349591));
#39809=CARTESIAN_POINT('Ctrl Pts',(372.702586041308,-22.7479934127432,-2.63073698966304));
#39810=CARTESIAN_POINT('Ctrl Pts',(372.571074792703,-22.7388810476321,-2.71935089694838));
#39811=CARTESIAN_POINT('Ctrl Pts',(372.408421633394,-22.7276549040944,-2.81232208191326));
#39812=CARTESIAN_POINT('Ctrl Pts',(372.383057360193,-22.7259059833655,-2.82636941317432));
#39813=CARTESIAN_POINT('Ctrl Pts',(372.343181470897,-22.7231574342356,-2.84775568106284));
#39814=CARTESIAN_POINT('Ctrl Pts',(372.328797603426,-22.7221661884842,-2.85533047069488));
#39815=CARTESIAN_POINT('Ctrl Pts',(372.30321567839,-22.720403320069,-2.86855609233045));
#39816=CARTESIAN_POINT('Ctrl Pts',(372.292040707712,-22.7196332712365,-2.8742510238464));
#39817=CARTESIAN_POINT('Ctrl Pts',(372.266211612292,-22.7178533473739,-2.88722453959774));
#39818=CARTESIAN_POINT('Ctrl Pts',(372.251534826704,-22.71684188463,-2.89445699805788));
#39819=CARTESIAN_POINT('Ctrl Pts',(372.210975743188,-22.7140462255332,-2.9140613511023));
#39820=CARTESIAN_POINT('Ctrl Pts',(372.184982832316,-22.7122540200032,-2.92619967411106));
#39821=CARTESIAN_POINT('Ctrl Pts',(372.03561852144,-22.7019495045231,-2.9935365966455));
#39822=CARTESIAN_POINT('Ctrl Pts',(371.909048766829,-22.6931863669261,-3.04127109375586));
#39823=CARTESIAN_POINT('Ctrl Pts',(371.573536129836,-22.669918818181,-3.14424200773115));
#39824=CARTESIAN_POINT('Ctrl Pts',(371.361365461458,-22.6551387111873,-3.18667728991171));
#39825=CARTESIAN_POINT('Ctrl Pts',(371.076616937972,-22.6360103027534,-3.21439709733479));
#39826=CARTESIAN_POINT('Ctrl Pts',(371.006454044967,-22.6313577770401,-3.21891719321225));
#39827=CARTESIAN_POINT('Ctrl Pts',(370.908354709285,-22.6249836439428,-3.22201986193785));
#39828=CARTESIAN_POINT('Ctrl Pts',(370.880502680639,-22.623188672298,-3.2225394518304));
#39829=CARTESIAN_POINT('Ctrl Pts',(370.831790410131,-22.6200790425069,-3.22281649543114));
#39830=CARTESIAN_POINT('Ctrl Pts',(370.810933063276,-22.6187571049461,-3.22273265346978));
#39831=CARTESIAN_POINT('Ctrl Pts',(370.780053632795,-22.6168155135291,-3.22230871445646));
#39832=CARTESIAN_POINT('Ctrl Pts',(370.770030426685,-22.6161877149443,-3.22212432876341));
#39833=CARTESIAN_POINT('Ctrl Pts',(370.752172616245,-22.6150737179957,-3.22171245610256));
#39834=CARTESIAN_POINT('Ctrl Pts',(370.744337824636,-22.6145865334719,-3.22150315667842));
#39835=CARTESIAN_POINT('Ctrl Pts',(370.727276768108,-22.6135290643111,-3.22098509491697));
#39836=CARTESIAN_POINT('Ctrl Pts',(370.718051039864,-22.612959397355,-3.22066527423341));
#39837=CARTESIAN_POINT('Ctrl Pts',(370.692333841999,-22.6113771207536,-3.21966310812248));
#39838=CARTESIAN_POINT('Ctrl Pts',(370.675845785337,-22.6103692128702,-3.21889369494802));
#39839=CARTESIAN_POINT('Ctrl Pts',(370.583254402348,-22.6047422436662,-3.21385975027898));
#39840=CARTESIAN_POINT('Ctrl Pts',(370.507309001395,-22.6002524158567,-3.20702268835355));
#39841=CARTESIAN_POINT('Ctrl Pts',(370.406620101294,-22.5943837805416,-3.19434339418074));
#39842=CARTESIAN_POINT('Ctrl Pts',(370.38160615894,-22.5929328169873,-3.19089442892033));
#39843=CARTESIAN_POINT('Ctrl Pts',(370.118439190809,-22.577717848968,-3.15145156950783));
#39844=CARTESIAN_POINT('Ctrl Pts',(369.884993756802,-22.5645969140588,-3.08916200989525));
#39845=CARTESIAN_POINT('Ctrl Pts',(369.551343008246,-22.544106370614,-2.95869407315529));
#39846=CARTESIAN_POINT('Ctrl Pts',(369.4444532531,-22.5372642585771,-2.91001152634442));
#39847=CARTESIAN_POINT('Ctrl Pts',(369.316567139063,-22.528601226433,-2.84311056161835));
#39848=CARTESIAN_POINT('Ctrl Pts',(369.29282879917,-22.5269723726417,-2.83031028776976));
#39849=CARTESIAN_POINT('Ctrl Pts',(369.255426819647,-22.5243714032571,-2.80953214587484));
#39850=CARTESIAN_POINT('Ctrl Pts',(369.241656142435,-22.5234062343577,-2.80174881737241));
#39851=CARTESIAN_POINT('Ctrl Pts',(369.215823303253,-22.5215811106365,-2.78689583881151));
#39852=CARTESIAN_POINT('Ctrl Pts',(369.203748724746,-22.5207219737441,-2.77984843690317));
#39853=CARTESIAN_POINT('Ctrl Pts',(369.176623228777,-22.518778035624,-2.76377893751879));
#39854=CARTESIAN_POINT('Ctrl Pts',(369.161599469324,-22.5176916218334,-2.75471208514711));
#39855=CARTESIAN_POINT('Ctrl Pts',(369.123211731119,-22.5148901899874,-2.7311152257372));
#39856=CARTESIAN_POINT('Ctrl Pts',(369.099958795823,-22.5131687122187,-2.71640812875586));
#39857=CARTESIAN_POINT('Ctrl Pts',(368.90747694444,-22.4987090372795,-2.59118756795139));
#39858=CARTESIAN_POINT('Ctrl Pts',(368.748830111933,-22.4853805015065,-2.46529592096053));
#39859=CARTESIAN_POINT('Ctrl Pts',(368.439693774064,-22.4565270836035,-2.16867212810489));
#39860=CARTESIAN_POINT('Ctrl Pts',(368.293313226137,-22.4410072626153,-1.99516127724561));
#39861=CARTESIAN_POINT('Ctrl Pts',(368.147390020781,-22.4242069970067,-1.77979643637953));
#39862=CARTESIAN_POINT('Ctrl Pts',(368.128898570412,-22.4220495410153,-1.75156023204495));
#39863=CARTESIAN_POINT('Ctrl Pts',(368.104362843625,-22.4191526926294,-1.71277861331031));
#39864=CARTESIAN_POINT('Ctrl Pts',(368.097930317653,-22.4183898949876,-1.70248295112186));
#39865=CARTESIAN_POINT('Ctrl Pts',(368.087263688831,-22.4171196971502,-1.68519370053065));
#39866=CARTESIAN_POINT('Ctrl Pts',(368.082997792968,-22.4166102586024,-1.67821998582673));
#39867=CARTESIAN_POINT('Ctrl Pts',(368.074958850116,-22.4156475845874,-1.66496520646447));
#39868=CARTESIAN_POINT('Ctrl Pts',(368.071180622507,-22.4151940019205,-1.65868740078578));
#39869=CARTESIAN_POINT('Ctrl Pts',(368.062284800896,-22.4141232066181,-1.64379158544372));
#39870=CARTESIAN_POINT('Ctrl Pts',(368.057185900619,-22.4135071945503,-1.63516242116217));
#39871=CARTESIAN_POINT('Ctrl Pts',(368.039474953511,-22.4113590235147,-1.60486734382766));
#39872=CARTESIAN_POINT('Ctrl Pts',(368.027075158065,-22.4098398026188,-1.58307756077528));
#39873=CARTESIAN_POINT('Ctrl Pts',(367.907781650956,-22.3950489428594,-1.3676365184546));
#39874=CARTESIAN_POINT('Ctrl Pts',(367.820824017495,-22.3828236105416,-1.16358333373568));
#39875=CARTESIAN_POINT('Ctrl Pts',(367.691924192908,-22.3584158248751,-0.746798412283902));
#39876=CARTESIAN_POINT('Ctrl Pts',(367.649119630298,-22.3462892245306,-0.535576541975873));
#39877=CARTESIAN_POINT('Ctrl Pts',(367.624416628219,-22.3315008076421,-0.289325118867448));
#39878=CARTESIAN_POINT('Ctrl Pts',(367.621660915153,-22.3295433778472,-0.256924465194356));
#39879=CARTESIAN_POINT('Ctrl Pts',(367.618212063996,-22.3265394617365,-0.207533134624308));
#39880=CARTESIAN_POINT('Ctrl Pts',(367.617162288861,-22.3255041358149,-0.190568903346805));
#39881=CARTESIAN_POINT('Ctrl Pts',(367.615495769845,-22.323611878576,-0.159675719927475));
#39882=CARTESIAN_POINT('Ctrl Pts',(367.614835127737,-22.3227563439161,-0.145749478905231));
#39883=CARTESIAN_POINT('Ctrl Pts',(367.613601405335,-22.3208992680427,-0.11561243796431));
#39884=CARTESIAN_POINT('Ctrl Pts',(367.613060312588,-22.3198967486611,-0.0994007798438235));
#39885=CARTESIAN_POINT('Ctrl Pts',(367.611917262764,-22.3171492188841,-0.0551320548488592));
#39886=CARTESIAN_POINT('Ctrl Pts',(367.61155937483,-22.3153966428901,-0.0270706258412181));
#39887=CARTESIAN_POINT('Ctrl Pts',(367.611612283881,-22.3045829565581,0.144955229369807));
#39888=CARTESIAN_POINT('Ctrl Pts',(367.621302827077,-22.2952341305359,0.288734706018177));
#39889=CARTESIAN_POINT('Ctrl Pts',(367.668697853027,-22.2717071754967,0.639635700406626));
#39890=CARTESIAN_POINT('Ctrl Pts',(367.717129037138,-22.2573193439216,0.844635775710463));
#39891=CARTESIAN_POINT('Ctrl Pts',(367.794265431603,-22.2413995174392,1.07004133787955));
#39892=CARTESIAN_POINT('Ctrl Pts',(367.803711225707,-22.2395293705156,1.09650842504543));
#39893=CARTESIAN_POINT('Ctrl Pts',(367.839622605778,-22.232707118368,1.19312128143747));
#39894=CARTESIAN_POINT('Ctrl Pts',(367.868189489768,-22.2278184363116,1.26246681312823));
#39895=CARTESIAN_POINT('Ctrl Pts',(367.905938017425,-22.2220108502679,1.34572627218807));
#39896=CARTESIAN_POINT('Ctrl Pts',(367.912838908949,-22.2209728885945,1.36064266692296));
#39897=CARTESIAN_POINT('Ctrl Pts',(367.923786854749,-22.2193633906209,1.38383950884999));
#39898=CARTESIAN_POINT('Ctrl Pts',(367.927755717288,-22.218787280989,1.3921562535321));
#39899=CARTESIAN_POINT('Ctrl Pts',(367.935166745954,-22.217725186406,1.40751620618379));
#39900=CARTESIAN_POINT('Ctrl Pts',(367.938598923244,-22.2172386271057,1.4145638529164));
#39901=CARTESIAN_POINT('Ctrl Pts',(367.94648827149,-22.2161321737461,1.43061482901119));
#39902=CARTESIAN_POINT('Ctrl Pts',(367.950961845366,-22.2155133060001,1.43960988479592));
#39903=CARTESIAN_POINT('Ctrl Pts',(367.964901739796,-22.2136105332993,1.46731330447654));
#39904=CARTESIAN_POINT('Ctrl Pts',(367.974508836153,-22.2123350374289,1.48595074080188));
#39905=CARTESIAN_POINT('Ctrl Pts',(367.99738965047,-22.2093763805,1.52929475126235));
#39906=CARTESIAN_POINT('Ctrl Pts',(368.010805505982,-22.2077010518569,1.55392477219541));
#39907=CARTESIAN_POINT('Ctrl Pts',(368.059316331355,-22.2018369392941,1.64028217133379));
#39908=CARTESIAN_POINT('Ctrl Pts',(368.096129599397,-22.197730103909,1.70102480492215));
#39909=CARTESIAN_POINT('Ctrl Pts',(368.254939960526,-22.1811378152163,1.94452995984583));
#39910=CARTESIAN_POINT('Ctrl Pts',(368.393462738948,-22.1691209599349,2.11580246317889));
#39911=CARTESIAN_POINT('Ctrl Pts',(368.64040486064,-22.1491868929606,2.36430183950861));
#39912=CARTESIAN_POINT('Ctrl Pts',(368.738009099589,-22.1416117265743,2.4512570863769));
#39913=CARTESIAN_POINT('Ctrl Pts',(368.862973301372,-22.1320796498359,2.54965257543158));
#39914=CARTESIAN_POINT('Ctrl Pts',(368.885566281338,-22.1303627967389,2.56696217932471));
#39915=CARTESIAN_POINT('Ctrl Pts',(368.921462920414,-22.1276435501531,2.59371733483017));
#39916=CARTESIAN_POINT('Ctrl Pts',(368.934614438044,-22.1266490679695,2.60336523101493));
#39917=CARTESIAN_POINT('Ctrl Pts',(368.959030464327,-22.1248057593544,2.62099319469931));
#39918=CARTESIAN_POINT('Ctrl Pts',(368.970274148213,-22.1239580523437,2.62900155458907));
#39919=CARTESIAN_POINT('Ctrl Pts',(368.99534035114,-22.122070553859,2.6466134193754));
#39920=CARTESIAN_POINT('Ctrl Pts',(369.009187278973,-22.1210294354912,2.65618132184698));
#39921=CARTESIAN_POINT('Ctrl Pts',(369.049340282527,-22.1180145410628,2.68346388750705));
#39922=CARTESIAN_POINT('Ctrl Pts',(369.075833135174,-22.1160303426408,2.70089887711048));
#39923=CARTESIAN_POINT('Ctrl Pts',(369.297491488857,-22.09946532088,2.84212885786059));
#39924=CARTESIAN_POINT('Ctrl Pts',(369.505161956313,-22.0841020747728,2.94496841624281));
#39925=CARTESIAN_POINT('Ctrl Pts',(369.91455574407,-22.0546224190185,3.09552057882965));
#39926=CARTESIAN_POINT('Ctrl Pts',(370.113449153496,-22.0406456606377,3.14778838051105));
#39927=CARTESIAN_POINT('Ctrl Pts',(370.341597952414,-22.0258073034496,3.1849676061297));
#39928=CARTESIAN_POINT('Ctrl Pts',(370.367271750704,-22.02415470334,3.18883357826953));
#39929=CARTESIAN_POINT('Ctrl Pts',(370.403067826214,-22.0218769940768,3.19378215793963));
#39930=CARTESIAN_POINT('Ctrl Pts',(370.413151967347,-22.0212382523578,3.19512759702493));
#39931=CARTESIAN_POINT('Ctrl Pts',(370.430547459083,-22.0201416176846,3.19736473940421));
#39932=CARTESIAN_POINT('Ctrl Pts',(370.437855736055,-22.0196824793025,3.19827916233054));
#39933=CARTESIAN_POINT('Ctrl Pts',(370.453239805592,-22.0187194094488,3.20015049893188));
#39934=CARTESIAN_POINT('Ctrl Pts',(370.461316189459,-22.0182158051448,3.20110191265379));
#39935=CARTESIAN_POINT('Ctrl Pts',(370.481250456995,-22.0169775249502,3.20337374119091));
#39936=CARTESIAN_POINT('Ctrl Pts',(370.493112381309,-22.0162448028569,3.20465891294888));
#39937=CARTESIAN_POINT('Ctrl Pts',(370.537078155534,-22.0135433401442,3.20917547031835));
#39938=CARTESIAN_POINT('Ctrl Pts',(370.569224035159,-22.0115964460134,3.21199067333927));
#39939=CARTESIAN_POINT('Ctrl Pts',(370.803393819919,-21.9975846718547,3.22895860734334));
#39940=CARTESIAN_POINT('Ctrl Pts',(371.006335553882,-21.9863442066119,3.22452483097958));
#39941=CARTESIAN_POINT('Ctrl Pts',(371.416293280266,-21.9632631396498,3.17672679826232));
#39942=CARTESIAN_POINT('Ctrl Pts',(371.622141640787,-21.9514553842187,3.13202951747999));
#39943=CARTESIAN_POINT('Ctrl Pts',(371.857966820673,-21.9367480102533,3.05608821134147));
#39944=CARTESIAN_POINT('Ctrl Pts',(371.893564299402,-21.934496363534,3.04393317186487));
#39945=CARTESIAN_POINT('Ctrl Pts',(371.948149643752,-21.9309907019908,3.0242211304565));
#39946=CARTESIAN_POINT('Ctrl Pts',(371.967292738687,-21.9297510888913,3.01710168585497));
#39947=CARTESIAN_POINT('Ctrl Pts',(371.999702433401,-21.927634477982,3.00469636487816));
#39948=CARTESIAN_POINT('Ctrl Pts',(372.013004084916,-21.9267606018636,2.99950332917185));
#39949=CARTESIAN_POINT('Ctrl Pts',(372.039870571419,-21.9249848593066,2.98880820319062));
#39950=CARTESIAN_POINT('Ctrl Pts',(372.053433297567,-21.9240828625618,2.98330175374703));
#39951=CARTESIAN_POINT('Ctrl Pts',(372.086826013824,-21.9218480528061,2.96947861699129));
#39952=CARTESIAN_POINT('Ctrl Pts',(372.106610952183,-21.9205116628002,2.96105558602107));
#39953=CARTESIAN_POINT('Ctrl Pts',(372.180601611237,-21.9154667081681,2.92867711883052));
#39954=CARTESIAN_POINT('Ctrl Pts',(372.234224708035,-21.911714342546,2.90342722946176));
#39955=CARTESIAN_POINT('Ctrl Pts',(372.294701480411,-21.9073686153834,2.87288520306915));
#39956=CARTESIAN_POINT('Ctrl Pts',(372.3022688911,-21.9068227714453,2.8690258740493));
#39957=CARTESIAN_POINT('Ctrl Pts',(372.30982061585,-21.9062759889522,2.86513684838664));
#39958=CARTESIAN_POINT('',(367.611568766713,-22.0642265507751,0.00242649832743659));
#39959=CARTESIAN_POINT('Ctrl Pts',(372.309820475366,-21.6596622257337,2.86513692073373));
#39960=CARTESIAN_POINT('Ctrl Pts',(372.15720255111,-21.6696054137955,2.94373286698527));
#39961=CARTESIAN_POINT('Ctrl Pts',(371.998464664616,-21.6791174589537,3.01005219247402));
#39962=CARTESIAN_POINT('Ctrl Pts',(371.636719776143,-21.7004247473343,3.12823047273937));
#39963=CARTESIAN_POINT('Ctrl Pts',(371.432535462295,-21.7122360244881,3.17360910930486));
#39964=CARTESIAN_POINT('Ctrl Pts',(371.198185196885,-21.7263662855851,3.20226021354722));
#39965=CARTESIAN_POINT('Ctrl Pts',(371.170918071698,-21.7280182410862,3.20524104274543));
#39966=CARTESIAN_POINT('Ctrl Pts',(371.12616871568,-21.7307437208177,3.20955571750068));
#39967=CARTESIAN_POINT('Ctrl Pts',(371.108707434098,-21.7318107829302,3.2110956336877));
#39968=CARTESIAN_POINT('Ctrl Pts',(371.07729088784,-21.7337374368571,3.21360814988941));
#39969=CARTESIAN_POINT('Ctrl Pts',(371.063340117727,-21.7345953834297,3.21463248742269));
#39970=CARTESIAN_POINT('Ctrl Pts',(371.033567836235,-21.7364316297104,3.21662373527376));
#39971=CARTESIAN_POINT('Ctrl Pts',(371.017745022203,-21.7374107164302,3.21756480422641));
#39972=CARTESIAN_POINT('Ctrl Pts',(370.974867390853,-21.7400728472851,3.21979766576227));
#39973=CARTESIAN_POINT('Ctrl Pts',(370.947802656645,-21.7417628521499,3.22086514905843));
#39974=CARTESIAN_POINT('Ctrl Pts',(370.801742683221,-21.7509374969785,3.22478281290298));
#39975=CARTESIAN_POINT('Ctrl Pts',(370.682685366382,-21.7586150860404,3.22137970072268));
#39976=CARTESIAN_POINT('Ctrl Pts',(370.408531303646,-21.7767436642974,3.19831148923421));
#39977=CARTESIAN_POINT('Ctrl Pts',(370.254129888967,-21.7872951779175,3.17393535632644));
#39978=CARTESIAN_POINT('Ctrl Pts',(369.938826625605,-21.8091971328656,3.10037537880386));
#39979=CARTESIAN_POINT('Ctrl Pts',(369.778743908101,-21.8205155936598,3.04959117024204));
#39980=CARTESIAN_POINT('Ctrl Pts',(369.598359065231,-21.8330214872617,2.97644913027678));
#39981=CARTESIAN_POINT('Ctrl Pts',(369.57351646754,-21.8347377708286,2.96601138345266));
#39982=CARTESIAN_POINT('Ctrl Pts',(369.539334873628,-21.8370879920982,2.95114271732617));
#39983=CARTESIAN_POINT('Ctrl Pts',(369.529882678033,-21.8377366928928,2.94697694867391));
#39984=CARTESIAN_POINT('Ctrl Pts',(369.513685020318,-21.8388460565771,2.93974512149232));
#39985=CARTESIAN_POINT('Ctrl Pts',(369.506929871898,-21.8393080276134,2.93670114385904));
#39986=CARTESIAN_POINT('Ctrl Pts',(369.49281133788,-21.8402720401648,2.93028043898301));
#39987=CARTESIAN_POINT('Ctrl Pts',(369.485450104011,-21.8407737821897,2.92689920884158));
#39988=CARTESIAN_POINT('Ctrl Pts',(369.468492659415,-21.8419277316657,2.91903259752636));
#39989=CARTESIAN_POINT('Ctrl Pts',(369.45890556076,-21.8425787442681,2.91452754293065));
#39990=CARTESIAN_POINT('Ctrl Pts',(369.424775032174,-21.8448920300211,2.8982834175181));
#39991=CARTESIAN_POINT('Ctrl Pts',(369.400357482516,-21.8465389339236,2.88628056483274));
#39992=CARTESIAN_POINT('Ctrl Pts',(369.340679306922,-21.8505512477435,2.85600044460679));
#39993=CARTESIAN_POINT('Ctrl Pts',(369.305598226387,-21.8528986613721,2.83737752672048));
#39994=CARTESIAN_POINT('Ctrl Pts',(369.163484569218,-21.8623982678518,2.75853480965307));
#39995=CARTESIAN_POINT('Ctrl Pts',(369.059585121429,-21.8693229051471,2.69286581003269));
#39996=CARTESIAN_POINT('Ctrl Pts',(368.747824252617,-21.8907998418315,2.46991876110876));
#39997=CARTESIAN_POINT('Ctrl Pts',(368.555137462499,-21.9052073193631,2.2933113135743));
#39998=CARTESIAN_POINT('Ctrl Pts',(368.360225706862,-21.9230317259545,2.06555886163211));
#39999=CARTESIAN_POINT('Ctrl Pts',(368.335195661523,-21.9253916888148,2.03520353475155));
#40000=CARTESIAN_POINT('Ctrl Pts',(368.299444921123,-21.928872625577,1.99019243067548));
#40001=CARTESIAN_POINT('Ctrl Pts',(368.288281822289,-21.9299759351463,1.97589149533118));
#40002=CARTESIAN_POINT('Ctrl Pts',(368.268660770095,-21.9319450354443,1.95031279403572));
#40003=CARTESIAN_POINT('Ctrl Pts',(368.260154884994,-21.9328089074328,1.93907226936395));
#40004=CARTESIAN_POINT('Ctrl Pts',(368.242545577739,-21.9346191225584,1.91548151313104));
#40005=CARTESIAN_POINT('Ctrl Pts',(368.233456078819,-21.9355659783712,1.90312137620516));
#40006=CARTESIAN_POINT('Ctrl Pts',(368.209928759807,-21.9380499912831,1.87064495639728));
#40007=CARTESIAN_POINT('Ctrl Pts',(368.195634126757,-21.9395925983478,1.85042665438473));
#40008=CARTESIAN_POINT('Ctrl Pts',(368.1314320321,-21.9466773620323,1.75736249585734));
#40009=CARTESIAN_POINT('Ctrl Pts',(368.08430257063,-21.9523224934432,1.6826551156313));
#40010=CARTESIAN_POINT('Ctrl Pts',(367.971273251686,-21.9670814143888,1.48602779920037));
#40011=CARTESIAN_POINT('Ctrl Pts',(367.910063524424,-21.9763319528122,1.36162881281598));
#40012=CARTESIAN_POINT('Ctrl Pts',(367.806771086688,-21.9945387165853,1.11235280351233));
#40013=CARTESIAN_POINT('Ctrl Pts',(367.763956825202,-22.0034674198314,0.988054720714536));
#40014=CARTESIAN_POINT('Ctrl Pts',(367.719479566163,-22.0145941420502,0.827724497566529));
#40015=CARTESIAN_POINT('Ctrl Pts',(367.710663772789,-22.0169259591233,0.793807730461049));
#40016=CARTESIAN_POINT('Ctrl Pts',(367.685633394994,-22.0239416283017,0.690625496999164));
#40017=CARTESIAN_POINT('Ctrl Pts',(367.671155987291,-22.0285729763092,0.620955764132295));
#40018=CARTESIAN_POINT('Ctrl Pts',(367.65622806814,-22.0341194728747,0.534906541002544));
#40019=CARTESIAN_POINT('Ctrl Pts',(367.65358086441,-22.0351417551776,0.518933447614696));
#40020=CARTESIAN_POINT('Ctrl Pts',(367.649624001201,-22.0367324567524,0.493889263945372));
#40021=CARTESIAN_POINT('Ctrl Pts',(367.648232508244,-22.0373052803712,0.484831636289578));
#40022=CARTESIAN_POINT('Ctrl Pts',(367.645720503549,-22.0383648473461,0.468002302179814));
#40023=CARTESIAN_POINT('Ctrl Pts',(367.644589763945,-22.0388521349285,0.460232475466851));
#40024=CARTESIAN_POINT('Ctrl Pts',(367.642410505258,-22.0398122952688,0.44486388903691));
#40025=CARTESIAN_POINT('Ctrl Pts',(367.641360720088,-22.0402852380351,0.437265533234733));
#40026=CARTESIAN_POINT('Ctrl Pts',(367.639007558378,-22.0413701111036,0.419772884890152));
#40027=CARTESIAN_POINT('Ctrl Pts',(367.637722984271,-22.0419810181206,0.409876084887379));
#40028=CARTESIAN_POINT('Ctrl Pts',(367.634520268729,-22.0435545488452,0.384270000244196));
#40029=CARTESIAN_POINT('Ctrl Pts',(367.632671806503,-22.0445135623278,0.368552070056182));
#40030=CARTESIAN_POINT('Ctrl Pts',(367.618127851558,-22.0525175341208,0.236502619217367));
#40031=CARTESIAN_POINT('Ctrl Pts',(367.611660397471,-22.0592628964552,0.119562495099769));
#40032=CARTESIAN_POINT('Ctrl Pts',(367.611568839302,-22.0658953423866,0.0025210645287454));
#40033=CARTESIAN_POINT('Ctrl Pts',(367.611568766713,-22.0642265507751,0.00242649832743659));
#40034=CARTESIAN_POINT('Ctrl Pts',(367.61149490218,-22.0703030074805,-0.0956765390764883));
#40035=CARTESIAN_POINT('Ctrl Pts',(367.615904730246,-22.076379464186,-0.193948280684805));
#40036=CARTESIAN_POINT('Ctrl Pts',(367.624817916114,-22.0824559208914,-0.291937863578686));
#40037=CARTESIAN_POINT('Ctrl Pts',(367.634068124722,-22.0887621387753,-0.393632599514726));
#40038=CARTESIAN_POINT('Ctrl Pts',(367.648169083226,-22.0950683566592,-0.495022935142761));
#40039=CARTESIAN_POINT('Ctrl Pts',(367.667083341441,-22.1013745745431,-0.595603147969471));
#40040=CARTESIAN_POINT('Ctrl Pts',(367.685274214606,-22.107439608042,-0.692336621399258));
#40041=CARTESIAN_POINT('Ctrl Pts',(367.707916867878,-22.1135046415409,-0.788320316617951));
#40042=CARTESIAN_POINT('Ctrl Pts',(367.734925204045,-22.1195696750397,-0.883109714992833));
#40043=CARTESIAN_POINT('Ctrl Pts',(367.761923563297,-22.1256324681073,-0.977864098039831));
#40044=CARTESIAN_POINT('Ctrl Pts',(367.793284280533,-22.1316952611748,-1.07142462983612));
#40045=CARTESIAN_POINT('Ctrl Pts',(367.8288706626,-22.1377580542424,-1.16335925099373));
#40046=CARTESIAN_POINT('Ctrl Pts',(367.864454056667,-22.1438203382491,-1.25528615288583));
#40047=CARTESIAN_POINT('Ctrl Pts',(367.904262248197,-22.1498826222559,-1.34558699777065));
#40048=CARTESIAN_POINT('Ctrl Pts',(367.94810981923,-22.1559449062627,-1.43384823011757));
#40049=CARTESIAN_POINT('Ctrl Pts',(367.991966225147,-22.162008411764,-1.52212724629151));
#40050=CARTESIAN_POINT('Ctrl Pts',(368.03986342594,-22.1680719172652,-1.60836543339431));
#40051=CARTESIAN_POINT('Ctrl Pts',(368.091569889003,-22.1741354227665,-1.69217350388752));
#40052=CARTESIAN_POINT('Ctrl Pts',(368.143331202225,-22.1802053604279,-1.77607047789136));
#40053=CARTESIAN_POINT('Ctrl Pts',(368.198909603746,-22.1862752980892,-1.85753181076433));
#40054=CARTESIAN_POINT('Ctrl Pts',(368.258030269901,-22.1923452357506,-1.93619726539244));
#40055=CARTESIAN_POINT('Ctrl Pts',(368.317188279368,-22.1984190074618,-2.01491240871425));
#40056=CARTESIAN_POINT('Ctrl Pts',(368.379892718554,-22.204492779173,-2.09082781700198));
#40057=CARTESIAN_POINT('Ctrl Pts',(368.445829956663,-22.2105665508842,-2.16361806483572));
#40058=CARTESIAN_POINT('Ctrl Pts',(368.51186647817,-22.2166494680298,-2.23651791482009));
#40059=CARTESIAN_POINT('Ctrl Pts',(368.581145192527,-22.2227323851755,-2.30628290284342));
#40060=CARTESIAN_POINT('Ctrl Pts',(368.65331761671,-22.2288153023212,-2.37262629396778));
#40061=CARTESIAN_POINT('Ctrl Pts',(368.673052085238,-22.2304785849159,-2.39076690070184));
#40062=CARTESIAN_POINT('Ctrl Pts',(368.693002731649,-22.2321418675107,-2.4086519303531));
#40063=CARTESIAN_POINT('Ctrl Pts',(368.713162052515,-22.2338051501055,-2.42627608313987));
#40064=CARTESIAN_POINT('Ctrl Pts',(368.7879867928,-22.2399787057032,-2.49169111690126));
#40065=CARTESIAN_POINT('Ctrl Pts',(368.865971414356,-22.2461522613009,-2.55375612836349));
#40066=CARTESIAN_POINT('Ctrl Pts',(368.946783406865,-22.2523258168986,-2.61215069938684));
#40067=CARTESIAN_POINT('Ctrl Pts',(369.027486316182,-22.2584910391893,-2.67046644713183));
#40068=CARTESIAN_POINT('Ctrl Pts',(369.111008661803,-22.2646562614799,-2.72512135014984));
#40069=CARTESIAN_POINT('Ctrl Pts',(369.196983264425,-22.2708214837706,-2.77583374985307));
#40070=CARTESIAN_POINT('Ctrl Pts',(369.282867184459,-22.2769802032302,-2.82649266013559));
#40071=CARTESIAN_POINT('Ctrl Pts',(369.371197847217,-22.2831389226898,-2.8732171151454));
#40072=CARTESIAN_POINT('Ctrl Pts',(369.461578149132,-22.2892976421493,-2.91576804072415));
#40073=CARTESIAN_POINT('Ctrl Pts',(369.551892819251,-22.295451889309,-2.95828806694153));
#40074=CARTESIAN_POINT('Ctrl Pts',(369.644253777684,-22.3016061364688,-2.9966404049843));
#40075=CARTESIAN_POINT('Ctrl Pts',(369.738239120822,-22.3077603836285,-3.03063177817354));
#40076=CARTESIAN_POINT('Ctrl Pts',(369.832189133076,-22.3139123172893,-3.06461037335698));
#40077=CARTESIAN_POINT('Ctrl Pts',(369.927761908852,-22.3200642509501,-3.09423111367641));
#40078=CARTESIAN_POINT('Ctrl Pts',(370.024516181735,-22.3262161846108,-3.11934910123139));
#40079=CARTESIAN_POINT('Ctrl Pts',(370.121259931609,-22.3323674491864,-3.14446435695037));
#40080=CARTESIAN_POINT('Ctrl Pts',(370.219184502878,-22.338518713762,-3.1650777244909));
#40081=CARTESIAN_POINT('Ctrl Pts',(370.317835081649,-22.3446699783376,-3.18109464008319));
#40082=CARTESIAN_POINT('Ctrl Pts',(370.416501286305,-22.3508222172506,-3.19711409269532));
#40083=CARTESIAN_POINT('Ctrl Pts',(370.515893298302,-22.3569744561636,-3.20853557764327));
#40084=CARTESIAN_POINT('Ctrl Pts',(370.615548765499,-22.3631266950766,-3.21531610401774));
#40085=CARTESIAN_POINT('Ctrl Pts',(370.715310527321,-22.3692854960975,-3.22210386264477));
#40086=CARTESIAN_POINT('Ctrl Pts',(370.815335871493,-22.3754442971184,-3.22424074843573));
#40087=CARTESIAN_POINT('Ctrl Pts',(370.915160130291,-22.3816030981393,-3.22173588128178));
#40088=CARTESIAN_POINT('Ctrl Pts',(371.015040260087,-22.3877653462017,-3.21922961216972));
#40089=CARTESIAN_POINT('Ctrl Pts',(371.114718647339,-22.3939275942641,-3.21207644735806));
#40090=CARTESIAN_POINT('Ctrl Pts',(371.213735526934,-22.4000898423265,-3.20033744961007));
#40091=CARTESIAN_POINT('Ctrl Pts',(371.312916739533,-22.4062623175416,-3.18857896927706));
#40092=CARTESIAN_POINT('Ctrl Pts',(371.411433823139,-22.4124347927566,-3.17221952512817));
#40093=CARTESIAN_POINT('Ctrl Pts',(371.508836858696,-22.4186072679716,-3.15137139571912));
#40094=CARTESIAN_POINT('Ctrl Pts',(371.580973515862,-22.4231786011534,-3.1359312777072));
#40095=CARTESIAN_POINT('Ctrl Pts',(371.652499354296,-22.4277499343352,-3.11803024189166));
#40096=CARTESIAN_POINT('Ctrl Pts',(371.723237922332,-22.432321267517,-3.09773121384613));
#40097=CARTESIAN_POINT('Ctrl Pts',(371.818769919459,-22.4384948246092,-3.07031750244726));
#40098=CARTESIAN_POINT('Ctrl Pts',(371.913199866761,-22.4446683817013,-3.03843243676399));
#40099=CARTESIAN_POINT('Ctrl Pts',(372.006078257194,-22.4508419387934,-3.00218172637621));
#40100=CARTESIAN_POINT('Ctrl Pts',(372.098831277111,-22.4570071626011,-2.96597994847164));
#40101=CARTESIAN_POINT('Ctrl Pts',(372.190036502055,-22.4631723864089,-2.92542439530771));
#40102=CARTESIAN_POINT('Ctrl Pts',(372.279258200579,-22.4693376102166,-2.88067092099817));
#40103=CARTESIAN_POINT('Ctrl Pts',(372.368385791926,-22.4754963312137,-2.8359646507122));
#40104=CARTESIAN_POINT('Ctrl Pts',(372.455533630333,-22.4816550522108,-2.78706945586543));
#40105=CARTESIAN_POINT('Ctrl Pts',(372.54028554618,-22.4878137732079,-2.73418942158186));
#40106=CARTESIAN_POINT('Ctrl Pts',(372.624975917764,-22.4939680219291,-2.6813477871705));
#40107=CARTESIAN_POINT('Ctrl Pts',(372.7072734587,-22.5001222706504,-2.62452729563315));
#40108=CARTESIAN_POINT('Ctrl Pts',(372.786787039032,-22.5062765193716,-2.56397769900044));
#40109=CARTESIAN_POINT('Ctrl Pts',(372.866270728882,-22.5124284546081,-2.50345086397094));
#40110=CARTESIAN_POINT('Ctrl Pts',(372.942972192604,-22.5185803898446,-2.43919797207752));
#40111=CARTESIAN_POINT('Ctrl Pts',(373.016530456563,-22.5247323250811,-2.37151127265513));
#40112=CARTESIAN_POINT('Ctrl Pts',(373.090080720462,-22.5308835912447,-2.30383193471127));
#40113=CARTESIAN_POINT('Ctrl Pts',(373.160488144793,-22.5370348574083,-2.23271982573149));
#40114=CARTESIAN_POINT('Ctrl Pts',(373.227426707879,-22.5431861235718,-2.15850586570228));
#40115=CARTESIAN_POINT('Ctrl Pts',(373.294375873894,-22.5493383640831,-2.08428015033702));
#40116=CARTESIAN_POINT('Ctrl Pts',(373.357854796475,-22.5554906045944,-2.00695193042528));
#40117=CARTESIAN_POINT('Ctrl Pts',(373.417576704477,-22.5616428451056,-1.92688641853166));
#40118=CARTESIAN_POINT('Ctrl Pts',(373.477362313167,-22.5678016477307,-1.84673550701894));
#40119=CARTESIAN_POINT('Ctrl Pts',(373.533382645166,-22.5739604503557,-1.76384182205795));
#40120=CARTESIAN_POINT('Ctrl Pts',(373.585393463147,-22.5801192529807,-1.67860077176959));
#40121=CARTESIAN_POINT('Ctrl Pts',(373.637433391291,-22.5862815026529,-1.59331201254414));
#40122=CARTESIAN_POINT('Ctrl Pts',(373.685459127654,-22.5924437523252,-1.50567365227615));
#40123=CARTESIAN_POINT('Ctrl Pts',(373.729272740669,-22.5986060019974,-1.41610513810223));
#40124=CARTESIAN_POINT('Ctrl Pts',(373.773159068715,-22.6047784788148,-1.32638797201701));
#40125=CARTESIAN_POINT('Ctrl Pts',(373.812819137771,-22.6109509556321,-1.23473465216716));
#40126=CARTESIAN_POINT('Ctrl Pts',(373.848103390945,-22.6171234324495,-1.14158411653432));
#40127=CARTESIAN_POINT('Ctrl Pts',(373.874234801161,-22.6216947499426,-1.07259711413171));
#40128=CARTESIAN_POINT('Ctrl Pts',(373.897967168603,-22.6262660674357,-1.00278930654557));
#40129=CARTESIAN_POINT('Ctrl Pts',(373.919257714423,-22.6308373849288,-0.932343078103629));
#40130=CARTESIAN_POINT('Ctrl Pts',(373.948010513183,-22.6370109313029,-0.837205722445122));
#40131=CARTESIAN_POINT('Ctrl Pts',(373.972408582359,-22.643184477677,-0.740570465601611));
#40132=CARTESIAN_POINT('Ctrl Pts',(373.99229706809,-22.6493580240511,-0.642872336453218));
#40133=CARTESIAN_POINT('Ctrl Pts',(374.012158707525,-22.6555232371186,-0.545306084256246));
#40134=CARTESIAN_POINT('Ctrl Pts',(374.027522776871,-22.661688450186,-0.446680233157299));
#40135=CARTESIAN_POINT('Ctrl Pts',(374.038284026963,-22.6678536632534,-0.347445420230547));
#40136=CARTESIAN_POINT('Ctrl Pts',(374.04903392652,-22.674012373502,-0.248315276194083));
#40137=CARTESIAN_POINT('Ctrl Pts',(374.055190612357,-22.6801710837505,-0.148577876587435));
#40138=CARTESIAN_POINT('Ctrl Pts',(374.056699968837,-22.6863297939991,-0.0486935671092582));
#40139=CARTESIAN_POINT('Ctrl Pts',(374.058208229274,-22.6924840320034,0.0511182098073811));
#40140=CARTESIAN_POINT('Ctrl Pts',(374.055075863433,-22.6986382700078,0.151076251681782));
#40141=CARTESIAN_POINT('Ctrl Pts',(374.047300704171,-22.7047925080121,0.250716497300676));
#40142=CARTESIAN_POINT('Ctrl Pts',(374.039528467698,-22.7109444325545,0.350319286793416));
#40143=CARTESIAN_POINT('Ctrl Pts',(374.027116939493,-22.7170963570968,0.449604085043901));
#40144=CARTESIAN_POINT('Ctrl Pts',(374.010116011264,-22.7232482816392,0.548109133190833));
#40145=CARTESIAN_POINT('Ctrl Pts',(373.99311693193,-22.729399537144,0.646603468659849));
#40146=CARTESIAN_POINT('Ctrl Pts',(373.971529518756,-22.7355507926487,0.744317794796839));
#40147=CARTESIAN_POINT('Ctrl Pts',(373.945455106497,-22.7417020481534,0.84079875939419));
#40148=CARTESIAN_POINT('Ctrl Pts',(373.919376563894,-22.7478542780537,0.93729500715171));
#40149=CARTESIAN_POINT('Ctrl Pts',(373.888809723702,-22.754006507954,1.03255708615276));
#40150=CARTESIAN_POINT('Ctrl Pts',(373.853906015083,-22.7601587378543,1.1261460363838));
#40151=CARTESIAN_POINT('Ctrl Pts',(373.818965076553,-22.7663175300076,1.21983481291871));
#40152=CARTESIAN_POINT('Ctrl Pts',(373.779678184323,-22.7724763221609,1.31184648945386));
#40153=CARTESIAN_POINT('Ctrl Pts',(373.736245199107,-22.7786351143142,1.40176147818316));
#40154=CARTESIAN_POINT('Ctrl Pts',(373.692787904219,-22.784797353576,1.49172679280622));
#40155=CARTESIAN_POINT('Ctrl Pts',(373.645180101722,-22.7909595928378,1.57959270082742));
#40156=CARTESIAN_POINT('Ctrl Pts',(373.593666955272,-22.7971218320996,1.66496549379406));
#40157=CARTESIAN_POINT('Ctrl Pts',(373.542068313422,-22.8032942987141,1.75047997838042));
#40158=CARTESIAN_POINT('Ctrl Pts',(373.486551622581,-22.8094667653285,1.83349272205318));
#40159=CARTESIAN_POINT('Ctrl Pts',(373.427404649069,-22.815639231943,1.91364009983924));
#40160=CARTESIAN_POINT('Ctrl Pts',(373.383599493119,-22.8202106554088,1.9729984773599));
#40161=CARTESIAN_POINT('Ctrl Pts',(373.337803971307,-22.8247820788746,2.03078581500396));
#40162=CARTESIAN_POINT('Ctrl Pts',(373.290148161389,-22.8293535023404,2.08686728375234));
#40163=CARTESIAN_POINT('Ctrl Pts',(373.222538649734,-22.8358390013515,2.16643031544849));
#40164=CARTESIAN_POINT('Ctrl Pts',(373.150934271423,-22.8423245003625,2.24285075309167));
#40165=CARTESIAN_POINT('Ctrl Pts',(373.075662772314,-22.8488099993736,2.31570518766263));
#40166=CARTESIAN_POINT('Ctrl Pts',(373.004120718376,-22.8549741641048,2.38494993433884));
#40167=CARTESIAN_POINT('Ctrl Pts',(372.929266562978,-22.8611383288359,2.45097319270896));
#40168=CARTESIAN_POINT('Ctrl Pts',(372.85142373199,-22.8673024935671,2.51344413829839));
#40169=CARTESIAN_POINT('Ctrl Pts',(372.773652963371,-22.8734609518727,2.57585725191674));
#40170=CARTESIAN_POINT('Ctrl Pts',(372.69289935254,-22.8796194101784,2.63472431588723));
#40171=CARTESIAN_POINT('Ctrl Pts',(372.609522090141,-22.8857778684841,2.6897523082492));
#40172=CARTESIAN_POINT('Ctrl Pts',(372.52620826623,-22.8919316410604,2.74473843197019));
#40173=CARTESIAN_POINT('Ctrl Pts',(372.440275122555,-22.8980854136366,2.79589105555995));
#40174=CARTESIAN_POINT('Ctrl Pts',(372.352112829219,-22.9042391862129,2.84295901717621));
#40175=CARTESIAN_POINT('Ctrl Pts',(372.338071363139,-22.905219287633,2.8504554554098));
#40176=CARTESIAN_POINT('Ctrl Pts',(372.323973410745,-22.9061993890532,2.8578483700235));
#40177=CARTESIAN_POINT('Ctrl Pts',(372.309820613641,-22.9071794904733,2.86513684952399));
#40178=CARTESIAN_POINT('Origin',(370.834317853224,2.31077344927308,0.));
#40179=CARTESIAN_POINT('',(372.309820613641,-24.4036702759163,2.86513684952401));
#40180=CARTESIAN_POINT('',(372.309820613613,-24.1556143901908,2.8651368495388));
#40181=CARTESIAN_POINT('',(372.309820613641,2.31077344927308,2.86513684952399));
#40182=CARTESIAN_POINT('',(367.611569215287,-23.5607734493238,-0.00296296689770666));
#40183=CARTESIAN_POINT('Ctrl Pts',(367.611569215287,-23.5607734493238,-0.00296296689770666));
#40184=CARTESIAN_POINT('Ctrl Pts',(367.611692406337,-23.5690424041229,-0.136954943290668));
#40185=CARTESIAN_POINT('Ctrl Pts',(367.620176327635,-23.577311358922,-0.270574321379934));
#40186=CARTESIAN_POINT('Ctrl Pts',(367.636856717719,-23.5855803137211,-0.402939014537645));
#40187=CARTESIAN_POINT('Ctrl Pts',(367.653537107804,-23.5938492685202,-0.535303707695356));
#40188=CARTESIAN_POINT('Ctrl Pts',(367.678413783074,-23.6021182233193,-0.66641417607396));
#40189=CARTESIAN_POINT('Ctrl Pts',(367.711269345869,-23.6103871781184,-0.795415352636087));
#40190=CARTESIAN_POINT('Ctrl Pts',(367.735803278768,-23.6165617788534,-0.891743217399455));
#40191=CARTESIAN_POINT('Ctrl Pts',(367.764841010137,-23.6227363795885,-0.987103344829856));
#40192=CARTESIAN_POINT('Ctrl Pts',(367.798290303457,-23.6289109803235,-1.08104314417068));
#40193=CARTESIAN_POINT('Ctrl Pts',(367.831694437508,-23.6350772448446,-1.17485611713065));
#40194=CARTESIAN_POINT('Ctrl Pts',(367.869498150779,-23.6412435093657,-1.2672521681585));
#40195=CARTESIAN_POINT('Ctrl Pts',(367.911558672564,-23.6474097738868,-1.35779097594902));
#40196=CARTESIAN_POINT('Ctrl Pts',(367.953574809394,-23.6535695313708,-1.448234241393));
#40197=CARTESIAN_POINT('Ctrl Pts',(367.999838642044,-23.6597292888548,-1.53682376866967));
#40198=CARTESIAN_POINT('Ctrl Pts',(368.050158604511,-23.6658890463388,-1.62313734486777));
#40199=CARTESIAN_POINT('Ctrl Pts',(368.10044194652,-23.6720443210465,-1.70938810618064));
#40200=CARTESIAN_POINT('Ctrl Pts',(368.154775331463,-23.6781995957541,-1.79336583575048));
#40201=CARTESIAN_POINT('Ctrl Pts',(368.212920796576,-23.6843548704617,-1.87467198034734));
#40202=CARTESIAN_POINT('Ctrl Pts',(368.271044343581,-23.6905078249199,-1.95594747634661));
#40203=CARTESIAN_POINT('Ctrl Pts',(368.332976863224,-23.6966607793781,-2.03455303583693));
#40204=CARTESIAN_POINT('Ctrl Pts',(368.398437009064,-23.7028137338363,-2.11011897189568));
#40205=CARTESIAN_POINT('Ctrl Pts',(368.463889952418,-23.7089660112937,-2.18567659354284));
#40206=CARTESIAN_POINT('Ctrl Pts',(368.532869466085,-23.7151182887511,-2.25819492869112));
#40207=CARTESIAN_POINT('Ctrl Pts',(368.605054499426,-23.7212705662085,-2.32733806352102));
#40208=CARTESIAN_POINT('Ctrl Pts',(368.677250858103,-23.727423808916,-2.39649204643378));
#40209=CARTESIAN_POINT('Ctrl Pts',(368.75265342196,-23.7335770516235,-2.46226947697302));
#40210=CARTESIAN_POINT('Ctrl Pts',(368.830905681368,-23.739730294331,-2.52437264130288));
#40211=CARTESIAN_POINT('Ctrl Pts',(368.909241136097,-23.7458900789711,-2.58654183174805));
#40212=CARTESIAN_POINT('Ctrl Pts',(368.99043199569,-23.7520498636111,-2.64502868519833));
#40213=CARTESIAN_POINT('Ctrl Pts',(369.074090287861,-23.7582096482512,-2.69957709292313));
#40214=CARTESIAN_POINT('Ctrl Pts',(369.157795263888,-23.7643728702374,-2.75415594030923));
#40215=CARTESIAN_POINT('Ctrl Pts',(369.243970040455,-23.7705360922235,-2.80479174516912));
#40216=CARTESIAN_POINT('Ctrl Pts',(369.332201218711,-23.7766993142097,-2.85127395716686));
#40217=CARTESIAN_POINT('Ctrl Pts',(369.420578436674,-23.7828727375233,-2.89783310623801));
#40218=CARTESIAN_POINT('Ctrl Pts',(369.511018461915,-23.7890461608368,-2.94022474592278));
#40219=CARTESIAN_POINT('Ctrl Pts',(369.603086953579,-23.7952195841504,-2.97828609006258));
#40220=CARTESIAN_POINT('Ctrl Pts',(369.67111180803,-23.799780821277,-3.00640773459576));
#40221=CARTESIAN_POINT('Ctrl Pts',(369.740025219121,-23.8043420584035,-3.03216648065162));
#40222=CARTESIAN_POINT('Ctrl Pts',(369.809647408009,-23.8089032955301,-3.05551436606063));
#40223=CARTESIAN_POINT('Ctrl Pts',(369.903886288049,-23.8150772737584,-3.08711748867723));
#40224=CARTESIAN_POINT('Ctrl Pts',(369.999753264778,-23.8212512519868,-3.11441194208328));
#40225=CARTESIAN_POINT('Ctrl Pts',(370.096818059282,-23.8274252302152,-3.13722992725036));
#40226=CARTESIAN_POINT('Ctrl Pts',(370.193752031933,-23.8335908872878,-3.16001715882533));
#40227=CARTESIAN_POINT('Ctrl Pts',(370.291880194628,-23.8397565443605,-3.17833981576138));
#40228=CARTESIAN_POINT('Ctrl Pts',(370.390755187851,-23.8459222014331,-3.19207921649617));
#40229=CARTESIAN_POINT('Ctrl Pts',(370.489526082069,-23.8520813670892,-3.20580415191577));
#40230=CARTESIAN_POINT('Ctrl Pts',(370.589041815961,-23.8582405327454,-3.21495536528608));
#40231=CARTESIAN_POINT('Ctrl Pts',(370.688843799736,-23.8643996984015,-3.21946499627839));
#40232=CARTESIAN_POINT('Ctrl Pts',(370.788573560222,-23.8705544068796,-3.22397136380465));
#40233=CARTESIAN_POINT('Ctrl Pts',(370.888588726393,-23.8767091153578,-3.2238428076631));
#40234=CARTESIAN_POINT('Ctrl Pts',(370.988425442236,-23.8828638238359,-3.21906328199818));
#40235=CARTESIAN_POINT('Ctrl Pts',(371.088224778161,-23.8890162279264,-3.21428554583794));
#40236=CARTESIAN_POINT('Ctrl Pts',(371.187845363413,-23.895168632017,-3.20486032107226));
#40237=CARTESIAN_POINT('Ctrl Pts',(371.286824087747,-23.9013210361075,-3.19082366642503));
#40238=CARTESIAN_POINT('Ctrl Pts',(371.38579218459,-23.9074727796055,-3.17678851891385));
#40239=CARTESIAN_POINT('Ctrl Pts',(371.484118127764,-23.9136245231034,-3.15814298692393));
#40240=CARTESIAN_POINT('Ctrl Pts',(371.581345671679,-23.9197762666014,-3.13497480068882));
#40241=CARTESIAN_POINT('Ctrl Pts',(371.678588739431,-23.9259289923175,-3.11180291530516));
#40242=CARTESIAN_POINT('Ctrl Pts',(371.774732637287,-23.9320817180336,-3.0841070419717));
#40243=CARTESIAN_POINT('Ctrl Pts',(371.869334006427,-23.9382344437497,-3.05202541357524));
#40244=CARTESIAN_POINT('Ctrl Pts',(371.964036410521,-23.9443937406219,-3.01990952176504));
#40245=CARTESIAN_POINT('Ctrl Pts',(372.057192584349,-23.950553037494,-2.98339866125467));
#40246=CARTESIAN_POINT('Ctrl Pts',(372.148377081947,-23.9567123343662,-2.94268005496815));
#40247=CARTESIAN_POINT('Ctrl Pts',(372.239612696557,-23.9628750840714,-2.90193862228546));
#40248=CARTESIAN_POINT('Ctrl Pts',(372.328874046053,-23.9690378337767,-2.85698494148562));
#40249=CARTESIAN_POINT('Ctrl Pts',(372.415760194849,-23.9752005834819,-2.80805229342594));
#40250=CARTESIAN_POINT('Ctrl Pts',(372.502790590456,-23.9813735644726,-2.7590384082704));
#40251=CARTESIAN_POINT('Ctrl Pts',(372.587437541014,-23.9875465454632,-2.70603259178947));
#40252=CARTESIAN_POINT('Ctrl Pts',(372.669328903666,-23.9937195264539,-2.64931161007049));
#40253=CARTESIAN_POINT('Ctrl Pts',(372.729910243236,-23.9982861552832,-2.60735073723878));
#40254=CARTESIAN_POINT('Ctrl Pts',(372.788984151554,-24.0028527841124,-2.56335756968843));
#40255=CARTESIAN_POINT('Ctrl Pts',(372.846412402545,-24.0074194129417,-2.51745766341643));
#40256=CARTESIAN_POINT('Ctrl Pts',(372.923980424882,-24.0135875333515,-2.45546091279952));
#40257=CARTESIAN_POINT('Ctrl Pts',(372.998817689026,-24.0197556537614,-2.38976601714212));
#40258=CARTESIAN_POINT('Ctrl Pts',(373.070550216883,-24.0259237741713,-2.32064266491488));
#40259=CARTESIAN_POINT('Ctrl Pts',(373.142185663187,-24.0320835467545,-2.25161286302785));
#40260=CARTESIAN_POINT('Ctrl Pts',(373.210724414209,-24.0382433193377,-2.17916412599214));
#40261=CARTESIAN_POINT('Ctrl Pts',(373.275824448159,-24.0444030919209,-2.10360716612856));
#40262=CARTESIAN_POINT('Ctrl Pts',(373.340855678201,-24.0505563542704,-2.02813006204793));
#40263=CARTESIAN_POINT('Ctrl Pts',(373.402455134041,-24.05670961662,-1.94955159369536));
#40264=CARTESIAN_POINT('Ctrl Pts',(373.460317367959,-24.0628628789695,-1.86821950292517));
#40265=CARTESIAN_POINT('Ctrl Pts',(373.51813765047,-24.069011680067,-1.78694637973033));
#40266=CARTESIAN_POINT('Ctrl Pts',(373.572225846467,-24.0751604811644,-1.70292395656945));
#40267=CARTESIAN_POINT('Ctrl Pts',(373.622317162364,-24.0813092822619,-1.61653252820172));
#40268=CARTESIAN_POINT('Ctrl Pts',(373.672389699844,-24.0874557782741,-1.53017348657084));
#40269=CARTESIAN_POINT('Ctrl Pts',(373.718468116397,-24.0936022742864,-1.44144758023228));
#40270=CARTESIAN_POINT('Ctrl Pts',(373.760331787587,-24.0997487702986,-1.35076275430425));
#40271=CARTESIAN_POINT('Ctrl Pts',(373.802191001744,-24.1058946119217,-1.26008758317269));
#40272=CARTESIAN_POINT('Ctrl Pts',(373.839836180324,-24.1120404535448,-1.16745430204368));
#40273=CARTESIAN_POINT('Ctrl Pts',(373.873093830474,-24.1181862951678,-1.07329312053637));
#40274=CARTESIAN_POINT('Ctrl Pts',(373.906356866755,-24.1243331321203,-0.979116689467482));
#40275=CARTESIAN_POINT('Ctrl Pts',(373.935230818367,-24.1304799690728,-0.88341227674254));
#40276=CARTESIAN_POINT('Ctrl Pts',(373.95959161304,-24.1366268060252,-0.786626651406925));
#40277=CARTESIAN_POINT('Ctrl Pts',(373.983978674557,-24.1427802707583,-0.689736667700208));
#40278=CARTESIAN_POINT('Ctrl Pts',(374.003842755604,-24.1489337354914,-0.591763566115745));
#40279=CARTESIAN_POINT('Ctrl Pts',(374.019110660718,-24.1550872002244,-0.493165627184254));
#40280=CARTESIAN_POINT('Ctrl Pts',(374.034387188387,-24.1612441401292,-0.394512005027022));
#40281=CARTESIAN_POINT('Ctrl Pts',(374.045062324706,-24.167401080034,-0.295233275307133));
#40282=CARTESIAN_POINT('Ctrl Pts',(374.051114866669,-24.1735580199387,-0.195792075397338));
#40283=CARTESIAN_POINT('Ctrl Pts',(374.057177561605,-24.1797252879408,-0.0961840656103151));
#40284=CARTESIAN_POINT('Ctrl Pts',(374.05860216773,-24.1858925559429,0.00358652363811422));
#40285=CARTESIAN_POINT('Ctrl Pts',(374.055419632907,-24.1920598239449,0.103057689769968));
#40286=CARTESIAN_POINT('Ctrl Pts',(374.053032843013,-24.1966850594144,0.177657588076881));
#40287=CARTESIAN_POINT('Ctrl Pts',(374.048055867032,-24.2013102948839,0.252089099841304));
#40288=CARTESIAN_POINT('Ctrl Pts',(374.040520715247,-24.2059355303535,0.32616065068505));
#40289=CARTESIAN_POINT('Ctrl Pts',(374.030446123188,-24.2121195279502,0.425195239394674));
#40290=CARTESIAN_POINT('Ctrl Pts',(374.015761345737,-24.218303525547,0.523933314390892));
#40291=CARTESIAN_POINT('Ctrl Pts',(373.996491531801,-24.2244875231438,0.621912525210338));
#40292=CARTESIAN_POINT('Ctrl Pts',(373.977247756659,-24.2306631644669,0.719759339293816));
#40293=CARTESIAN_POINT('Ctrl Pts',(373.953431343539,-24.2368388057901,0.816848906757136));
#40294=CARTESIAN_POINT('Ctrl Pts',(373.925119226506,-24.2430144471132,0.912723634742711));
#40295=CARTESIAN_POINT('Ctrl Pts',(373.89683708831,-24.2491835492381,1.00849684390231));
#40296=CARTESIAN_POINT('Ctrl Pts',(373.864068833032,-24.2553526513629,1.10305735860655));
#40297=CARTESIAN_POINT('Ctrl Pts',(373.826942315829,-24.2615217534878,1.19595835559579));
#40298=CARTESIAN_POINT('Ctrl Pts',(373.789843372054,-24.267686273893,1.28879035610646));
#40299=CARTESIAN_POINT('Ctrl Pts',(373.748392762907,-24.2738507942982,1.37996488928198));
#40300=CARTESIAN_POINT('Ctrl Pts',(373.702767705487,-24.2800153147034,1.46905173753502));
#40301=CARTESIAN_POINT('Ctrl Pts',(373.657160253058,-24.2861774564523,1.55810421052689));
#40302=CARTESIAN_POINT('Ctrl Pts',(373.607381750357,-24.2923395982011,1.64507021490609));
#40303=CARTESIAN_POINT('Ctrl Pts',(373.553656571141,-24.29850173995,1.72954170222534));
#40304=CARTESIAN_POINT('Ctrl Pts',(373.499937898263,-24.3046631354385,1.81400295970507));
#40305=CARTESIAN_POINT('Ctrl Pts',(373.442273731442,-24.310824530927,1.89596993588171));
#40306=CARTESIAN_POINT('Ctrl Pts',(373.380932693877,-24.3169859264155,1.97506212962201));
#40307=CARTESIAN_POINT('Ctrl Pts',(373.319582844735,-24.323148206982,2.05416568487398));
#40308=CARTESIAN_POINT('Ctrl Pts',(373.254555340926,-24.3293104875486,2.13039329566615));
#40309=CARTESIAN_POINT('Ctrl Pts',(373.186159521633,-24.3354727681152,2.20339699764539));
#40310=CARTESIAN_POINT('Ctrl Pts',(373.11769382624,-24.3416413443317,2.27647528333577));
#40311=CARTESIAN_POINT('Ctrl Pts',(373.045853240098,-24.3478099205483,2.34632276702677));
#40312=CARTESIAN_POINT('Ctrl Pts',(372.970984357664,-24.3539784967648,2.41262798858518));
#40313=CARTESIAN_POINT('Ctrl Pts',(372.896074773403,-24.360150426475,2.47896925640998));
#40314=CARTESIAN_POINT('Ctrl Pts',(372.818133950538,-24.3663223561853,2.54176415499762));
#40315=CARTESIAN_POINT('Ctrl Pts',(372.737540397211,-24.3724942858955,2.60074249216659));
#40316=CARTESIAN_POINT('Ctrl Pts',(372.656818848318,-24.3786760176259,2.65981449645049));
#40317=CARTESIAN_POINT('Ctrl Pts',(372.573436514892,-24.3848577493563,2.7150575937841));
#40318=CARTESIAN_POINT('Ctrl Pts',(372.487799670703,-24.3910394810866,2.76624573054627));
#40319=CARTESIAN_POINT('Ctrl Pts',(372.429473975143,-24.3952497460299,2.80110903861588));
#40320=CARTESIAN_POINT('Ctrl Pts',(372.370103013157,-24.3994600109731,2.83409231253986));
#40321=CARTESIAN_POINT('Ctrl Pts',(372.309820613641,-24.4036702759164,2.86513684952406));
#40322=CARTESIAN_POINT('Ctrl Pts',(367.611569202942,-23.5610139381901,-0.0029495098797409));
#40323=CARTESIAN_POINT('Ctrl Pts',(367.611380133205,-23.5494540715678,0.203635402400345));
#40324=CARTESIAN_POINT('Ctrl Pts',(367.631054003286,-23.5377943915509,0.409741458807204));
#40325=CARTESIAN_POINT('Ctrl Pts',(367.675072507174,-23.5239887098281,0.63711280560356));
#40326=CARTESIAN_POINT('Ctrl Pts',(367.680115170967,-23.5224883651973,0.66162623187756));
#40327=CARTESIAN_POINT('Ctrl Pts',(367.688962196206,-23.5199820626771,0.702231206944551));
#40328=CARTESIAN_POINT('Ctrl Pts',(367.692605866632,-23.5189811692298,0.718356913272546));
#40329=CARTESIAN_POINT('Ctrl Pts',(367.699991077294,-23.5170114587375,0.749910137940433));
#40330=CARTESIAN_POINT('Ctrl Pts',(367.703722856242,-23.516042977234,0.765339469820808));
#40331=CARTESIAN_POINT('Ctrl Pts',(367.710951352093,-23.5142156201992,0.794288523311939));
#40332=CARTESIAN_POINT('Ctrl Pts',(367.714422259156,-23.5133575956715,0.807814354310493));
#40333=CARTESIAN_POINT('Ctrl Pts',(367.722425264666,-23.5114215825672,0.838180291735856));
#40334=CARTESIAN_POINT('Ctrl Pts',(367.727006342797,-23.5103420288793,0.855006925232355));
#40335=CARTESIAN_POINT('Ctrl Pts',(367.739073921332,-23.507569007301,0.897953703212452));
#40336=CARTESIAN_POINT('Ctrl Pts',(367.746754487406,-23.5058692900971,0.924017445948775));
#40337=CARTESIAN_POINT('Ctrl Pts',(367.80321028937,-23.4938126983858,1.10703040359618));
#40338=CARTESIAN_POINT('Ctrl Pts',(367.863592127225,-23.4830748265927,1.26012048479625));
#40339=CARTESIAN_POINT('Ctrl Pts',(367.994739098085,-23.4630061701277,1.53015545340408));
#40340=CARTESIAN_POINT('Ctrl Pts',(368.06177485662,-23.4537776085564,1.6485103184398));
#40341=CARTESIAN_POINT('Ctrl Pts',(368.217519064277,-23.4345500723545,1.88697208611006));
#40342=CARTESIAN_POINT('Ctrl Pts',(368.307516678658,-23.4245847290635,2.00588765010823));
#40343=CARTESIAN_POINT('Ctrl Pts',(368.418109840132,-23.4138573885052,2.13270456257474));
#40344=CARTESIAN_POINT('Ctrl Pts',(368.43092318024,-23.4126353810892,2.1471339040296));
#40345=CARTESIAN_POINT('Ctrl Pts',(368.450499814581,-23.4108007664504,2.16878467438934));
#40346=CARTESIAN_POINT('Ctrl Pts',(368.457167767995,-23.4101814558805,2.17609119377525));
#40347=CARTESIAN_POINT('Ctrl Pts',(368.468662404547,-23.4091235420553,2.1885707465838));
#40348=CARTESIAN_POINT('Ctrl Pts',(368.473472583463,-23.4086837190848,2.19375869917104));
#40349=CARTESIAN_POINT('Ctrl Pts',(368.484454792367,-23.4076861133738,2.20552545384239));
#40350=CARTESIAN_POINT('Ctrl Pts',(368.490637378892,-23.4071291485305,2.21209420486772));
#40351=CARTESIAN_POINT('Ctrl Pts',(368.507573736009,-23.4056157594886,2.22993769692907));
#40352=CARTESIAN_POINT('Ctrl Pts',(368.51838197718,-23.4046634020596,2.24116071704021));
#40353=CARTESIAN_POINT('Ctrl Pts',(368.573339388843,-23.3998854571837,2.29740504253139));
#40354=CARTESIAN_POINT('Ctrl Pts',(368.618724775936,-23.3961476035813,2.34120525214784));
#40355=CARTESIAN_POINT('Ctrl Pts',(368.818820475119,-23.3803814053289,2.52327792289411));
#40356=CARTESIAN_POINT('Ctrl Pts',(368.985407988201,-23.3689802148214,2.64777410432298));
#40357=CARTESIAN_POINT('Ctrl Pts',(369.269128081034,-23.3503442157055,2.81988629963155));
#40358=CARTESIAN_POINT('Ctrl Pts',(369.379072471157,-23.3432929817804,2.8781652479805));
#40359=CARTESIAN_POINT('Ctrl Pts',(369.558878684482,-23.3317650861883,2.9605349853177));
#40360=CARTESIAN_POINT('Ctrl Pts',(369.626677412875,-23.3274203636305,2.98883184898583));
#40361=CARTESIAN_POINT('Ctrl Pts',(369.716631397185,-23.321629636725,3.02281501693162));
#40362=CARTESIAN_POINT('Ctrl Pts',(369.737966668181,-23.3202543651,3.03061836581827));
#40363=CARTESIAN_POINT('Ctrl Pts',(369.773688825696,-23.3179478787091,3.04325712489756));
#40364=CARTESIAN_POINT('Ctrl Pts',(369.788030784401,-23.3170208351351,3.04821771196498));
#40365=CARTESIAN_POINT('Ctrl Pts',(369.815804401445,-23.3152233857138,3.05760492940643));
#40366=CARTESIAN_POINT('Ctrl Pts',(369.829231235774,-23.314353441857,3.06204481304255));
#40367=CARTESIAN_POINT('Ctrl Pts',(369.860274585425,-23.3123396275133,3.07208381377094));
#40368=CARTESIAN_POINT('Ctrl Pts',(369.877910788305,-23.3111937212452,3.07761998137172));
#40369=CARTESIAN_POINT('Ctrl Pts',(369.935081857265,-23.3074726460979,3.09502764046936));
#40370=CARTESIAN_POINT('Ctrl Pts',(369.97479616449,-23.3048778588671,3.10629098515518));
#40371=CARTESIAN_POINT('Ctrl Pts',(370.239521699351,-23.2875090406947,3.17590430315866));
#40372=CARTESIAN_POINT('Ctrl Pts',(370.470026884013,-23.2719661716621,3.21051502441555));
#40373=CARTESIAN_POINT('Ctrl Pts',(370.843961392244,-23.2466524399666,3.22585701486366));
#40374=CARTESIAN_POINT('Ctrl Pts',(370.985954778114,-23.2370366717919,3.22230611145));
#40375=CARTESIAN_POINT('Ctrl Pts',(371.170232003222,-23.2248548909977,3.20548614410348));
#40376=CARTESIAN_POINT('Ctrl Pts',(371.213125284679,-23.2220412807141,3.20070070850935));
#40377=CARTESIAN_POINT('Ctrl Pts',(371.28479040941,-23.2173906603054,3.19124435789764));
#40378=CARTESIAN_POINT('Ctrl Pts',(371.313617538054,-23.215533687009,3.18704220651699));
#40379=CARTESIAN_POINT('Ctrl Pts',(371.353706562784,-23.212974075198,3.1806421330473));
#40380=CARTESIAN_POINT('Ctrl Pts',(371.365018730542,-23.212254356973,3.17877422889665));
#40381=CARTESIAN_POINT('Ctrl Pts',(371.384249077559,-23.2110354670183,3.17549333124718));
#40382=CARTESIAN_POINT('Ctrl Pts',(371.392172320108,-23.2105345989786,3.17411100112082));
#40383=CARTESIAN_POINT('Ctrl Pts',(371.407443141196,-23.2095719308206,3.17138782671641));
#40384=CARTESIAN_POINT('Ctrl Pts',(371.414791302006,-23.2091098916934,3.17005109124221));
#40385=CARTESIAN_POINT('Ctrl Pts',(371.43461298449,-23.2078665838393,3.16637401143913));
#40386=CARTESIAN_POINT('Ctrl Pts',(371.447077589814,-23.2070880039969,3.16398548393497));
#40387=CARTESIAN_POINT('Ctrl Pts',(371.493643353979,-23.2041904546128,3.15477682561962));
#40388=CARTESIAN_POINT('Ctrl Pts',(371.527648852348,-23.2020967710002,3.14747824194551));
#40389=CARTESIAN_POINT('Ctrl Pts',(371.821610133719,-23.1841397458632,3.07938980133958));
#40390=CARTESIAN_POINT('Ctrl Pts',(372.072938453568,-23.1696816819013,2.98712763432748));
#40391=CARTESIAN_POINT('Ctrl Pts',(372.309820652881,-23.1546465340816,2.86513682931627));
#40392=CARTESIAN_POINT('',(367.61156800787,-23.3142265506821,0.000998384406030673));
#40393=CARTESIAN_POINT('Ctrl Pts',(372.309820613641,-22.9071794904733,2.86513684952399));
#40394=CARTESIAN_POINT('Ctrl Pts',(372.220989734859,-22.9133311557454,2.91088342769398));
#40395=CARTESIAN_POINT('Ctrl Pts',(372.129996352699,-22.9194828210175,2.95251196963913));
#40396=CARTESIAN_POINT('Ctrl Pts',(372.037260366095,-22.9256344862896,2.98982388665753));
#40397=CARTESIAN_POINT('Ctrl Pts',(371.944529271348,-22.9317858270591,3.02713383545884));
#40398=CARTESIAN_POINT('Ctrl Pts',(371.85005615787,-22.9379371678286,3.06012745032107));
#40399=CARTESIAN_POINT('Ctrl Pts',(371.75428056199,-22.9440885085982,3.08865442822273));
#40400=CARTESIAN_POINT('Ctrl Pts',(371.658484431469,-22.9502411682378,3.11718752241366));
#40401=CARTESIAN_POINT('Ctrl Pts',(371.561385679857,-22.9563938278775,3.14125195325109));
#40402=CARTESIAN_POINT('Ctrl Pts',(371.46343766846,-22.9625464875172,3.16074766796994));
#40403=CARTESIAN_POINT('Ctrl Pts',(371.365382213966,-22.9687058962556,3.18026476831898));
#40404=CARTESIAN_POINT('Ctrl Pts',(371.266476066421,-22.9748653049941,3.19520306302124));
#40405=CARTESIAN_POINT('Ctrl Pts',(371.167181258783,-22.9810247137325,3.20551392380996));
#40406=CARTESIAN_POINT('Ctrl Pts',(371.067825889607,-22.9871878791957,3.21583107336247));
#40407=CARTESIAN_POINT('Ctrl Pts',(370.96808182146,-22.993351044659,3.22151514481994));
#40408=CARTESIAN_POINT('Ctrl Pts',(370.868412603373,-22.9995142101222,3.2225696440127));
#40409=CARTESIAN_POINT('Ctrl Pts',(370.76858417089,-23.0056872207983,3.22362582769196));
#40410=CARTESIAN_POINT('Ctrl Pts',(370.668831260545,-23.0118602314744,3.22003768913998));
#40411=CARTESIAN_POINT('Ctrl Pts',(370.569613789268,-23.0180332421505,3.21186072565816));
#40412=CARTESIAN_POINT('Ctrl Pts',(370.51691446294,-23.0213120346843,3.20751753426901));
#40413=CARTESIAN_POINT('Ctrl Pts',(370.46436605609,-23.0245908272182,3.2018806167265));
#40414=CARTESIAN_POINT('Ctrl Pts',(370.412036183166,-23.027869619752,3.19496412399772));
#40415=CARTESIAN_POINT('Ctrl Pts',(370.313505351796,-23.0340431901468,3.18194120342392));
#40416=CARTESIAN_POINT('Ctrl Pts',(370.215405000158,-23.0402167605415,3.16433326267595));
#40417=CARTESIAN_POINT('Ctrl Pts',(370.11819531248,-23.0463903309363,3.14217855462378));
#40418=CARTESIAN_POINT('Ctrl Pts',(370.021116839483,-23.0525555681794,3.12005375123481));
#40419=CARTESIAN_POINT('Ctrl Pts',(369.924927060452,-23.0587208054224,3.09339447487113));
#40420=CARTESIAN_POINT('Ctrl Pts',(369.830079930798,-23.0648860426655,3.06229060633737));
#40421=CARTESIAN_POINT('Ctrl Pts',(369.735332839819,-23.0710447772114,3.0312195441709));
#40422=CARTESIAN_POINT('Ctrl Pts',(369.641925993033,-23.0772035117573,2.99571334445778));
#40423=CARTESIAN_POINT('Ctrl Pts',(369.550301111884,-23.0833622463032,2.95591247679277));
#40424=CARTESIAN_POINT('Ctrl Pts',(369.458742764106,-23.0895165086865,2.91614051051173));
#40425=CARTESIAN_POINT('Ctrl Pts',(369.368964206311,-23.0956707710697,2.87208024906491));
#40426=CARTESIAN_POINT('Ctrl Pts',(369.281389129887,-23.101825033453,2.82392102275079));
#40427=CARTESIAN_POINT('Ctrl Pts',(369.193846973397,-23.1079769824166,2.77577989974461));
#40428=CARTESIAN_POINT('Ctrl Pts',(369.108507032422,-23.1141289313801,2.72354308251434));
#40429=CARTESIAN_POINT('Ctrl Pts',(369.025769440113,-23.1202808803436,2.66744638182932));
#40430=CARTESIAN_POINT('Ctrl Pts',(368.943040845521,-23.1264321602824,2.61135578166257));
#40431=CARTESIAN_POINT('Ctrl Pts',(368.862914396256,-23.1325834402213,2.55140637626594));
#40432=CARTESIAN_POINT('Ctrl Pts',(368.785761359651,-23.1387347201601,2.48787737944211));
#40433=CARTESIAN_POINT('Ctrl Pts',(368.708596101796,-23.1448869744783,2.42433831945346));
#40434=CARTESIAN_POINT('Ctrl Pts',(368.634405527312,-23.1510392287965,2.35721881777673));
#40435=CARTESIAN_POINT('Ctrl Pts',(368.56352714042,-23.1571914831147,2.2868377951104));
#40436=CARTESIAN_POINT('Ctrl Pts',(368.492573153698,-23.1633502995092,2.21638170310869));
#40437=CARTESIAN_POINT('Ctrl Pts',(368.424938717774,-23.1695091159038,2.14265744997855));
#40438=CARTESIAN_POINT('Ctrl Pts',(368.360923722094,-23.1756679322983,2.06602009539862));
#40439=CARTESIAN_POINT('Ctrl Pts',(368.296872897655,-23.1818301957406,1.98933984741162));
#40440=CARTESIAN_POINT('Ctrl Pts',(368.236445810301,-23.1879924591828,1.90974359673948));
#40441=CARTESIAN_POINT('Ctrl Pts',(368.179900095961,-23.1941547226251,1.82761700922941));
#40442=CARTESIAN_POINT('Ctrl Pts',(368.123260537344,-23.2003272130696,1.74535412297017));
#40443=CARTESIAN_POINT('Ctrl Pts',(368.070515447642,-23.2064997035142,1.66055288074536));
#40444=CARTESIAN_POINT('Ctrl Pts',(368.021877492127,-23.2126721939587,1.57362536131473));
#40445=CARTESIAN_POINT('Ctrl Pts',(367.985857525235,-23.2172433750271,1.5092491691267));
#40446=CARTESIAN_POINT('Ctrl Pts',(367.952089158342,-23.2218145560954,1.44370736284903));
#40447=CARTESIAN_POINT('Ctrl Pts',(367.920641598016,-23.2263857371637,1.3771740058318));
#40448=CARTESIAN_POINT('Ctrl Pts',(367.874660085628,-23.2330695567271,1.27989128029524));
#40449=CARTESIAN_POINT('Ctrl Pts',(367.833500582128,-23.2397533762904,1.18018949652149));
#40450=CARTESIAN_POINT('Ctrl Pts',(367.797403084392,-23.2464371958538,1.07854821373587));
#40451=CARTESIAN_POINT('Ctrl Pts',(367.761433795259,-23.253097276288,0.97726793344535));
#40452=CARTESIAN_POINT('Ctrl Pts',(367.730490777906,-23.2597573567222,0.874062186934083));
#40453=CARTESIAN_POINT('Ctrl Pts',(367.704765965764,-23.2664174371564,0.769430013840498));
#40454=CARTESIAN_POINT('Ctrl Pts',(367.679099449172,-23.2730624250395,0.665034949959054));
#40455=CARTESIAN_POINT('Ctrl Pts',(367.658627659573,-23.2797074129225,0.55922020650824));
#40456=CARTESIAN_POINT('Ctrl Pts',(367.643493542549,-23.2863524008056,0.452501691604395));
#40457=CARTESIAN_POINT('Ctrl Pts',(367.628409460502,-23.2929754196625,0.34613599929171));
#40458=CARTESIAN_POINT('Ctrl Pts',(367.618627926109,-23.2995984385194,0.238872805855995));
#40459=CARTESIAN_POINT('Ctrl Pts',(367.61424114798,-23.3062214573763,0.131238617972967));
#40460=CARTESIAN_POINT('Ctrl Pts',(367.612473748099,-23.3088898218116,0.0878736140116947));
#40461=CARTESIAN_POINT('Ctrl Pts',(367.611581468412,-23.3115581862468,0.0444485422163019));
#40462=CARTESIAN_POINT('Ctrl Pts',(367.61156800787,-23.3142265506821,0.000998384406030673));
#40463=CARTESIAN_POINT('Ctrl Pts',(372.309820613613,-24.1556143901908,2.86513684953878));
#40464=CARTESIAN_POINT('Ctrl Pts',(372.442467835282,-24.1456807417415,2.79682550805366));
#40465=CARTESIAN_POINT('Ctrl Pts',(372.570225783518,-24.1359684629225,2.71937755021739));
#40466=CARTESIAN_POINT('Ctrl Pts',(372.71400207142,-24.1248961996909,2.61794165651371));
#40467=CARTESIAN_POINT('Ctrl Pts',(372.735639693992,-24.1232254189926,2.60226951022979));
#40468=CARTESIAN_POINT('Ctrl Pts',(372.770977497378,-24.1204887407584,2.57599822448064));
#40469=CARTESIAN_POINT('Ctrl Pts',(372.784791237552,-24.1194168924612,2.5655547208309));
#40470=CARTESIAN_POINT('Ctrl Pts',(372.809601410106,-24.117487797431,2.54648145323391));
#40471=CARTESIAN_POINT('Ctrl Pts',(372.820627069685,-24.1166290541856,2.53789058631565));
#40472=CARTESIAN_POINT('Ctrl Pts',(372.844161623111,-24.1147927314224,2.51930583980846));
#40473=CARTESIAN_POINT('Ctrl Pts',(372.856652674699,-24.1138160601309,2.50928989519937));
#40474=CARTESIAN_POINT('Ctrl Pts',(372.890624974238,-24.1111537696733,2.48163076886942));
#40475=CARTESIAN_POINT('Ctrl Pts',(372.911953723628,-24.1094756626206,2.46380184110973));
#40476=CARTESIAN_POINT('Ctrl Pts',(373.032637829351,-24.0999367694206,2.36023897619377));
#40477=CARTESIAN_POINT('Ctrl Pts',(373.126919786398,-24.0923196815813,2.26877080163027));
#40478=CARTESIAN_POINT('Ctrl Pts',(373.312543629323,-24.0766404502101,2.06526205475736));
#40479=CARTESIAN_POINT('Ctrl Pts',(373.402459820053,-24.0686272142593,1.95232133653624));
#40480=CARTESIAN_POINT('Ctrl Pts',(373.579077853419,-24.051241220845,1.6970658514811));
#40481=CARTESIAN_POINT('Ctrl Pts',(373.66292007332,-24.0418725320143,1.5532984449698));
#40482=CARTESIAN_POINT('Ctrl Pts',(373.747049322534,-24.0302942232591,1.37943514783926));
#40483=CARTESIAN_POINT('Ctrl Pts',(373.758498583684,-24.0286610656654,1.35499553021274));
#40484=CARTESIAN_POINT('Ctrl Pts',(373.773906126548,-24.0263778251464,1.32100158323732));
#40485=CARTESIAN_POINT('Ctrl Pts',(373.778127734967,-24.0257429094197,1.31156691517234));
#40486=CARTESIAN_POINT('Ctrl Pts',(373.785298629911,-24.0246479901468,1.29533198794876));
#40487=CARTESIAN_POINT('Ctrl Pts',(373.788270006115,-24.0241893149638,1.28854149300396));
#40488=CARTESIAN_POINT('Ctrl Pts',(373.794438023941,-24.0232265726319,1.2743122425177));
#40489=CARTESIAN_POINT('Ctrl Pts',(373.797630078186,-24.0227222222388,1.26687164650172));
#40490=CARTESIAN_POINT('Ctrl Pts',(373.805382162072,-24.0214823997838,1.24861214142649));
#40491=CARTESIAN_POINT('Ctrl Pts',(373.809911147423,-24.0207450925936,1.23778024888221));
#40492=CARTESIAN_POINT('Ctrl Pts',(373.82616188849,-24.0180523914571,1.1983089949849));
#40493=CARTESIAN_POINT('Ctrl Pts',(373.837529756581,-24.0160775364631,1.16952694618834));
#40494=CARTESIAN_POINT('Ctrl Pts',(373.865048833878,-24.0110672133875,1.09680387408566));
#40495=CARTESIAN_POINT('Ctrl Pts',(373.880659988586,-24.0080078539166,1.05266716711442));
#40496=CARTESIAN_POINT('Ctrl Pts',(374.000151315765,-23.9827952290267,0.689883826976194));
#40497=CARTESIAN_POINT('Ctrl Pts',(374.054718573656,-23.9595432569405,0.35712651679104));
#40498=CARTESIAN_POINT('Ctrl Pts',(374.05743309452,-23.9337913500727,-0.0428874854631862));
#40499=CARTESIAN_POINT('Ctrl Pts',(374.055920631198,-23.9296795236787,-0.107646196950578));
#40500=CARTESIAN_POINT('Ctrl Pts',(374.051230006456,-23.9241917417428,-0.195245715194762));
#40501=CARTESIAN_POINT('Ctrl Pts',(374.049757396586,-23.9227631724972,-0.218158836000152));
#40502=CARTESIAN_POINT('Ctrl Pts',(374.046922111944,-23.9204173294058,-0.255958618483742));
#40503=CARTESIAN_POINT('Ctrl Pts',(374.045700525348,-23.9194956710875,-0.270854726207899));
#40504=CARTESIAN_POINT('Ctrl Pts',(374.043112353225,-23.9177019446455,-0.299930540435097));
#40505=CARTESIAN_POINT('Ctrl Pts',(374.041755293547,-23.9168295995274,-0.314110727311317));
#40506=CARTESIAN_POINT('Ctrl Pts',(374.038324221398,-23.9147738206573,-0.347618452159981));
#40507=CARTESIAN_POINT('Ctrl Pts',(374.036169263463,-23.9135929545013,-0.366937280676859));
#40508=CARTESIAN_POINT('Ctrl Pts',(374.028374357827,-23.9096597447962,-0.43150916286562));
#40509=CARTESIAN_POINT('Ctrl Pts',(374.021948598906,-23.9069320677534,-0.476663039213774));
#40510=CARTESIAN_POINT('Ctrl Pts',(374.004265634068,-23.9004635370716,-0.584464019033404));
#40511=CARTESIAN_POINT('Ctrl Pts',(373.992106726697,-23.896750150491,-0.646944564977889));
#40512=CARTESIAN_POINT('Ctrl Pts',(373.937211133331,-23.8823588087427,-0.890348639634534));
#40513=CARTESIAN_POINT('Ctrl Pts',(373.880707345235,-23.8720535919357,-1.06779326105677));
#40514=CARTESIAN_POINT('Ctrl Pts',(373.746134394167,-23.8524512054304,-1.3908096630725));
#40515=CARTESIAN_POINT('Ctrl Pts',(373.671586221931,-23.8431975132892,-1.53717998803959));
#40516=CARTESIAN_POINT('Ctrl Pts',(373.572202271709,-23.8317503433501,-1.70024511841311));
#40517=CARTESIAN_POINT('Ctrl Pts',(373.557882142189,-23.8301187725732,-1.7230908297668));
#40518=CARTESIAN_POINT('Ctrl Pts',(373.537682871047,-23.8278376384181,-1.75443489866671));
#40519=CARTESIAN_POINT('Ctrl Pts',(373.532046530819,-23.8272032277156,-1.76308939324761));
#40520=CARTESIAN_POINT('Ctrl Pts',(373.522297322871,-23.826109207318,-1.77790291682286));
#40521=CARTESIAN_POINT('Ctrl Pts',(373.51820460441,-23.8256509253845,-1.78407519883241));
#40522=CARTESIAN_POINT('Ctrl Pts',(373.509591685067,-23.8246884292966,-1.79696774644401));
#40523=CARTESIAN_POINT('Ctrl Pts',(373.505067393653,-23.8241839290119,-1.80368512895664));
#40524=CARTESIAN_POINT('Ctrl Pts',(373.493920415644,-23.8229437308169,-1.82010156471624));
#40525=CARTESIAN_POINT('Ctrl Pts',(373.487269975296,-23.8222061971507,-1.82978155086282));
#40526=CARTESIAN_POINT('Ctrl Pts',(373.462902857343,-23.8195131249983,-1.86483678270179));
#40527=CARTESIAN_POINT('Ctrl Pts',(373.444874432871,-23.8175381322536,-1.88999193913474));
#40528=CARTESIAN_POINT('Ctrl Pts',(373.398672438488,-23.8125277723452,-1.95253541258379));
#40529=CARTESIAN_POINT('Ctrl Pts',(373.370041794885,-23.8094685289126,-1.98957599084985));
#40530=CARTESIAN_POINT('Ctrl Pts',(373.130001478492,-23.7842646622101,-2.28652524659589));
#40531=CARTESIAN_POINT('Ctrl Pts',(372.880034100536,-23.7610223940301,-2.51266487245713));
#40532=CARTESIAN_POINT('Ctrl Pts',(372.545373553593,-23.7352702109003,-2.73177844891641));
#40533=CARTESIAN_POINT('Ctrl Pts',(372.49004191261,-23.7311514395181,-2.76566518484465));
#40534=CARTESIAN_POINT('Ctrl Pts',(372.413768032092,-23.7256552974136,-2.80926733451301));
#40535=CARTESIAN_POINT('Ctrl Pts',(372.393692448891,-23.7242251688583,-2.82046037706913));
#40536=CARTESIAN_POINT('Ctrl Pts',(372.360356214305,-23.721876973729,-2.83858208254149));
#40537=CARTESIAN_POINT('Ctrl Pts',(372.347164260939,-23.7209545151969,-2.84563474070548));
#40538=CARTESIAN_POINT('Ctrl Pts',(372.321306187646,-23.7191593699215,-2.85922829586009));
#40539=CARTESIAN_POINT('Ctrl Pts',(372.30864484895,-23.7182864050242,-2.8657774991294));
#40540=CARTESIAN_POINT('Ctrl Pts',(372.278607366622,-23.7162293667329,-2.88106292777026));
#40541=CARTESIAN_POINT('Ctrl Pts',(372.261194650089,-23.7150478605854,-2.88972635806348));
#40542=CARTESIAN_POINT('Ctrl Pts',(372.202684712001,-23.7111133253847,-2.91817926264425));
#40543=CARTESIAN_POINT('Ctrl Pts',(372.161244859663,-23.7083849498742,-2.93725434720373));
#40544=CARTESIAN_POINT('Ctrl Pts',(372.061044129988,-23.7019149054048,-2.98082391284935));
#40545=CARTESIAN_POINT('Ctrl Pts',(372.001934482439,-23.6982006830013,-3.00447011650423));
#40546=CARTESIAN_POINT('Ctrl Pts',(371.767534707402,-23.6838030078993,-3.09027577786004));
#40547=CARTESIAN_POINT('Ctrl Pts',(371.587703263998,-23.673492175786,-3.13896678149078));
#40548=CARTESIAN_POINT('Ctrl Pts',(371.243614258785,-23.6539039780741,-3.20083920080511));
#40549=CARTESIAN_POINT('Ctrl Pts',(371.080605450578,-23.64467062926,-3.21748732348361));
#40550=CARTESIAN_POINT('Ctrl Pts',(370.89010909125,-23.633247361395,-3.22237982570473));
#40551=CARTESIAN_POINT('Ctrl Pts',(370.863151363411,-23.6316159203847,-3.22273376565086));
#40552=CARTESIAN_POINT('Ctrl Pts',(370.825860245988,-23.6293346263441,-3.22275546777749));
#40553=CARTESIAN_POINT('Ctrl Pts',(370.815527305335,-23.6286999045171,-3.2227117843164));
#40554=CARTESIAN_POINT('Ctrl Pts',(370.79778355667,-23.6276052191003,-3.22255143332531));
#40555=CARTESIAN_POINT('Ctrl Pts',(370.790372537335,-23.6271465824796,-3.22245889063775));
#40556=CARTESIAN_POINT('Ctrl Pts',(370.774861384072,-23.6261835678811,-3.22221168256888));
#40557=CARTESIAN_POINT('Ctrl Pts',(370.766761461282,-23.6256789045941,-3.22205203679152));
#40558=CARTESIAN_POINT('Ctrl Pts',(370.746913032961,-23.6244380336093,-3.2215859577276));
#40559=CARTESIAN_POINT('Ctrl Pts',(370.735165501581,-23.6236999866931,-3.22124579731949));
#40560=CARTESIAN_POINT('Ctrl Pts',(370.692438942622,-23.6210031222292,-3.21977466916652));
#40561=CARTESIAN_POINT('Ctrl Pts',(370.661475889779,-23.619024782242,-3.21826102669073));
#40562=CARTESIAN_POINT('Ctrl Pts',(370.583717254512,-23.614004141467,-3.21333442906917));
#40563=CARTESIAN_POINT('Ctrl Pts',(370.536966327229,-23.6109378491655,-3.20934579561924));
#40564=CARTESIAN_POINT('Ctrl Pts',(370.154452293196,-23.5855423839119,-3.16828165909862));
#40565=CARTESIAN_POINT('Ctrl Pts',(369.826308807702,-23.5621059305944,-3.07964705438672));
#40566=CARTESIAN_POINT('Ctrl Pts',(369.460755538353,-23.5363545674471,-2.91605196249271));
#40567=CARTESIAN_POINT('Ctrl Pts',(369.40439804049,-23.5323848797017,-2.88883413915596));
#40568=CARTESIAN_POINT('Ctrl Pts',(369.3287539288,-23.5270541988766,-2.84954530041571));
#40569=CARTESIAN_POINT('Ctrl Pts',(369.308752740665,-23.5256444144833,-2.83888750730262));
#40570=CARTESIAN_POINT('Ctrl Pts',(369.27710628605,-23.5234129267838,-2.82159339091499));
#40571=CARTESIAN_POINT('Ctrl Pts',(369.265387407107,-23.5225863955767,-2.81509402906771));
#40572=CARTESIAN_POINT('Ctrl Pts',(369.241649314295,-23.5209116082893,-2.80173446214553));
#40573=CARTESIAN_POINT('Ctrl Pts',(369.229633061403,-23.5200635433797,-2.79486954965636));
#40574=CARTESIAN_POINT('Ctrl Pts',(369.202033903474,-23.5181148306078,-2.77886541645274));
#40575=CARTESIAN_POINT('Ctrl Pts',(369.186482786133,-23.5170161644153,-2.76967209388485));
#40576=CARTESIAN_POINT('Ctrl Pts',(369.153920839204,-23.5147138866712,-2.75005118011403));
#40577=CARTESIAN_POINT('Ctrl Pts',(369.136927845903,-23.5135113461233,-2.73959537304416));
#40578=CARTESIAN_POINT('Ctrl Pts',(369.091800528143,-23.5103140547179,-2.71124740986724));
#40579=CARTESIAN_POINT('Ctrl Pts',(369.063844496158,-23.5083294094359,-2.6930750744508));
#40580=CARTESIAN_POINT('Ctrl Pts',(368.890462271229,-23.495983641918,-2.57650399326839));
#40581=CARTESIAN_POINT('Ctrl Pts',(368.75299306793,-23.486050932814,-2.46678813542396));
#40582=CARTESIAN_POINT('Ctrl Pts',(368.467561371951,-23.4640905314945,-2.19804938935714));
#40583=CARTESIAN_POINT('Ctrl Pts',(368.325351303357,-23.4521715428843,-2.03421299416523));
#40584=CARTESIAN_POINT('Ctrl Pts',(368.177802589493,-23.4369987957076,-1.82499733314741));
#40585=CARTESIAN_POINT('Ctrl Pts',(368.155559316862,-23.4346197714901,-1.79218888359884));
#40586=CARTESIAN_POINT('Ctrl Pts',(368.126635994491,-23.4313884781567,-1.74778574327806));
#40587=CARTESIAN_POINT('Ctrl Pts',(368.119413912504,-23.4305695885449,-1.73654617871157));
#40588=CARTESIAN_POINT('Ctrl Pts',(368.108191409367,-23.4292774861578,-1.71883972315113));
#40589=CARTESIAN_POINT('Ctrl Pts',(368.104143541894,-23.4288073452721,-1.71240287570564));
#40590=CARTESIAN_POINT('Ctrl Pts',(368.09590252233,-23.4278416395556,-1.69919465407191));
#40591=CARTESIAN_POINT('Ctrl Pts',(368.091711683448,-23.4273459212298,-1.69242204809366));
#40592=CARTESIAN_POINT('Ctrl Pts',(368.081791256619,-23.4261614934845,-1.6762565298239));
#40593=CARTESIAN_POINT('Ctrl Pts',(368.076084613433,-23.4254713180545,-1.66684972490288));
#40594=CARTESIAN_POINT('Ctrl Pts',(368.056927707008,-23.4231247347265,-1.63490380828036));
#40595=CARTESIAN_POINT('Ctrl Pts',(368.04370506277,-23.421454706823,-1.61223033024187));
#40596=CARTESIAN_POINT('Ctrl Pts',(368.012234155429,-23.417359647458,-1.55671847845611));
#40597=CARTESIAN_POINT('Ctrl Pts',(367.994280613696,-23.414919985841,-1.52371816552844));
#40598=CARTESIAN_POINT('Ctrl Pts',(367.925134837549,-23.4051203823547,-1.39115239105593));
#40599=CARTESIAN_POINT('Ctrl Pts',(367.878571310424,-23.397593111491,-1.28926725537856));
#40600=CARTESIAN_POINT('Ctrl Pts',(367.749651634282,-23.3739040249761,-0.963271993030066));
#40601=CARTESIAN_POINT('Ctrl Pts',(367.686800329966,-23.3577465822787,-0.732273755138728));
#40602=CARTESIAN_POINT('Ctrl Pts',(367.640064499905,-23.3382158920887,-0.432493266754107));
#40603=CARTESIAN_POINT('Ctrl Pts',(367.632024075438,-23.3341073263439,-0.368266801160347));
#40604=CARTESIAN_POINT('Ctrl Pts',(367.623760271491,-23.3286242171115,-0.281004642953406));
#40605=CARTESIAN_POINT('Ctrl Pts',(367.621841707968,-23.3271971591267,-0.258148513109521));
#40606=CARTESIAN_POINT('Ctrl Pts',(367.619076172366,-23.3248528204618,-0.220367577383022));
#40607=CARTESIAN_POINT('Ctrl Pts',(367.618088768468,-23.3239311734424,-0.205454184320089));
#40608=CARTESIAN_POINT('Ctrl Pts',(367.616417549739,-23.3221941933596,-0.1772361669251));
#40609=CARTESIAN_POINT('Ctrl Pts',(367.615712417976,-23.3213782110927,-0.163933165152991));
#40610=CARTESIAN_POINT('Ctrl Pts',(367.614440904176,-23.319717079721,-0.136757959450048));
#40611=CARTESIAN_POINT('Ctrl Pts',(367.61388163701,-23.3188721689367,-0.122885691443705));
#40612=CARTESIAN_POINT('Ctrl Pts',(367.61281983492,-23.3169680356372,-0.0915127688218745));
#40613=CARTESIAN_POINT('Ctrl Pts',(367.612370226851,-23.3159104699517,-0.0740106754883971));
#40614=CARTESIAN_POINT('Ctrl Pts',(367.611728139963,-23.313707335571,-0.0373953607415123));
#40615=CARTESIAN_POINT('Ctrl Pts',(367.611563030695,-23.3125626383311,-0.0182823692621725));
#40616=CARTESIAN_POINT('Ctrl Pts',(367.611567960415,-23.3114228970708,0.00083120270546652));
#40617=CARTESIAN_POINT('Origin',(370.834317853224,0.,0.));
#40618=CARTESIAN_POINT('',(366.90131859535,-0.404163522081287,0.00241610556833531));
#40619=CARTESIAN_POINT('',(372.583015783242,-7.58132545439985E-5,3.52286027959531));
#40620=CARTESIAN_POINT('Ctrl Pts',(366.901318595351,-0.404163522034968,
0.00241610647972434));
#40621=CARTESIAN_POINT('Ctrl Pts',(366.90139983104,-0.397442828341541,0.134653616887458));
#40622=CARTESIAN_POINT('Ctrl Pts',(366.908149810272,-0.390722134648114,
0.266692292879821));
#40623=CARTESIAN_POINT('Ctrl Pts',(366.921511751991,-0.384001440954687,
0.39804197537121));
#40624=CARTESIAN_POINT('Ctrl Pts',(366.933209419728,-0.378117831862511,
0.513031620996121));
#40625=CARTESIAN_POINT('Ctrl Pts',(366.94999952768,-0.372234222770335,0.627693708269049));
#40626=CARTESIAN_POINT('Ctrl Pts',(366.971856973827,-0.36635061367816,0.741542281418));
#40627=CARTESIAN_POINT('Ctrl Pts',(366.993686185506,-0.360474604768403,
0.855243790084839));
#40628=CARTESIAN_POINT('Ctrl Pts',(367.020569640122,-0.354598595858646,
0.968133473973612));
#40629=CARTESIAN_POINT('Ctrl Pts',(367.052430428212,-0.348722586948889,
1.07972982941867));
#40630=CARTESIAN_POINT('Ctrl Pts',(367.084258493025,-0.342852613114828,
1.19121156753371));
#40631=CARTESIAN_POINT('Ctrl Pts',(367.121053609894,-0.336982639280766,
1.30140222607469));
#40632=CARTESIAN_POINT('Ctrl Pts',(367.162687831609,-0.331112665446705,
1.40983048072249));
#40633=CARTESIAN_POINT('Ctrl Pts',(367.205725225613,-0.325044859534052,
1.5219130254236));
#40634=CARTESIAN_POINT('Ctrl Pts',(367.253933585446,-0.318977053621399,
1.63211183191873));
#40635=CARTESIAN_POINT('Ctrl Pts',(367.307115391484,-0.312909247708746,
1.73992292757268));
#40636=CARTESIAN_POINT('Ctrl Pts',(367.358503086155,-0.307046141868695,
1.84409696900549));
#40637=CARTESIAN_POINT('Ctrl Pts',(367.414533876438,-0.301183036028645,
1.94604140494679));
#40638=CARTESIAN_POINT('Ctrl Pts',(367.474980931379,-0.295319930188594,
2.04532257737789));
#40639=CARTESIAN_POINT('Ctrl Pts',(367.53541824693,-0.289457769027829,2.14458775336109));
#40640=CARTESIAN_POINT('Ctrl Pts',(367.600270198113,-0.283595607867065,
2.24119016769621));
#40641=CARTESIAN_POINT('Ctrl Pts',(367.669265030756,-0.2777334467063,2.33472260257821));
#40642=CARTESIAN_POINT('Ctrl Pts',(367.738265281955,-0.271870825156812,
2.42826238309215));
#40643=CARTESIAN_POINT('Ctrl Pts',(367.811408816996,-0.266008203607325,
2.51873137362716));
#40644=CARTESIAN_POINT('Ctrl Pts',(367.888382183185,-0.260145582057837,
2.60575363915912));
#40645=CARTESIAN_POINT('Ctrl Pts',(367.96538004165,-0.254281095071549,2.69280359444305));
#40646=CARTESIAN_POINT('Ctrl Pts',(368.046209881964,-0.24841660808526,2.77640433567425));
#40647=CARTESIAN_POINT('Ctrl Pts',(368.130520310688,-0.242552121098972,
2.85621565169292));
#40648=CARTESIAN_POINT('Ctrl Pts',(368.214923611673,-0.236681174079493,
2.93611488396953));
#40649=CARTESIAN_POINT('Ctrl Pts',(368.302814854683,-0.230810227060013,
3.01221607612009));
#40650=CARTESIAN_POINT('Ctrl Pts',(368.393808309786,-0.224939280040534,
3.08421824266495));
#40651=CARTESIAN_POINT('Ctrl Pts',(368.484861606446,-0.21906447201135,3.15626776120651));
#40652=CARTESIAN_POINT('Ctrl Pts',(368.57902084509,-0.213189663982166,3.2242126453513));
#40653=CARTESIAN_POINT('Ctrl Pts',(368.675871377948,-0.207314855952981,
3.28779528154807));
#40654=CARTESIAN_POINT('Ctrl Pts',(368.7728599454,-0.201431674952421,3.35146853782812));
#40655=CARTESIAN_POINT('Ctrl Pts',(368.872547109993,-0.19554849395186,3.41076692797266));
#40656=CARTESIAN_POINT('Ctrl Pts',(368.974493672812,-0.1896653129513,3.46547875739509));
#40657=CARTESIAN_POINT('Ctrl Pts',(368.998637955345,-0.188271983148544,
3.47843630918389));
#40658=CARTESIAN_POINT('Ctrl Pts',(369.02290888086,-0.186878653345788,3.4911368154074));
#40659=CARTESIAN_POINT('Ctrl Pts',(369.047300464512,-0.185485323543031,
3.50357786447521));
#40660=CARTESIAN_POINT('Ctrl Pts',(369.149105904895,-0.179669852264471,
3.55550423781901));
#40661=CARTESIAN_POINT('Ctrl Pts',(369.253360637276,-0.17385438098591,3.60308333242703));
#40662=CARTESIAN_POINT('Ctrl Pts',(369.359652963928,-0.168038909707349,
3.64607356813824));
#40663=CARTESIAN_POINT('Ctrl Pts',(369.465809271562,-0.162230880308276,
3.68900879056884));
#40664=CARTESIAN_POINT('Ctrl Pts',(369.573997602747,-0.156422850909202,
3.72736667042392));
#40665=CARTESIAN_POINT('Ctrl Pts',(369.683781476545,-0.150614821510128,
3.76095134852051));
#40666=CARTESIAN_POINT('Ctrl Pts',(369.793455633911,-0.144812596572471,
3.79450246257071));
#40667=CARTESIAN_POINT('Ctrl Pts',(369.90472176221,-0.139010371634813,3.82328973690433));
#40668=CARTESIAN_POINT('Ctrl Pts',(370.017123934124,-0.133208146697156,
3.84716559282111));
#40669=CARTESIAN_POINT('Ctrl Pts',(370.12944833016,-0.127409936567555,3.87102492801012));
#40670=CARTESIAN_POINT('Ctrl Pts',(370.242906795218,-0.121611726437954,
3.88997951496179));
#40671=CARTESIAN_POINT('Ctrl Pts',(370.357029515543,-0.115813516308353,
3.90393197209095));
#40672=CARTESIAN_POINT('Ctrl Pts',(370.471111671465,-0.110017367126275,
3.91787946988243));
#40673=CARTESIAN_POINT('Ctrl Pts',(370.585857195012,-0.104221217944197,
3.92682832001067));
#40674=CARTESIAN_POINT('Ctrl Pts',(370.700788087664,-0.0984250687621187,
3.93073260368975));
#40675=CARTESIAN_POINT('Ctrl Pts',(370.815707265729,-0.0926295103654732,
3.934636489416));
#40676=CARTESIAN_POINT('Ctrl Pts',(370.930811353533,-0.0868339519688277,
3.93349681685789));
#40677=CARTESIAN_POINT('Ctrl Pts',(371.045620097053,-0.0810383935721821,
3.92731974274477));
#40678=CARTESIAN_POINT('Ctrl Pts',(371.160446245561,-0.0752419565697322,
3.92114173218812));
#40679=CARTESIAN_POINT('Ctrl Pts',(371.274976539408,-0.0694455195672822,
3.90992482587317));
#40680=CARTESIAN_POINT('Ctrl Pts',(371.388734429562,-0.0636490825648323,
3.89372716813622));
#40681=CARTESIAN_POINT('Ctrl Pts',(371.502604957337,-0.057846906207729,
3.87751347225338));
#40682=CARTESIAN_POINT('Ctrl Pts',(371.615701135977,-0.0520447298506258,
3.8563092379738));
#40683=CARTESIAN_POINT('Ctrl Pts',(371.727555213591,-0.0462425534935225,
3.83022401669202));
#40684=CARTESIAN_POINT('Ctrl Pts',(371.839468999384,-0.0404372799102038,
3.80412487100908));
#40685=CARTESIAN_POINT('Ctrl Pts',(371.950138958083,-0.0346320063268851,
3.77313966492761));
#40686=CARTESIAN_POINT('Ctrl Pts',(372.059112930347,-0.0288267327435663,
3.73742772760287));
#40687=CARTESIAN_POINT('Ctrl Pts',(372.168252435842,-0.0230126408555866,
3.70166154326654));
#40688=CARTESIAN_POINT('Ctrl Pts',(372.275690416357,-0.0171985489676068,
3.66115443970971));
#40689=CARTESIAN_POINT('Ctrl Pts',(372.380994919605,-0.011384457079627,
3.61611380522396));
#40690=CARTESIAN_POINT('Ctrl Pts',(372.449268758601,-0.00761490913793266,
3.58691185343346));
#40691=CARTESIAN_POINT('Ctrl Pts',(372.516646252166,-0.00384536119623833,
3.55580517448111));
#40692=CARTESIAN_POINT('Ctrl Pts',(372.583015783242,-7.58132545439984E-5,
3.52286027959531));
#40693=CARTESIAN_POINT('',(369.085623377893,-2.77555756156289E-16,3.52286199445083));
#40694=CARTESIAN_POINT('Origin',(370.834317853224,0.,0.));
#40695=CARTESIAN_POINT('',(366.899343652645,-0.220836477965047,0.00293853132396546));
#40696=CARTESIAN_POINT('Ctrl Pts',(369.085623377893,-1.52655665885959E-15,
3.52286199445085));
#40697=CARTESIAN_POINT('Ctrl Pts',(367.913859775743,-0.0661720391372309,
2.94121657640649));
#40698=CARTESIAN_POINT('Ctrl Pts',(366.970282437321,-0.139784198458912,
1.59707612697616));
#40699=CARTESIAN_POINT('Ctrl Pts',(366.896697454669,-0.213396357780595,
0.149413139069871));
#40700=CARTESIAN_POINT('Ctrl Pts',(366.897788092871,-0.220836477965047,
0.00293969297354404));
#40701=CARTESIAN_POINT('',(366.901318304758,-1.47083647792631,0.00188461231299786));
#40702=CARTESIAN_POINT('Ctrl Pts',(366.901318949881,-0.220836477965047,
0.00293705622590823));
#40703=CARTESIAN_POINT('Ctrl Pts',(366.901234427765,-0.226590815698461,
-0.110246132556759));
#40704=CARTESIAN_POINT('Ctrl Pts',(366.906039797176,-0.232345153431876,
-0.223646287279866));
#40705=CARTESIAN_POINT('Ctrl Pts',(366.915764765303,-0.23809949116529,-0.336794740378594));
#40706=CARTESIAN_POINT('Ctrl Pts',(366.925477985005,-0.243846877265747,
-0.44980650241884));
#40707=CARTESIAN_POINT('Ctrl Pts',(366.940098957755,-0.249594263366204,
-0.562566741970477));
#40708=CARTESIAN_POINT('Ctrl Pts',(366.959605392163,-0.255341649466661,
-0.674605324692005));
#40709=CARTESIAN_POINT('Ctrl Pts',(366.979642603147,-0.261245423856523,
-0.789692514553013));
#40710=CARTESIAN_POINT('Ctrl Pts',(367.004834999942,-0.267149198246385,
-0.904017749906057));
#40711=CARTESIAN_POINT('Ctrl Pts',(367.035101201619,-0.273052972636247,
-1.01707513693258));
#40712=CARTESIAN_POINT('Ctrl Pts',(367.064521882916,-0.278791818449364,
-1.1269741387124));
#40713=CARTESIAN_POINT('Ctrl Pts',(367.098736520101,-0.284530664262481,
-1.23567474535294));
#40714=CARTESIAN_POINT('Ctrl Pts',(367.137618511887,-0.290269510075598,
-1.34272222732676));
#40715=CARTESIAN_POINT('Ctrl Pts',(367.176490656075,-0.29600690241781,-1.44974259750745));
#40716=CARTESIAN_POINT('Ctrl Pts',(367.220027659705,-0.301744294760022,
-1.55511027016918));
#40717=CARTESIAN_POINT('Ctrl Pts',(367.268053469544,-0.307481687102234,
-1.65838697103408));
#40718=CARTESIAN_POINT('Ctrl Pts',(367.316079741298,-0.31321913462706,-1.76166466522104));
#40719=CARTESIAN_POINT('Ctrl Pts',(367.368594722556,-0.318956582151886,
-1.86285095747377));
#40720=CARTESIAN_POINT('Ctrl Pts',(367.42537515651,-0.324694029676713,-1.96152968127402));
#40721=CARTESIAN_POINT('Ctrl Pts',(367.485032850718,-0.330722213438933,
-2.06520879605726));
#40722=CARTESIAN_POINT('Ctrl Pts',(367.549399382709,-0.336750397201152,
-2.16611907350112));
#40723=CARTESIAN_POINT('Ctrl Pts',(367.618163464101,-0.342778580963372,
-2.26381093409381));
#40724=CARTESIAN_POINT('Ctrl Pts',(367.68370180763,-0.348523981327521,-2.35692004847437));
#40725=CARTESIAN_POINT('Ctrl Pts',(367.753234155057,-0.35426938169167,-2.44710554481106));
#40726=CARTESIAN_POINT('Ctrl Pts',(367.826449722831,-0.360014782055818,
-2.53401229479408));
#40727=CARTESIAN_POINT('Ctrl Pts',(367.89971427732,-0.36576402652439,-2.62097719192105));
#40728=CARTESIAN_POINT('Ctrl Pts',(367.976666662431,-0.371513270992961,
-2.70465866445914));
#40729=CARTESIAN_POINT('Ctrl Pts',(368.056959715535,-0.377262515461532,
-2.78473890607607));
#40730=CARTESIAN_POINT('Ctrl Pts',(368.137368011638,-0.383020011704652,
-2.86493408524752));
#40731=CARTESIAN_POINT('Ctrl Pts',(368.221126219979,-0.388777507947771,
-2.9415174392729));
#40732=CARTESIAN_POINT('Ctrl Pts',(368.307854884267,-0.394535004190891,
-3.01421198101424));
#40733=CARTESIAN_POINT('Ctrl Pts',(368.320393985063,-0.39536741440171,-3.02472204932538));
#40734=CARTESIAN_POINT('Ctrl Pts',(368.332995130104,-0.39619982461253,-3.03515090546895));
#40735=CARTESIAN_POINT('Ctrl Pts',(368.345657126446,-0.39703223482335,-3.04549778968796));
#40736=CARTESIAN_POINT('Ctrl Pts',(368.43501691424,-0.402906821877936,-3.11851908531629));
#40737=CARTESIAN_POINT('Ctrl Pts',(368.527743429137,-0.408781408932522,
-3.18772681551179));
#40738=CARTESIAN_POINT('Ctrl Pts',(368.623477395761,-0.414655995987109,
-3.25279471710768));
#40739=CARTESIAN_POINT('Ctrl Pts',(368.719086275458,-0.420522907249488,
-3.31777760035463));
#40740=CARTESIAN_POINT('Ctrl Pts',(368.817694453855,-0.426389818511866,
-3.37863118196099));
#40741=CARTESIAN_POINT('Ctrl Pts',(368.91890901952,-0.432256729774245,-3.43506884934927));
#40742=CARTESIAN_POINT('Ctrl Pts',(369.020018356643,-0.438117541454837,
-3.49144784085979));
#40743=CARTESIAN_POINT('Ctrl Pts',(369.123728332576,-0.443978353135429,
-3.54341985015297));
#40744=CARTESIAN_POINT('Ctrl Pts',(369.229616995135,-0.44983916481602,-3.59074144934557));
#40745=CARTESIAN_POINT('Ctrl Pts',(369.339307084574,-0.455910380958478,
-3.63976190462764));
#40746=CARTESIAN_POINT('Ctrl Pts',(369.451334858364,-0.461981597100936,
-3.6837915195401));
#40747=CARTESIAN_POINT('Ctrl Pts',(369.565202912687,-0.468052813243394,
-3.72261148492628));
#40748=CARTESIAN_POINT('Ctrl Pts',(369.67499397438,-0.473906652320662,-3.76004151953938));
#40749=CARTESIAN_POINT('Ctrl Pts',(369.786495371136,-0.47976049139793,-3.79262842019649));
#40750=CARTESIAN_POINT('Ctrl Pts',(369.899241547008,-0.485614330475199,
-3.82022529460672));
#40751=CARTESIAN_POINT('Ctrl Pts',(370.011969085537,-0.491467201892101,
-3.8478176071557));
#40752=CARTESIAN_POINT('Ctrl Pts',(370.125940592961,-0.497320073309003,
-3.87042143549834));
#40753=CARTESIAN_POINT('Ctrl Pts',(370.24067733466,-0.503172944725905,-3.88794032036495));
#40754=CARTESIAN_POINT('Ctrl Pts',(370.355422840317,-0.509026263203728,
-3.90546054337966));
#40755=CARTESIAN_POINT('Ctrl Pts',(370.470933288102,-0.514879581681551,
-3.91789498858037));
#40756=CARTESIAN_POINT('Ctrl Pts',(370.586722485398,-0.520732900159374,
-3.92519878908458));
#40757=CARTESIAN_POINT('Ctrl Pts',(370.702548511644,-0.526588080396118,
-3.93250491270102));
#40758=CARTESIAN_POINT('Ctrl Pts',(370.818653051683,-0.532443260632862,
-3.93467712077262));
#40759=CARTESIAN_POINT('Ctrl Pts',(370.934548270486,-0.538298440869606,
-3.93172263307771));
#40760=CARTESIAN_POINT('Ctrl Pts',(371.050572154818,-0.544160121459632,
-3.92876486534478));
#40761=CARTESIAN_POINT('Ctrl Pts',(371.166385840931,-0.550021802049658,
-3.92066905220891));
#40762=CARTESIAN_POINT('Ctrl Pts',(371.281504887398,-0.555883482639684,
-3.90749443460466));
#40763=CARTESIAN_POINT('Ctrl Pts',(371.39670000685,-0.561749036746287,-3.89431111094779));
#40764=CARTESIAN_POINT('Ctrl Pts',(371.511199165663,-0.56761459085289,-3.87604236462034));
#40765=CARTESIAN_POINT('Ctrl Pts',(371.624528107544,-0.573480144959494,
-3.85279856130163));
#40766=CARTESIAN_POINT('Ctrl Pts',(371.738020524004,-0.57935416000267,-3.82952122929286));
#40767=CARTESIAN_POINT('Ctrl Pts',(371.850338955568,-0.585228175045846,
-3.80125461822108));
#40768=CARTESIAN_POINT('Ctrl Pts',(371.961024224051,-0.591102190089022,
-3.76815893427253));
#40769=CARTESIAN_POINT('Ctrl Pts',(371.988950872021,-0.592584244137683,
-3.75980866754208));
#40770=CARTESIAN_POINT('Ctrl Pts',(372.016773656166,-0.594066298186344,
-3.7511512266878));
#40771=CARTESIAN_POINT('Ctrl Pts',(372.044485418052,-0.595548352235006,
-3.74218966182081));
#40772=CARTESIAN_POINT('Ctrl Pts',(372.154481444827,-0.601431054947578,
-3.70661860960474));
#40773=CARTESIAN_POINT('Ctrl Pts',(372.263084729786,-0.607313757660151,
-3.66613649502488));
#40774=CARTESIAN_POINT('Ctrl Pts',(372.36982554564,-0.613196460372723,-3.6208707691011));
#40775=CARTESIAN_POINT('Ctrl Pts',(372.476431606303,-0.619071736453563,
-3.57566218899838));
#40776=CARTESIAN_POINT('Ctrl Pts',(372.581179498504,-0.624947012534402,
-3.52568216769427));
#40777=CARTESIAN_POINT('Ctrl Pts',(372.683614836949,-0.630822288615242,
-3.47110784418825));
#40778=CARTESIAN_POINT('Ctrl Pts',(372.785947967316,-0.636691702454758,
-3.41658797392835));
#40779=CARTESIAN_POINT('Ctrl Pts',(372.885972772728,-0.642561116294274,
-3.35748311290708));
#40780=CARTESIAN_POINT('Ctrl Pts',(372.983255643082,-0.648430530133791,
-3.29401812006566));
#40781=CARTESIAN_POINT('Ctrl Pts',(373.08383132835,-0.654498610946827,-3.22840497437678));
#40782=CARTESIAN_POINT('Ctrl Pts',(373.181475754103,-0.660566691759863,
-3.15813147174083));
#40783=CARTESIAN_POINT('Ctrl Pts',(373.275737999055,-0.666634772572899,
-3.08349747389725));
#40784=CARTESIAN_POINT('Ctrl Pts',(373.366814166754,-0.672497751393524,
-3.01138611576976));
#40785=CARTESIAN_POINT('Ctrl Pts',(373.454732750234,-0.678360730214148,
-2.93520454944456));
#40786=CARTESIAN_POINT('Ctrl Pts',(373.539117912785,-0.684223709034772,
-2.85526629892858));
#40787=CARTESIAN_POINT('Ctrl Pts',(373.623491786546,-0.69008590352393,-2.77533874230853));
#40788=CARTESIAN_POINT('Ctrl Pts',(373.70433288055,-0.695948098013087,-2.69165578387076));
#40789=CARTESIAN_POINT('Ctrl Pts',(373.781300729666,-0.701810292502244,
-2.60456924000078));
#40790=CARTESIAN_POINT('Ctrl Pts',(373.858276728288,-0.707673107692014,
-2.51747347523727));
#40791=CARTESIAN_POINT('Ctrl Pts',(373.93137839401,-0.713535922881785,-2.42697371697525));
#40792=CARTESIAN_POINT('Ctrl Pts',(374.000304680523,-0.719398738071556,
-2.3334558940266));
#40793=CARTESIAN_POINT('Ctrl Pts',(374.069254783761,-0.725263579092993,
-2.23990575701705));
#40794=CARTESIAN_POINT('Ctrl Pts',(374.134026394532,-0.73112842011443,-2.14333581259028));
#40795=CARTESIAN_POINT('Ctrl Pts',(374.19436142697,-0.736993261135867,-2.04416148641085));
#40796=CARTESIAN_POINT('Ctrl Pts',(374.25476533676,-0.742864797350716,-1.94487394466549));
#40797=CARTESIAN_POINT('Ctrl Pts',(374.310722345107,-0.748736333565566,
-1.84297643876841));
#40798=CARTESIAN_POINT('Ctrl Pts',(374.362019974693,-0.754607869780415,
-1.73890964175274));
#40799=CARTESIAN_POINT('Ctrl Pts',(374.413352542805,-0.760483405065387,
-1.63477196542995));
#40800=CARTESIAN_POINT('Ctrl Pts',(374.460019247498,-0.766358940350359,
-1.52846243173027));
#40801=CARTESIAN_POINT('Ctrl Pts',(374.501856133221,-0.772234475635331,
-1.42044076425583));
#40802=CARTESIAN_POINT('Ctrl Pts',(374.543754029754,-0.778118579224664,
-1.31226156857679));
#40803=CARTESIAN_POINT('Ctrl Pts',(374.580807919275,-0.784002682813997,
-1.20236564459075));
#40804=CARTESIAN_POINT('Ctrl Pts',(374.612903924456,-0.789886786403331,
-1.0912269710248));
#40805=CARTESIAN_POINT('Ctrl Pts',(374.620499923914,-0.791279347484441,
-1.06492434241461));
#40806=CARTESIAN_POINT('Ctrl Pts',(374.62781845736,-0.792671908565551,-1.03855214562892));
#40807=CARTESIAN_POINT('Ctrl Pts',(374.634858437725,-0.794064469646662,
-1.01211672526561));
#40808=CARTESIAN_POINT('Ctrl Pts',(374.664527507088,-0.799933234780828,
-0.900708130382654));
#40809=CARTESIAN_POINT('Ctrl Pts',(374.689343901236,-0.805801999914994,
-0.787805313291286));
#40810=CARTESIAN_POINT('Ctrl Pts',(374.709158397564,-0.81167076504916,-0.673869242462348));
#40811=CARTESIAN_POINT('Ctrl Pts',(374.728947086403,-0.817531886380949,
-0.560081568236297));
#40812=CARTESIAN_POINT('Ctrl Pts',(374.743746762255,-0.823393007712738,
-0.445263720451045));
#40813=CARTESIAN_POINT('Ctrl Pts',(374.753458183173,-0.829254129044527,
-0.329891003466261));
#40814=CARTESIAN_POINT('Ctrl Pts',(374.76315956181,-0.835109189571829,-0.214637589843619));
#40815=CARTESIAN_POINT('Ctrl Pts',(374.767783116298,-0.84096425009913,-0.0988308582322655));
#40816=CARTESIAN_POINT('Ctrl Pts',(374.767280916993,-0.846819310626432,
0.0170452055034932));
#40817=CARTESIAN_POINT('Ctrl Pts',(374.766759991466,-0.852892697144427,
0.137242105257054));
#40818=CARTESIAN_POINT('Ctrl Pts',(374.760723519815,-0.858966083662422,
0.257513161864049));
#40819=CARTESIAN_POINT('Ctrl Pts',(374.749177157538,-0.865039470180417,
0.377313698964833));
#40820=CARTESIAN_POINT('Ctrl Pts',(374.738058864704,-0.870887692172542,
0.492672755014569));
#40821=CARTESIAN_POINT('Ctrl Pts',(374.721832007549,-0.876735914164666,
0.607595110489041));
#40822=CARTESIAN_POINT('Ctrl Pts',(374.700554655476,-0.882584136156791,
0.721596832665063));
#40823=CARTESIAN_POINT('Ctrl Pts',(374.679280607887,-0.888431449889361,
0.835580849775604));
#40824=CARTESIAN_POINT('Ctrl Pts',(374.652957700854,-0.894278763621932,
0.948644111060452));
#40825=CARTESIAN_POINT('Ctrl Pts',(374.6216953827,-0.900126077354503,1.06031148688492));
#40826=CARTESIAN_POINT('Ctrl Pts',(374.590430323825,-0.905973903712251,
1.17198865241984));
#40827=CARTESIAN_POINT('Ctrl Pts',(374.554225104672,-0.91182173007,1.28226929059222));
#40828=CARTESIAN_POINT('Ctrl Pts',(374.513239244379,-0.917669556427749,
1.3906927761732));
#40829=CARTESIAN_POINT('Ctrl Pts',(374.472239832407,-0.923519316327171,
1.49915211119891));
#40830=CARTESIAN_POINT('Ctrl Pts',(374.426456782632,-0.929369076226593,
1.60575268567303));
#40831=CARTESIAN_POINT('Ctrl Pts',(374.376097729164,-0.935218836126015,
1.71005389107764));
#40832=CARTESIAN_POINT('Ctrl Pts',(374.32568156061,-0.941075230572934,1.8144733904487));
#40833=CARTESIAN_POINT('Ctrl Pts',(374.270679209817,-0.946931625019853,
1.91658794271533));
#40834=CARTESIAN_POINT('Ctrl Pts',(374.21134428671,-0.952788019466772,2.01598151468107));
#40835=CARTESIAN_POINT('Ctrl Pts',(374.151969390969,-0.958648359237997,
2.11544204591309));
#40836=CARTESIAN_POINT('Ctrl Pts',(374.088256338433,-0.964508699009221,
2.212177602151));
#40837=CARTESIAN_POINT('Ctrl Pts',(374.020501076916,-0.970369038780445,
2.30580256419781));
#40838=CARTESIAN_POINT('Ctrl Pts',(373.952646309136,-0.976237985123354,
2.3995650250892));
#40839=CARTESIAN_POINT('Ctrl Pts',(373.880737741167,-0.982106931466264,
2.49020745178429));
#40840=CARTESIAN_POINT('Ctrl Pts',(373.805110467789,-0.987975877809173,
2.57737855994104));
#40841=CARTESIAN_POINT('Ctrl Pts',(373.785331698605,-0.989510780892221,
2.60017638340796));
#40842=CARTESIAN_POINT('Ctrl Pts',(373.765298765781,-0.991045683975268,
2.62273698068117));
#40843=CARTESIAN_POINT('Ctrl Pts',(373.7450180497,-0.992580587058316,2.6450545110137));
#40844=CARTESIAN_POINT('Ctrl Pts',(373.667402471763,-0.998454757841746,
2.73046510539298));
#40845=CARTESIAN_POINT('Ctrl Pts',(373.585895108387,-1.00432892862518,2.81259870524487));
#40846=CARTESIAN_POINT('Ctrl Pts',(373.500803564184,-1.0102030994086,2.89107989395727));
#40847=CARTESIAN_POINT('Ctrl Pts',(373.415821930156,-1.0160696827033,2.96945971089188));
#40848=CARTESIAN_POINT('Ctrl Pts',(373.327265622912,-1.02193626599799,3.04419622120281));
#40849=CARTESIAN_POINT('Ctrl Pts',(373.23548132504,-1.02780284929268,3.11494831122668));
#40850=CARTESIAN_POINT('Ctrl Pts',(373.143791077077,-1.0336634211929,3.1856279027106));
#40851=CARTESIAN_POINT('Ctrl Pts',(373.048879742946,-1.03952399309311,3.25233094422102));
#40852=CARTESIAN_POINT('Ctrl Pts',(372.951129053949,-1.04538456499333,3.31475479341772));
#40853=CARTESIAN_POINT('Ctrl Pts',(372.849862898589,-1.05145590413819,3.37942362875561));
#40854=CARTESIAN_POINT('Ctrl Pts',(372.745549649257,-1.05752724328305,3.43949938190571));
#40855=CARTESIAN_POINT('Ctrl Pts',(372.638649337469,-1.06359858242791,3.49469267532374));
#40856=CARTESIAN_POINT('Ctrl Pts',(372.535578934053,-1.06945240422199,3.5479085633163));
#40857=CARTESIAN_POINT('Ctrl Pts',(372.430104058848,-1.07530622601607,3.59658563003629));
#40858=CARTESIAN_POINT('Ctrl Pts',(372.322663715453,-1.08116004781016,3.64051034806745));
#40859=CARTESIAN_POINT('Ctrl Pts',(372.215239617031,-1.08701298450677,3.68442842468413));
#40860=CARTESIAN_POINT('Ctrl Pts',(372.10585102357,-1.09286592120338,3.72359542510701));
#40861=CARTESIAN_POINT('Ctrl Pts',(371.994957353933,-1.0987188579,3.75784578573875));
#40862=CARTESIAN_POINT('Ctrl Pts',(371.884053645702,-1.10457232443071,3.79209924686686));
#40863=CARTESIAN_POINT('Ctrl Pts',(371.771644985145,-1.11042579096142,3.82143506153576));
#40864=CARTESIAN_POINT('Ctrl Pts',(371.65820571613,-1.11627925749214,3.84573761317069));
#40865=CARTESIAN_POINT('Ctrl Pts',(371.544728757109,-1.12213466882724,3.87004823928745));
#40866=CARTESIAN_POINT('Ctrl Pts',(371.430220912433,-1.12799008016235,3.8893221906019));
#40867=CARTESIAN_POINT('Ctrl Pts',(371.31516576963,-1.13384549149745,3.90349513657796));
#40868=CARTESIAN_POINT('Ctrl Pts',(371.199980493832,-1.13970752558923,3.91768411284928));
#40869=CARTESIAN_POINT('Ctrl Pts',(371.084247094577,-1.145569559681,3.92676051768643));
#40870=CARTESIAN_POINT('Ctrl Pts',(370.968453420699,-1.15143159377278,3.93071197743338));
#40871=CARTESIAN_POINT('Ctrl Pts',(370.852581812872,-1.15729757325678,3.93466609667673));
#40872=CARTESIAN_POINT('Ctrl Pts',(370.736650261674,-1.16316355274079,3.93348840664086));
#40873=CARTESIAN_POINT('Ctrl Pts',(370.621144014598,-1.16902953222479,3.92721859775153));
#40874=CARTESIAN_POINT('Ctrl Pts',(370.50546915118,-1.17490407488202,3.92093963617768));
#40875=CARTESIAN_POINT('Ctrl Pts',(370.390221240461,-1.18077861753925,3.90955376079433));
#40876=CARTESIAN_POINT('Ctrl Pts',(370.275877907201,-1.18665316019649,3.89315217101589));
#40877=CARTESIAN_POINT('Ctrl Pts',(370.247047880572,-1.18813434162098,3.88901674609357));
#40878=CARTESIAN_POINT('Ctrl Pts',(370.218275294763,-1.18961552304547,3.88456271075643));
#40879=CARTESIAN_POINT('Ctrl Pts',(370.189567661076,-1.19109670446997,3.87979202918465));
#40880=CARTESIAN_POINT('Ctrl Pts',(370.075708923278,-1.1969712899297,3.86087079770612));
#40881=CARTESIAN_POINT('Ctrl Pts',(369.962494838753,-1.20284587538942,3.8369018660354));
#40882=CARTESIAN_POINT('Ctrl Pts',(369.850407688153,-1.20872046084915,3.80794036023027));
#40883=CARTESIAN_POINT('Ctrl Pts',(369.738464919095,-1.21458747914623,3.77901616027875));
#40884=CARTESIAN_POINT('Ctrl Pts',(369.627646593364,-1.2204544974433,3.74511227789214));
#40885=CARTESIAN_POINT('Ctrl Pts',(369.518427331906,-1.22632151574038,3.70633527030471));
#40886=CARTESIAN_POINT('Ctrl Pts',(369.409319610662,-1.23218254234268,3.66759786375174));
#40887=CARTESIAN_POINT('Ctrl Pts',(369.301808092295,-1.23804356894498,3.62399736847882));
#40888=CARTESIAN_POINT('Ctrl Pts',(369.196354052403,-1.24390459554727,3.57569064478454));
#40889=CARTESIAN_POINT('Ctrl Pts',(369.087118914978,-1.24997577164454,3.52565186384557));
#40890=CARTESIAN_POINT('Ctrl Pts',(368.980092005545,-1.2560469477418,3.47056314614565));
#40891=CARTESIAN_POINT('Ctrl Pts',(368.875765726678,-1.26211812383907,3.41065427265807));
#40892=CARTESIAN_POINT('Ctrl Pts',(368.775165822266,-1.26797244685032,3.35288525212275));
#40893=CARTESIAN_POINT('Ctrl Pts',(368.677077312013,-1.27382676986157,3.29063474660381));
#40894=CARTESIAN_POINT('Ctrl Pts',(368.581917608772,-1.27968109287282,3.22415603511867));
#40895=CARTESIAN_POINT('Ctrl Pts',(368.486772025745,-1.28553454719394,3.15768718803637));
#40896=CARTESIAN_POINT('Ctrl Pts',(368.394554724071,-1.29138800151506,3.08699161896017));
#40897=CARTESIAN_POINT('Ctrl Pts',(368.305653866951,-1.29724145583618,3.0123657554363));
#40898=CARTESIAN_POINT('Ctrl Pts',(368.216744721041,-1.30309545591186,2.93773293407125));
#40899=CARTESIAN_POINT('Ctrl Pts',(368.131152950724,-1.30894945598755,2.85916935532755));
#40900=CARTESIAN_POINT('Ctrl Pts',(368.04923282857,-1.31480345606323,2.77701105605485));
#40901=CARTESIAN_POINT('Ctrl Pts',(367.967285274941,-1.32065941638826,2.69482524555043));
#40902=CARTESIAN_POINT('Ctrl Pts',(367.889012105708,-1.32651537671329,2.60904261325329));
#40903=CARTESIAN_POINT('Ctrl Pts',(367.814729499569,-1.33237133703832,2.52003475660019));
#40904=CARTESIAN_POINT('Ctrl Pts',(367.740362627206,-1.33823394036761,2.43092592939101));
#40905=CARTESIAN_POINT('Ctrl Pts',(367.669995618135,-1.34409654369689,2.33858489253369));
#40906=CARTESIAN_POINT('Ctrl Pts',(367.603903294895,-1.34995914702618,2.24341498197191));
#40907=CARTESIAN_POINT('Ctrl Pts',(367.537766352001,-1.35582570826346,2.14818082115663));
#40908=CARTESIAN_POINT('Ctrl Pts',(367.475910061212,-1.36169226950075,2.05011433221244));
#40909=CARTESIAN_POINT('Ctrl Pts',(367.41856407928,-1.36755883073803,1.9496448794047));
#40910=CARTESIAN_POINT('Ctrl Pts',(367.361134255697,-1.37343396907469,1.84902853705703));
#40911=CARTESIAN_POINT('Ctrl Pts',(367.308228089329,-1.37930910741135,1.7460025853227));
#40912=CARTESIAN_POINT('Ctrl Pts',(367.260027817216,-1.38518424574801,1.64101789706739));
#40913=CARTESIAN_POINT('Ctrl Pts',(367.24791697758,-1.38666043779255,1.61463935877258));
#40914=CARTESIAN_POINT('Ctrl Pts',(367.236102986169,-1.38813662983709,1.58813724181436));
#40915=CARTESIAN_POINT('Ctrl Pts',(367.224588238786,-1.38961282188163,1.56151884735705));
#40916=CARTESIAN_POINT('Ctrl Pts',(367.171790801604,-1.39638145988535,1.4394681446803));
#40917=CARTESIAN_POINT('Ctrl Pts',(367.125132255917,-1.40315009788907,1.3146085025099));
#40918=CARTESIAN_POINT('Ctrl Pts',(367.084888280074,-1.4099187358928,1.1875465784499));
#40919=CARTESIAN_POINT('Ctrl Pts',(367.046449861813,-1.41638369700041,1.06618532425741));
#40920=CARTESIAN_POINT('Ctrl Pts',(367.013863146076,-1.42284865810803,0.942815388015679));
#40921=CARTESIAN_POINT('Ctrl Pts',(366.987321294167,-1.42931361921565,0.817989287584305));
#40922=CARTESIAN_POINT('Ctrl Pts',(366.960853551685,-1.43576052903715,0.693511723148201));
#40923=CARTESIAN_POINT('Ctrl Pts',(366.940397090558,-1.44220743885865,0.567586355194118));
#40924=CARTESIAN_POINT('Ctrl Pts',(366.926095588808,-1.44865434868014,0.440780820727839));
#40925=CARTESIAN_POINT('Ctrl Pts',(366.91185314515,-1.4550746359692,0.314498930076723));
#40926=CARTESIAN_POINT('Ctrl Pts',(366.903715033871,-1.46149492325826,0.187344380357386));
#40927=CARTESIAN_POINT('Ctrl Pts',(366.901773925552,-1.46791521054732,0.0598937136168328));
#40928=CARTESIAN_POINT('Ctrl Pts',(366.901479520429,-1.46888896634032,0.0405634532293221));
#40929=CARTESIAN_POINT('Ctrl Pts',(366.901327572947,-1.46986272213331,0.0212264068426718));
#40930=CARTESIAN_POINT('Ctrl Pts',(366.901318304758,-1.47083647792631,0.00188461231300882));
#40931=CARTESIAN_POINT('',(366.901319334106,-2.72083647799451,-0.00341300743396218));
#40932=CARTESIAN_POINT('Ctrl Pts',(366.901318304757,-1.47083647796505,0.00188461154355254));
#40933=CARTESIAN_POINT('Ctrl Pts',(366.901261719524,-1.47678156820664,-0.116203223969871));
#40934=CARTESIAN_POINT('Ctrl Pts',(366.906527842602,-1.48272665844822,-0.234278390804712));
#40935=CARTESIAN_POINT('Ctrl Pts',(366.917086804898,-1.48867174868981,-0.351837908745937));
#40936=CARTESIAN_POINT('Ctrl Pts',(366.92764953488,-1.49461896027934,-0.469439374686569));
#40937=CARTESIAN_POINT('Ctrl Pts',(366.943508829284,-1.50056617186887,-0.586524432214348));
#40938=CARTESIAN_POINT('Ctrl Pts',(366.964583027599,-1.50651338345841,-0.702596170888543));
#40939=CARTESIAN_POINT('Ctrl Pts',(366.985669182943,-1.51246396936283,-0.818733766072115));
#40940=CARTESIAN_POINT('Ctrl Pts',(367.011976063052,-1.51841455526725,-0.933856509621635));
#40941=CARTESIAN_POINT('Ctrl Pts',(367.043371192066,-1.52436514117167,-1.04747907485301));
#40942=CARTESIAN_POINT('Ctrl Pts',(367.074812871969,-1.53032455026213,-1.16127011307985));
#40943=CARTESIAN_POINT('Ctrl Pts',(367.111357763594,-1.5362839593526,-1.27355614956378));
#40944=CARTESIAN_POINT('Ctrl Pts',(367.152823750657,-1.54224336844306,-1.38386783067174));
#40945=CARTESIAN_POINT('Ctrl Pts',(367.19432364179,-1.54820765015872,-1.49426970654022));
#40946=CARTESIAN_POINT('Ctrl Pts',(367.240752491767,-1.55417193187437,-1.60269364785085));
#40947=CARTESIAN_POINT('Ctrl Pts',(367.291881092043,-1.56013621359003,-1.70869271463069));
#40948=CARTESIAN_POINT('Ctrl Pts',(367.343101685845,-1.56611122658532,-1.81488250104475));
#40949=CARTESIAN_POINT('Ctrl Pts',(367.39903873536,-1.57208623958061,-1.91863835015954));
#40950=CARTESIAN_POINT('Ctrl Pts',(367.459418063913,-1.57806125257591,-2.01953965351184));
#40951=CARTESIAN_POINT('Ctrl Pts',(367.49333041214,-1.58141714814836,-2.07621136911178));
#40952=CARTESIAN_POINT('Ctrl Pts',(367.528643336201,-1.58477304372082,-2.13198314630219));
#40953=CARTESIAN_POINT('Ctrl Pts',(367.565302654357,-1.58812893929328,-2.18678499848034));
#40954=CARTESIAN_POINT('Ctrl Pts',(367.629467027507,-1.59400272382044,-2.28270403542105));
#40955=CARTESIAN_POINT('Ctrl Pts',(367.697963489202,-1.5998765083476,-2.37595634573234));
#40956=CARTESIAN_POINT('Ctrl Pts',(367.77054320877,-1.60575029287476,-2.46612528635486));
#40957=CARTESIAN_POINT('Ctrl Pts',(367.843029224813,-1.6116164940947,-2.55617781501576));
#40958=CARTESIAN_POINT('Ctrl Pts',(367.919587758434,-1.61748269531463,-2.64315457153911));
#40959=CARTESIAN_POINT('Ctrl Pts',(367.999926268157,-1.62334889653457,-2.72666707584575));
#40960=CARTESIAN_POINT('Ctrl Pts',(368.080182514416,-1.62920909099594,-2.81009406664348));
#40961=CARTESIAN_POINT('Ctrl Pts',(368.16421075322,-1.63506928545731,-2.89006356505874));
#40962=CARTESIAN_POINT('Ctrl Pts',(368.251678103068,-1.64092947991869,-2.96621997176746));
#40963=CARTESIAN_POINT('Ctrl Pts',(368.34229906722,-1.64700096228478,-3.04512217944073));
#40964=CARTESIAN_POINT('Ctrl Pts',(368.436611531206,-1.65307244465088,-3.11993079519123));
#40965=CARTESIAN_POINT('Ctrl Pts',(368.534203108104,-1.65914392701697,-3.1902917044186));
#40966=CARTESIAN_POINT('Ctrl Pts',(368.628290220622,-1.6649973855088,-3.2581259888283));
#40967=CARTESIAN_POINT('Ctrl Pts',(368.725424630104,-1.67085084400064,-3.32182624026368));
#40968=CARTESIAN_POINT('Ctrl Pts',(368.825203662947,-1.67670430249247,-3.38111655676455));
#40969=CARTESIAN_POINT('Ctrl Pts',(368.924967708685,-1.68255688177761,-3.44039796768529));
#40970=CARTESIAN_POINT('Ctrl Pts',(369.027375232877,-1.68840946106274,-3.49527054975938));
#40971=CARTESIAN_POINT('Ctrl Pts',(369.1319962977,-1.69426204034787,-3.5455028305727));
#40972=CARTESIAN_POINT('Ctrl Pts',(369.23662694669,-1.70011515577833,-3.59573971308408));
#40973=CARTESIAN_POINT('Ctrl Pts',(369.343471166969,-1.70596827120879,-3.64133527046977));
#40974=CARTESIAN_POINT('Ctrl Pts',(369.452076895114,-1.71182138663925,-3.68210523121274));
#40975=CARTESIAN_POINT('Ctrl Pts',(369.560718834498,-1.71767645361093,-3.72288878544448));
#40976=CARTESIAN_POINT('Ctrl Pts',(369.671123063043,-1.72353152058261,-3.75884339859797));
#40977=CARTESIAN_POINT('Ctrl Pts',(369.782820814395,-1.72938658755429,-3.78983416224704));
#40978=CARTESIAN_POINT('Ctrl Pts',(369.89464513393,-1.73524828908372,-3.82086004249034));
#40979=CARTESIAN_POINT('Ctrl Pts',(370.00776550347,-1.74110999061315,-3.84691073616757));
#40980=CARTESIAN_POINT('Ctrl Pts',(370.1217012825,-1.74697169214257,-3.86790209585631));
#40981=CARTESIAN_POINT('Ctrl Pts',(370.235713875457,-1.75283734555011,-3.8889076076295));
#40982=CARTESIAN_POINT('Ctrl Pts',(370.35054256436,-1.75870299895765,-3.90484693682024));
#40983=CARTESIAN_POINT('Ctrl Pts',(370.465701608604,-1.76456865236519,-3.9156878149569));
#40984=CARTESIAN_POINT('Ctrl Pts',(370.581029008395,-1.77044288100274,-3.92654454180078));
#40985=CARTESIAN_POINT('Ctrl Pts',(370.696687316357,-1.77631710964028,-3.93228792160872));
#40986=CARTESIAN_POINT('Ctrl Pts',(370.812190739785,-1.78219133827782,-3.9329377557814));
#40987=CARTESIAN_POINT('Ctrl Pts',(370.841381507179,-1.78367591108686,-3.93310198604936));
#40988=CARTESIAN_POINT('Ctrl Pts',(370.870562409818,-1.7851604838959,-3.93294114670895));
#40989=CARTESIAN_POINT('Ctrl Pts',(370.89972567556,-1.78664505670494,-3.93245607944669));
#40990=CARTESIAN_POINT('Ctrl Pts',(371.015111361698,-1.79251883139494,-3.93053689044455));
#40991=CARTESIAN_POINT('Ctrl Pts',(371.13060461455,-1.79839260608493,-3.9235317516989));
#40992=CARTESIAN_POINT('Ctrl Pts',(371.245720432017,-1.80426638077492,-3.91142389906314));
#40993=CARTESIAN_POINT('Ctrl Pts',(371.360687659088,-1.81013257365272,-3.89933167512777));
#40994=CARTESIAN_POINT('Ctrl Pts',(371.475278012522,-1.81599876653052,-3.88214987859083));
#40995=CARTESIAN_POINT('Ctrl Pts',(371.589006460754,-1.82186495940832,-3.85991374329322));
#40996=CARTESIAN_POINT('Ctrl Pts',(371.702618484437,-1.82772514702643,-3.83770037127148));
#40997=CARTESIAN_POINT('Ctrl Pts',(371.815369954917,-1.83358533464455,-3.81044303113285));
#40998=CARTESIAN_POINT('Ctrl Pts',(371.926781602886,-1.83944552226266,-3.77822867964279));
#40999=CARTESIAN_POINT('Ctrl Pts',(372.042210365337,-1.84551700775657,-3.74485279127307));
#41000=CARTESIAN_POINT('Ctrl Pts',(372.156200414314,-1.85158849325049,-3.7061557285506));
#41001=CARTESIAN_POINT('Ctrl Pts',(372.268230626626,-1.8576599787444,-3.66229206348618));
#41002=CARTESIAN_POINT('Ctrl Pts',(372.376237778867,-1.86351343420555,-3.62000356422606));
#41003=CARTESIAN_POINT('Ctrl Pts',(372.482423013211,-1.86936688966669,-3.57291331431962));
#41004=CARTESIAN_POINT('Ctrl Pts',(372.586336197593,-1.87522034512784,-3.52121012167621));
#41005=CARTESIAN_POINT('Ctrl Pts',(372.690233799147,-1.88107292280444,-3.46951468244678));
#41006=CARTESIAN_POINT('Ctrl Pts',(372.791859658437,-1.88692550048104,-3.41320785994075));
#41007=CARTESIAN_POINT('Ctrl Pts',(372.890786198693,-1.89277807815764,-3.35252545763399));
#41008=CARTESIAN_POINT('Ctrl Pts',(372.989721825639,-1.89863119341051,-3.29183748147225));
#41009=CARTESIAN_POINT('Ctrl Pts',(373.085957288494,-1.90448430866338,-3.22677334257692));
#41010=CARTESIAN_POINT('Ctrl Pts',(373.179092680216,-1.91033742391624,-3.15761302421715));
#41011=CARTESIAN_POINT('Ctrl Pts',(373.272259147994,-1.91619249215109,-3.08842962945288));
#41012=CARTESIAN_POINT('Ctrl Pts',(373.362323156304,-1.92204756038593,-3.01514758366029));
#41013=CARTESIAN_POINT('Ctrl Pts',(373.448917224356,-1.92790262862077,-2.93808766521248));
#41014=CARTESIAN_POINT('Ctrl Pts',(373.535609446504,-1.93376433355642,-2.86094039959762));
#41015=CARTESIAN_POINT('Ctrl Pts',(373.618823569234,-1.93962603849207,-2.78000698909683));
#41016=CARTESIAN_POINT('Ctrl Pts',(373.698228330228,-1.94548774342772,-2.69564570737847));
#41017=CARTESIAN_POINT('Ctrl Pts',(373.777686641789,-1.95135340149696,-2.61122753241484));
#41018=CARTESIAN_POINT('Ctrl Pts',(373.853330207195,-1.95721905956621,-2.5233771953031));
#41019=CARTESIAN_POINT('Ctrl Pts',(373.924868594353,-1.96308471763545,-2.43248537847783));
#41020=CARTESIAN_POINT('Ctrl Pts',(373.996511588308,-1.96895895274604,-2.34146065535941));
#41021=CARTESIAN_POINT('Ctrl Pts',(374.064037183986,-1.97483318785662,-2.24738591097531));
#41022=CARTESIAN_POINT('Ctrl Pts',(374.12719867635,-1.98070742296721,-2.1506800981757));
#41023=CARTESIAN_POINT('Ctrl Pts',(374.143161354266,-1.98219200668367,-2.12623983109978));
#41024=CARTESIAN_POINT('Ctrl Pts',(374.158845522861,-1.98367659040014,-2.10163163060495));
#41025=CARTESIAN_POINT('Ctrl Pts',(374.174247676138,-1.9851611741166,-2.07686248413491));
#41026=CARTESIAN_POINT('Ctrl Pts',(374.235184917553,-1.99103479676543,-1.97886557221579));
#41027=CARTESIAN_POINT('Ctrl Pts',(374.291907025266,-1.99690841941426,-1.87802119648227));
#41028=CARTESIAN_POINT('Ctrl Pts',(374.344136978532,-2.0027820420631,-1.7747277840912));
#41029=CARTESIAN_POINT('Ctrl Pts',(374.396299489111,-2.00864808031137,-1.67156775081926));
#41030=CARTESIAN_POINT('Ctrl Pts',(374.443981195916,-2.01451411855964,-1.56596533510407));
#41031=CARTESIAN_POINT('Ctrl Pts',(374.486948754576,-2.02038015680791,-1.45834718036902));
#41032=CARTESIAN_POINT('Ctrl Pts',(374.529872308428,-2.02624018741016,-1.35083924172044));
#41033=CARTESIAN_POINT('Ctrl Pts',(374.568091165031,-2.03210021801241,-1.24132005173336));
#41034=CARTESIAN_POINT('Ctrl Pts',(374.601418565507,-2.03796024861466,-1.13023945406255));
#41035=CARTESIAN_POINT('Ctrl Pts',(374.635948890338,-2.0440317920694,-1.01514949608916));
#41036=CARTESIAN_POINT('Ctrl Pts',(374.665227779516,-2.05010333552413,-0.898383689086442));
#41037=CARTESIAN_POINT('Ctrl Pts',(374.689102584017,-2.05617487897886,-0.780463759087138));
#41038=CARTESIAN_POINT('Ctrl Pts',(374.712119175849,-2.06202817245776,-0.666782623072344));
#41039=CARTESIAN_POINT('Ctrl Pts',(374.730113419204,-2.06788146593666,-0.552029348212954));
#41040=CARTESIAN_POINT('Ctrl Pts',(374.742999937441,-2.07373475941556,-0.436684513719917));
#41041=CARTESIAN_POINT('Ctrl Pts',(374.755884519722,-2.07958717354782,-0.321357007606787));
#41042=CARTESIAN_POINT('Ctrl Pts',(374.763662856782,-2.08543958768007,-0.205438529059168));
#41043=CARTESIAN_POINT('Ctrl Pts',(374.7663012899,-2.09129200181233,-0.0894161825815296));
#41044=CARTESIAN_POINT('Ctrl Pts',(374.768939964745,-2.09714495212982,0.0266167936069241));
#41045=CARTESIAN_POINT('Ctrl Pts',(374.766437790135,-2.10299790244732,0.142753243570707));
#41046=CARTESIAN_POINT('Ctrl Pts',(374.758813231973,-2.10885085276482,0.258505361991111));
#41047=CARTESIAN_POINT('Ctrl Pts',(374.751186131278,-2.11470575484346,0.374296079831456));
#41048=CARTESIAN_POINT('Ctrl Pts',(374.738433277609,-2.1205606569221,0.48970179924492));
#41049=CARTESIAN_POINT('Ctrl Pts',(374.720624996025,-2.12641555900074,0.604239846263571));
#41050=CARTESIAN_POINT('Ctrl Pts',(374.70279653121,-2.13227709680322,0.718907706358394));
#41051=CARTESIAN_POINT('Ctrl Pts',(374.679901265995,-2.13813863460571,0.832705522798185));
#41052=CARTESIAN_POINT('Ctrl Pts',(374.652060667602,-2.14400017240819,0.9451607287999));
#41053=CARTESIAN_POINT('Ctrl Pts',(374.624201296653,-2.14986566256999,1.05769176189599));
#41054=CARTESIAN_POINT('Ctrl Pts',(374.591390069302,-2.15573115273178,1.1688779866112));
#41055=CARTESIAN_POINT('Ctrl Pts',(374.553797820794,-2.16159664289357,1.27826357643707));
#41056=CARTESIAN_POINT('Ctrl Pts',(374.51615060056,-2.16747071025231,1.38780912250208));
#41057=CARTESIAN_POINT('Ctrl Pts',(374.473708557019,-2.17334477761104,1.49554839575386));
#41058=CARTESIAN_POINT('Ctrl Pts',(374.426689986348,-2.17921884496978,1.60104698780224));
#41059=CARTESIAN_POINT('Ctrl Pts',(374.414794209437,-2.1807049938226,1.62773830779771));
#41060=CARTESIAN_POINT('Ctrl Pts',(374.402605714179,-2.18219114267543,1.65428633429488));
#41061=CARTESIAN_POINT('Ctrl Pts',(374.390128484359,-2.18367729152825,1.68068431167408));
#41062=CARTESIAN_POINT('Ctrl Pts',(374.340814742886,-2.18955099597836,1.78501700816801));
#41063=CARTESIAN_POINT('Ctrl Pts',(374.286823069956,-2.19542470042848,1.88735121811656));
#41064=CARTESIAN_POINT('Ctrl Pts',(374.228338108275,-2.20129840487859,1.98723816094113));
#41065=CARTESIAN_POINT('Ctrl Pts',(374.169928655086,-2.2071645259338,2.08699614219802));
#41066=CARTESIAN_POINT('Ctrl Pts',(374.107037656623,-2.213030646989,2.18431278648332));
#41067=CARTESIAN_POINT('Ctrl Pts',(374.039897142691,-2.2188967680442,2.27876071998403));
#41068=CARTESIAN_POINT('Ctrl Pts',(373.972825378801,-2.22475688235252,2.37311194139425));
#41069=CARTESIAN_POINT('Ctrl Pts',(373.901512992663,-2.23061699666084,2.46459996018473));
#41070=CARTESIAN_POINT('Ctrl Pts',(373.82623676315,-2.23647711096916,2.55282397286396));
#41071=CARTESIAN_POINT('Ctrl Pts',(373.748245014519,-2.24254862338461,2.64423058374904));
#41072=CARTESIAN_POINT('Ctrl Pts',(373.665998267915,-2.24862013580006,2.73213286109561));
#41073=CARTESIAN_POINT('Ctrl Pts',(373.579852176448,-2.2546916482155,2.81611972046616));
#41074=CARTESIAN_POINT('Ctrl Pts',(373.496801088157,-2.26054502711049,2.8970891522086));
#41075=CARTESIAN_POINT('Ctrl Pts',(373.410126341169,-2.26639840600548,2.97441935289265));
#41076=CARTESIAN_POINT('Ctrl Pts',(373.320185499786,-2.27225178490047,3.04777805028148));
#41077=CARTESIAN_POINT('Ctrl Pts',(373.230258162648,-2.27810428493482,3.12112573316519));
#41078=CARTESIAN_POINT('Ctrl Pts',(373.137066026264,-2.28395678496917,3.19050283737361));
#41079=CARTESIAN_POINT('Ctrl Pts',(373.041000174379,-2.28980928500352,3.25561701271872));
#41080=CARTESIAN_POINT('Ctrl Pts',(372.944925514806,-2.29566232161761,3.32073715798223));
#41081=CARTESIAN_POINT('Ctrl Pts',(372.845976957976,-2.30151535823171,3.38159336561159));
#41082=CARTESIAN_POINT('Ctrl Pts',(372.744574433297,-2.3073683948458,3.43793670655639));
#41083=CARTESIAN_POINT('Ctrl Pts',(372.643138089548,-2.31322338352427,3.49429883874342));
#41084=CARTESIAN_POINT('Ctrl Pts',(372.53924651148,-2.31907837220274,3.54614491086618));
#41085=CARTESIAN_POINT('Ctrl Pts',(372.433343429567,-2.32493336088122,3.59327235346863));
#41086=CARTESIAN_POINT('Ctrl Pts',(372.327320322671,-2.33079498529589,3.64045320783567));
#41087=CARTESIAN_POINT('Ctrl Pts',(372.219281539386,-2.33665660971056,3.68290459063861));
#41088=CARTESIAN_POINT('Ctrl Pts',(372.109690041444,-2.34251823412524,3.7204723868772));
#41089=CARTESIAN_POINT('Ctrl Pts',(372.00002464635,-2.34838381101207,3.75806551494505));
#41090=CARTESIAN_POINT('Ctrl Pts',(371.88880484719,-2.35424938789891,3.79076838312668));
#41091=CARTESIAN_POINT('Ctrl Pts',(371.776506301536,-2.36011496478575,3.81847743582001));
#41092=CARTESIAN_POINT('Ctrl Pts',(371.664043552036,-2.36598911836679,3.84622700491544));
#41093=CARTESIAN_POINT('Ctrl Pts',(371.550499311584,-2.37186327194783,3.86896810474756));
#41094=CARTESIAN_POINT('Ctrl Pts',(371.436356968969,-2.37773742552887,3.88664867245714));
#41095=CARTESIAN_POINT('Ctrl Pts',(371.407495143563,-2.37922275333255,3.89111934869017));
#41096=CARTESIAN_POINT('Ctrl Pts',(371.378595087753,-2.38070808113623,3.89526672833392));
#41097=CARTESIAN_POINT('Ctrl Pts',(371.349664624851,-2.38219340893991,3.899090497151));
#41098=CARTESIAN_POINT('Ctrl Pts',(371.235259727832,-2.38806710598372,3.91421150918715));
#41099=CARTESIAN_POINT('Ctrl Pts',(371.119998224111,-2.39394080302752,3.92431823209095));
#41100=CARTESIAN_POINT('Ctrl Pts',(371.004357323081,-2.39981450007133,3.9293225343169));
#41101=CARTESIAN_POINT('Ctrl Pts',(370.888865721855,-2.4056806137964,3.93432037566845));
#41102=CARTESIAN_POINT('Ctrl Pts',(370.77299610641,-2.41154672752147,3.93422887912462));
#41103=CARTESIAN_POINT('Ctrl Pts',(370.657233386885,-2.41741284124654,3.92901133770078));
#41104=CARTESIAN_POINT('Ctrl Pts',(370.541589203678,-2.42327294830962,3.92379913882726));
#41105=CARTESIAN_POINT('Ctrl Pts',(370.426052108943,-2.42913305537271,3.91347135398659));
#41106=CARTESIAN_POINT('Ctrl Pts',(370.311108944468,-2.43499316243579,3.89804328321253));
#41107=CARTESIAN_POINT('Ctrl Pts',(370.192019112406,-2.44106467759895,3.88205863231204));
#41108=CARTESIAN_POINT('Ctrl Pts',(370.073567323926,-2.44713619276211,3.86059873453573));
#41109=CARTESIAN_POINT('Ctrl Pts',(369.956291821024,-2.45320770792527,3.83373959558801));
#41110=CARTESIAN_POINT('Ctrl Pts',(369.843229905495,-2.45906107983606,3.80784547768828));
#41111=CARTESIAN_POINT('Ctrl Pts',(369.731261641927,-2.46491445174686,3.77693352036053));
#41112=CARTESIAN_POINT('Ctrl Pts',(369.620860079267,-2.47076782365766,3.74112405980109));
#41113=CARTESIAN_POINT('Ctrl Pts',(369.510475090904,-2.47662031681705,3.70531997522223));
#41114=CARTESIAN_POINT('Ctrl Pts',(369.401656728655,-2.48247280997644,3.66461997679757));
#41115=CARTESIAN_POINT('Ctrl Pts',(369.294862665814,-2.48832530313584,3.61919420948306));
#41116=CARTESIAN_POINT('Ctrl Pts',(369.188058809529,-2.49417833299227,3.5737642764439));
#41117=CARTESIAN_POINT('Ctrl Pts',(369.08328000188,-2.50003136284871,3.52360787473349));
#41118=CARTESIAN_POINT('Ctrl Pts',(368.980963066482,-2.50588439270515,3.46894292753008));
#41119=CARTESIAN_POINT('Ctrl Pts',(368.878612004814,-2.5117393747514,3.41425974765814));
#41120=CARTESIAN_POINT('Ctrl Pts',(368.778724812357,-2.51759435679765,3.35506522671987));
#41121=CARTESIAN_POINT('Ctrl Pts',(368.681712259107,-2.52344933884391,3.29162242005026));
#41122=CARTESIAN_POINT('Ctrl Pts',(368.58458975315,-2.52931095684717,3.22810770816659));
#41123=CARTESIAN_POINT('Ctrl Pts',(368.490348735288,-2.53517257485043,3.16033532645054));
#41124=CARTESIAN_POINT('Ctrl Pts',(368.39936968424,-2.54103419285368,3.08861075798817));
#41125=CARTESIAN_POINT('Ctrl Pts',(368.3083292844,-2.54689976345022,3.01683782437362));
#41126=CARTESIAN_POINT('Ctrl Pts',(368.220555543304,-2.55276533404675,2.94110766656594));
#41127=CARTESIAN_POINT('Ctrl Pts',(368.136393336658,-2.55863090464328,2.86176384471411));
#41128=CARTESIAN_POINT('Ctrl Pts',(368.052108063965,-2.56450505216076,2.78230400248942));
#41129=CARTESIAN_POINT('Ctrl Pts',(367.971445151871,-2.57037919967823,2.69922024582023));
#41130=CARTESIAN_POINT('Ctrl Pts',(367.894710397421,-2.57625334719571,2.61289054607839));
#41131=CARTESIAN_POINT('Ctrl Pts',(367.875306514429,-2.57773874024766,2.59106039356829));
#41132=CARTESIAN_POINT('Ctrl Pts',(367.856153596938,-2.57922413329961,2.56902283554765));
#41133=CARTESIAN_POINT('Ctrl Pts',(367.837256150676,-2.58070952635156,2.54678427651789));
#41134=CARTESIAN_POINT('Ctrl Pts',(367.762976104771,-2.58654814933545,2.45937134449326));
#41135=CARTESIAN_POINT('Ctrl Pts',(367.692389725622,-2.59238677231935,2.3685483759452));
#41136=CARTESIAN_POINT('Ctrl Pts',(367.625829426242,-2.59822539530325,2.27466283521863));
#41137=CARTESIAN_POINT('Ctrl Pts',(367.559413871114,-2.60405132142248,2.18098146112644));
#41138=CARTESIAN_POINT('Ctrl Pts',(367.497007195303,-2.60987724754172,2.08425112139886));
#41139=CARTESIAN_POINT('Ctrl Pts',(367.43890221528,-2.61570317366095,1.9848530539077));
#41140=CARTESIAN_POINT('Ctrl Pts',(367.380853286225,-2.62152347980066,1.88555087076066));
#41141=CARTESIAN_POINT('Ctrl Pts',(367.327098015095,-2.62734378594036,1.78358643416845));
#41142=CARTESIAN_POINT('Ctrl Pts',(367.277886848885,-2.63316409208007,1.67937116545977));
#41143=CARTESIAN_POINT('Ctrl Pts',(367.228710852137,-2.63898023865493,1.57523037568008));
#41144=CARTESIAN_POINT('Ctrl Pts',(367.184072681692,-2.64479638522979,1.46884232958704));
#41145=CARTESIAN_POINT('Ctrl Pts',(367.144177225176,-2.65061253180465,1.36064365108106));
#41146=CARTESIAN_POINT('Ctrl Pts',(367.104035865337,-2.65646452731802,1.2517780692015));
#41147=CARTESIAN_POINT('Ctrl Pts',(367.068696089812,-2.66231652283139,1.14107983564306));
#41148=CARTESIAN_POINT('Ctrl Pts',(367.038317611231,-2.66816851834475,1.02901465625417));
#41149=CARTESIAN_POINT('Ctrl Pts',(367.00814066676,-2.67398169108727,0.917692929379906));
#41150=CARTESIAN_POINT('Ctrl Pts',(366.982859474865,-2.67979486382978,0.805022755356134));
#41151=CARTESIAN_POINT('Ctrl Pts',(366.962580390979,-2.6856080365723,0.691475251508002));
#41152=CARTESIAN_POINT('Ctrl Pts',(366.942098158934,-2.69147944347109,0.576790271899731));
#41153=CARTESIAN_POINT('Ctrl Pts',(366.926718911473,-2.69735085036988,0.461210711058661));
#41154=CARTESIAN_POINT('Ctrl Pts',(366.916498975035,-2.70322225726867,0.345230702143492));
#41155=CARTESIAN_POINT('Ctrl Pts',(366.906279038596,-2.70909366416747,0.22925069322832));
#41156=CARTESIAN_POINT('Ctrl Pts',(366.901218424583,-2.71496507106626,0.112870675986645));
#41157=CARTESIAN_POINT('Ctrl Pts',(366.901319334106,-2.72083647796505,-0.00341300685045548));
#41158=CARTESIAN_POINT('',(366.901317853728,-3.97083647799244,6.29929319774584E-5));
#41159=CARTESIAN_POINT('Ctrl Pts',(366.901319334107,-2.72083647799451,-0.00341300743396402));
#41160=CARTESIAN_POINT('Ctrl Pts',(366.901441265661,-2.7279310477181,-0.143921527762734));
#41161=CARTESIAN_POINT('Ctrl Pts',(366.909096556454,-2.73502561744168,-0.284100586580425));
#41162=CARTESIAN_POINT('Ctrl Pts',(366.924157040721,-2.74212018716526,-0.423239199940604));
#41163=CARTESIAN_POINT('Ctrl Pts',(366.939429079127,-2.74931441408195,-0.564332288935045));
#41164=CARTESIAN_POINT('Ctrl Pts',(366.96231575338,-2.75650864099864,-0.704355514953356));
#41165=CARTESIAN_POINT('Ctrl Pts',(366.992634451626,-2.76370286791533,-0.842589842028374));
#41166=CARTESIAN_POINT('Ctrl Pts',(367.01444037844,-2.76887712653129,-0.942011248410526));
#41167=CARTESIAN_POINT('Ctrl Pts',(367.040089742119,-2.77405138514725,-1.04050775981355));
#41168=CARTESIAN_POINT('Ctrl Pts',(367.069499460836,-2.77922564376321,-1.13781873439388));
#41169=CARTESIAN_POINT('Ctrl Pts',(367.102884652554,-2.78509933529881,-1.24828376719106));
#41170=CARTESIAN_POINT('Ctrl Pts',(367.141191364605,-2.79097302683441,-1.35746218040211));
#41171=CARTESIAN_POINT('Ctrl Pts',(367.184303170996,-2.79684671837001,-1.46488286887288));
#41172=CARTESIAN_POINT('Ctrl Pts',(367.227359316144,-2.80271282643851,-1.57216486751786));
#41173=CARTESIAN_POINT('Ctrl Pts',(367.275208065812,-2.80857893450702,-1.67769327456226));
#41174=CARTESIAN_POINT('Ctrl Pts',(367.327682967674,-2.81444504257553,-1.78101116769307));
#41175=CARTESIAN_POINT('Ctrl Pts',(367.38010413606,-2.82030514384128,-1.88422326492003));
#41176=CARTESIAN_POINT('Ctrl Pts',(367.437141848167,-2.82616524510703,-1.98522898441801));
#41177=CARTESIAN_POINT('Ctrl Pts',(367.498581472885,-2.83202534637278,-2.08359108293439));
#41178=CARTESIAN_POINT('Ctrl Pts',(367.562237666942,-2.8380968636562,-2.18550181008616));
#41179=CARTESIAN_POINT('Ctrl Pts',(367.63061921938,-2.84416838093962,-2.28457414684417));
#41180=CARTESIAN_POINT('Ctrl Pts',(367.703435001426,-2.85023989822305,-2.3803490433799));
#41181=CARTESIAN_POINT('Ctrl Pts',(367.773634490001,-2.85609326402086,-2.47268271839094));
#41182=CARTESIAN_POINT('Ctrl Pts',(367.847954774005,-2.86194662981867,-2.56195147426968));
#41183=CARTESIAN_POINT('Ctrl Pts',(367.926091211913,-2.86779999561648,-2.64777393347103));
#41184=CARTESIAN_POINT('Ctrl Pts',(368.004215917966,-2.87365248255626,-2.7335835067944));
#41185=CARTESIAN_POINT('Ctrl Pts',(368.086155360562,-2.87950496949605,-2.81594750690446));
#41186=CARTESIAN_POINT('Ctrl Pts',(368.171565856825,-2.88535745643583,-2.89451909747916));
#41187=CARTESIAN_POINT('Ctrl Pts',(368.256984184116,-2.89121047997231,-2.97309789204371));
#41188=CARTESIAN_POINT('Ctrl Pts',(368.345873893653,-2.8970635035088,-3.0478833061231));
#41189=CARTESIAN_POINT('Ctrl Pts',(368.43785636777,-2.90291652704529,-3.11856719484054));
#41190=CARTESIAN_POINT('Ctrl Pts',(368.529869519808,-2.90877150267747,-3.18927465799169));
#41191=CARTESIAN_POINT('Ctrl Pts',(368.624977160095,-2.91462647830966,-3.25587762409626));
#41192=CARTESIAN_POINT('Ctrl Pts',(368.722770292194,-2.92048145394185,-3.31811029013596));
#41193=CARTESIAN_POINT('Ctrl Pts',(368.820674260018,-2.9263430654232,-3.38041348876383));
#41194=CARTESIAN_POINT('Ctrl Pts',(368.921269445856,-2.93220467690455,-3.43833627917756));
#41195=CARTESIAN_POINT('Ctrl Pts',(369.024120685343,-2.9380662883859,-3.49165794621909));
#41196=CARTESIAN_POINT('Ctrl Pts',(369.127041278082,-2.94393185238961,-3.54501556840394));
#41197=CARTESIAN_POINT('Ctrl Pts',(369.232220579747,-2.94979741639331,-3.59376571601081));
#41198=CARTESIAN_POINT('Ctrl Pts',(369.33920341154,-2.95566298039701,-3.63773580765107));
#41199=CARTESIAN_POINT('Ctrl Pts',(369.446342678002,-2.96153712126816,-3.68177019415657));
#41200=CARTESIAN_POINT('Ctrl Pts',(369.555290350564,-2.9674112621393,-3.72101043576224));
#41201=CARTESIAN_POINT('Ctrl Pts',(369.665576008652,-2.97328540301044,-3.7553337402616));
#41202=CARTESIAN_POINT('Ctrl Pts',(369.693465045456,-2.97477085573192,-3.76401341737478));
#41203=CARTESIAN_POINT('Ctrl Pts',(369.721439595303,-2.9762563084534,-3.77237892036187));
#41204=CARTESIAN_POINT('Ctrl Pts',(369.749491964837,-2.97774176117488,-3.78042878413089));
#41205=CARTESIAN_POINT('Ctrl Pts',(369.860414998906,-2.98361545119011,-3.81225908324459));
#41206=CARTESIAN_POINT('Ctrl Pts',(369.972924879248,-2.98948914120535,-3.83925630424393));
#41207=CARTESIAN_POINT('Ctrl Pts',(370.08656261712,-2.99536283122058,-3.86126289015381));
#41208=CARTESIAN_POINT('Ctrl Pts',(370.200053638318,-3.0012289377668,-3.8832410635561));
#41209=CARTESIAN_POINT('Ctrl Pts',(370.314669219303,-3.00709504431303,-3.90024133777752));
#41210=CARTESIAN_POINT('Ctrl Pts',(370.429935169522,-3.01296115085926,-3.91215588200705));
#41211=CARTESIAN_POINT('Ctrl Pts',(370.545083089184,-3.01882125060272,-3.92405822592678));
#41212=CARTESIAN_POINT('Ctrl Pts',(370.6608796449,-3.02468135034618,-3.93088515619367));
#41213=CARTESIAN_POINT('Ctrl Pts',(370.776841064394,-3.03054145008965,-3.93257999521253));
#41214=CARTESIAN_POINT('Ctrl Pts',(370.896986089165,-3.03661296794368,-3.93433597989082));
#41215=CARTESIAN_POINT('Ctrl Pts',(371.01730765464,-3.04268448579772,-3.93058248923657));
#41216=CARTESIAN_POINT('Ctrl Pts',(371.137262193632,-3.04875600365176,-3.92131530568698));
#41217=CARTESIAN_POINT('Ctrl Pts',(371.252906688351,-3.05460936793719,-3.91238109804404));
#41218=CARTESIAN_POINT('Ctrl Pts',(371.368209630447,-3.06046273222263,-3.89832263430311));
#41219=CARTESIAN_POINT('Ctrl Pts',(371.482685396514,-3.06631609650807,-3.87918915867836));
#41220=CARTESIAN_POINT('Ctrl Pts',(371.597143974651,-3.07216858194181,-3.86005855584379));
#41221=CARTESIAN_POINT('Ctrl Pts',(371.710775216324,-3.07802106737556,-3.8358545243301));
#41222=CARTESIAN_POINT('Ctrl Pts',(371.8231013587,-3.0838735528093,-3.80667784023));
#41223=CARTESIAN_POINT('Ctrl Pts',(371.935437800075,-3.08972657484777,-3.77749848096794));
#41224=CARTESIAN_POINT('Ctrl Pts',(372.046468504377,-3.09557959688623,-3.74334566663788));
#41225=CARTESIAN_POINT('Ctrl Pts',(372.155729283017,-3.10143261892469,-3.70437050431128));
#41226=CARTESIAN_POINT('Ctrl Pts',(372.265026502415,-3.10728759306855,-3.66538234295201));
#41227=CARTESIAN_POINT('Ctrl Pts',(372.372552233433,-3.11314256721241,-3.62156877418964));
#41228=CARTESIAN_POINT('Ctrl Pts',(372.47786139906,-3.11899754135627,-3.57312938653809));
#41229=CARTESIAN_POINT('Ctrl Pts',(372.58328991928,-3.12485915137134,-3.52463509897922));
#41230=CARTESIAN_POINT('Ctrl Pts',(372.686496484367,-3.13072076138641,-3.47150470100279));
#41231=CARTESIAN_POINT('Ctrl Pts',(372.787059719113,-3.13658237140148,-3.4139842127936));
#41232=CARTESIAN_POINT('Ctrl Pts',(372.887690764503,-3.14244793394998,-3.35642493803053));
#41233=CARTESIAN_POINT('Ctrl Pts',(372.985674582027,-3.14831349649848,-3.29446989871987));
#41234=CARTESIAN_POINT('Ctrl Pts',(373.08061939366,-3.15417905904698,-3.22840802709887));
#41235=CARTESIAN_POINT('Ctrl Pts',(373.175703037956,-3.16005319849043,-3.16224955677507));
#41236=CARTESIAN_POINT('Ctrl Pts',(373.267738480606,-3.16592733793389,-3.09197251904274));
#41237=CARTESIAN_POINT('Ctrl Pts',(373.356367519119,-3.17180147737734,-3.01790564510519));
#41238=CARTESIAN_POINT('Ctrl Pts',(373.37878025198,-3.17328694444707,-2.99917542883248));
#41239=CARTESIAN_POINT('Ctrl Pts',(373.40097533511,-3.1747724115168,-2.98020303382209));
#41240=CARTESIAN_POINT('Ctrl Pts',(373.422947366583,-3.17625787858653,-2.96099413078909));
#41241=CARTESIAN_POINT('Ctrl Pts',(373.509827023923,-3.18213156715133,-2.88504016561103));
#41242=CARTESIAN_POINT('Ctrl Pts',(373.593505655049,-3.18800525571613,-2.8051327049278));
#41243=CARTESIAN_POINT('Ctrl Pts',(373.673602041439,-3.19387894428093,-2.72157202707445));
#41244=CARTESIAN_POINT('Ctrl Pts',(373.753595015685,-3.19974504934853,-2.63811923409786));
#41245=CARTESIAN_POINT('Ctrl Pts',(373.830014659571,-3.20561115441613,-2.55102289936201));
#41246=CARTESIAN_POINT('Ctrl Pts',(373.902513298785,-3.21147725948372,-2.46062303245315));
#41247=CARTESIAN_POINT('Ctrl Pts',(373.974937700166,-3.21733735772231,-2.37031573404369));
#41248=CARTESIAN_POINT('Ctrl Pts',(374.043448826235,-3.22319745596089,-2.27671195247972));
#41249=CARTESIAN_POINT('Ctrl Pts',(374.107736792764,-3.22905755419947,-2.18018747961318));
#41250=CARTESIAN_POINT('Ctrl Pts',(374.174344135562,-3.23512907260775,-2.08018060430173));
#41251=CARTESIAN_POINT('Ctrl Pts',(374.236417527231,-3.24120059101603,-1.97703863982467));
#41252=CARTESIAN_POINT('Ctrl Pts',(374.293658750397,-3.24727210942431,-1.87121606372578));
#41253=CARTESIAN_POINT('Ctrl Pts',(374.348843239589,-3.25312547214878,-1.76919579783982));
#41254=CARTESIAN_POINT('Ctrl Pts',(374.399536619953,-3.25897883487324,-1.6646846337297));
#41255=CARTESIAN_POINT('Ctrl Pts',(374.44551701066,-3.26483219759771,-1.55811734003903));
#41256=CARTESIAN_POINT('Ctrl Pts',(374.491490497511,-3.27068468145237,-1.45156604719793));
#41257=CARTESIAN_POINT('Ctrl Pts',(374.532752238139,-3.27653716530704,-1.34295961787381));
#41258=CARTESIAN_POINT('Ctrl Pts',(374.56912791564,-3.2823896491617,-1.23275415135092));
#41259=CARTESIAN_POINT('Ctrl Pts',(374.605506928266,-3.28824266960461,-1.12253858057844));
#41260=CARTESIAN_POINT('Ctrl Pts',(374.636998857715,-3.29409569004751,-1.0107240735106));
#41261=CARTESIAN_POINT('Ctrl Pts',(374.663479039322,-3.29994871049042,-0.897782607807121));
#41262=CARTESIAN_POINT('Ctrl Pts',(374.689968052559,-3.30580368302387,-0.784803474036556));
#41263=CARTESIAN_POINT('Ctrl Pts',(374.711441899971,-3.31165865555731,-0.670697036266607));
#41264=CARTESIAN_POINT('Ctrl Pts',(374.727827016793,-3.31751362809076,-0.555945494812407));
#41265=CARTESIAN_POINT('Ctrl Pts',(374.744230704035,-3.32337523648144,-0.44106389726611));
#41266=CARTESIAN_POINT('Ctrl Pts',(374.755534090831,-3.32923684487212,-0.325536145945799));
#41267=CARTESIAN_POINT('Ctrl Pts',(374.761715478285,-3.33509845326281,-0.209849695415509));
#41268=CARTESIAN_POINT('Ctrl Pts',(374.767901033892,-3.34096401417679,-0.0940852367072996));
#41269=CARTESIAN_POINT('Ctrl Pts',(374.768957709119,-3.34682957509076,0.0218377221899005));
#41270=CARTESIAN_POINT('Ctrl Pts',(374.764915909321,-3.35269513600474,0.137433334413964));
#41271=CARTESIAN_POINT('Ctrl Pts',(374.760868199417,-3.35856927381135,0.253197975852862));
#41272=CARTESIAN_POINT('Ctrl Pts',(374.751707168292,-3.36444341161797,0.368633905063984));
#41273=CARTESIAN_POINT('Ctrl Pts',(374.737514866301,-3.37031754942459,0.483261913567972));
#41274=CARTESIAN_POINT('Ctrl Pts',(374.733925843954,-3.37180303161579,0.51224963412393));
#41275=CARTESIAN_POINT('Ctrl Pts',(374.730015320347,-3.37328851380699,0.541185748295071));
#41276=CARTESIAN_POINT('Ctrl Pts',(374.725785132249,-3.37477399599819,0.570062642416895));
#41277=CARTESIAN_POINT('Ctrl Pts',(374.709058703409,-3.38064768567527,0.684243691448876));
#41278=CARTESIAN_POINT('Ctrl Pts',(374.687274812471,-3.38652137535235,0.797878119513533));
#41279=CARTESIAN_POINT('Ctrl Pts',(374.660479123692,-3.39239506502944,0.910482801800082));
#41280=CARTESIAN_POINT('Ctrl Pts',(374.633718030649,-3.39826117122451,1.02294210092382));
#41281=CARTESIAN_POINT('Ctrl Pts',(374.601958102632,-3.40412727741957,1.13437389995395));
#41282=CARTESIAN_POINT('Ctrl Pts',(374.565296575013,-3.40999338361464,1.24430172287687));
#41283=CARTESIAN_POINT('Ctrl Pts',(374.528672588315,-3.41585348299443,1.35411698116069));
#41284=CARTESIAN_POINT('Ctrl Pts',(374.487157115496,-3.42171358237422,1.46243093703371));
#41285=CARTESIAN_POINT('Ctrl Pts',(374.440897946408,-3.427573681754,1.56877947189834));
#41286=CARTESIAN_POINT('Ctrl Pts',(374.392969855275,-3.43364519973966,1.6789648118273));
#41287=CARTESIAN_POINT('Ctrl Pts',(374.339949427173,-3.43971671772532,1.78703979826832));
#41288=CARTESIAN_POINT('Ctrl Pts',(374.2820568967,-3.44578823571098,1.89250746051153));
#41289=CARTESIAN_POINT('Ctrl Pts',(374.226244487294,-3.45164159960368,1.99418559231968));
#41290=CARTESIAN_POINT('Ctrl Pts',(374.165904282349,-3.45749496349637,2.09344014831928));
#41291=CARTESIAN_POINT('Ctrl Pts',(374.101281337829,-3.46334832738907,2.18984898800324));
#41292=CARTESIAN_POINT('Ctrl Pts',(374.036668096214,-3.46920081241996,2.28624335224225));
#41293=CARTESIAN_POINT('Ctrl Pts',(373.967773623597,-3.47505329745085,2.37979250665876));
#41294=CARTESIAN_POINT('Ctrl Pts',(373.894886685096,-3.48090578248174,2.4701027155506));
#41295=CARTESIAN_POINT('Ctrl Pts',(373.821993063834,-3.48675880410763,2.56042120468677));
#41296=CARTESIAN_POINT('Ctrl Pts',(373.74510650849,-3.49261182573351,2.64749983643588));
#41297=CARTESIAN_POINT('Ctrl Pts',(373.66455604385,-3.4984648473594,2.73097799044945));
#41298=CARTESIAN_POINT('Ctrl Pts',(373.583978714072,-3.50431982108134,2.81448398604389));
#41299=CARTESIAN_POINT('Ctrl Pts',(373.499735331858,-3.51017479480327,2.8943868189638));
#41300=CARTESIAN_POINT('Ctrl Pts',(373.412191213912,-3.51602976852521,2.97036326671578));
#41301=CARTESIAN_POINT('Ctrl Pts',(373.324547875972,-3.52189137810657,3.04642582399623));
#41302=CARTESIAN_POINT('Ctrl Pts',(373.233596647768,-3.52775298768792,3.11855284312599));
#41303=CARTESIAN_POINT('Ctrl Pts',(373.139735378167,-3.53361459726928,3.18646183653393));
#41304=CARTESIAN_POINT('Ctrl Pts',(373.045810817228,-3.53948015937665,3.25441662147055));
#41305=CARTESIAN_POINT('Ctrl Pts',(372.948972651852,-3.54534572148402,3.31814749059889));
#41306=CARTESIAN_POINT('Ctrl Pts',(372.849645626147,-3.5512112835914,3.37741661150713));
#41307=CARTESIAN_POINT('Ctrl Pts',(372.75017336002,-3.55708542258622,3.43677239837674));
#41308=CARTESIAN_POINT('Ctrl Pts',(372.64820533279,-3.56295956158103,3.49165322137719));
#41309=CARTESIAN_POINT('Ctrl Pts',(372.544188707529,-3.56883370057585,3.54186824452851));
#41310=CARTESIAN_POINT('Ctrl Pts',(372.517884652632,-3.57031917152052,3.55456677923165));
#41311=CARTESIAN_POINT('Ctrl Pts',(372.491449676109,-3.57180464246518,3.56696718210122));
#41312=CARTESIAN_POINT('Ctrl Pts',(372.464891171338,-3.57329011340984,3.57906686920676));
#41313=CARTESIAN_POINT('Ctrl Pts',(372.359876388396,-3.5791638028427,3.62691015052314));
#41314=CARTESIAN_POINT('Ctrl Pts',(372.252579237115,-3.58503749227556,3.67020727878392));
#41315=CARTESIAN_POINT('Ctrl Pts',(372.143430446049,-3.59091118170843,3.70873471945731));
#41316=CARTESIAN_POINT('Ctrl Pts',(372.034422576298,-3.59677728765789,3.74721241759496));
#41317=CARTESIAN_POINT('Ctrl Pts',(371.923568206989,-3.60264339360736,3.78093253835325));
#41318=CARTESIAN_POINT('Ctrl Pts',(371.811320436833,-3.60850949955683,3.80971848718799));
#41319=CARTESIAN_POINT('Ctrl Pts',(371.699187606936,-3.61436959868993,3.8384749595847));
#41320=CARTESIAN_POINT('Ctrl Pts',(371.585664612081,-3.62022969782304,3.86230720793486));
#41321=CARTESIAN_POINT('Ctrl Pts',(371.471221573008,-3.62608979695614,3.88108781808982));
#41322=CARTESIAN_POINT('Ctrl Pts',(371.352649691404,-3.63216131503386,3.90054598961159));
#41323=CARTESIAN_POINT('Ctrl Pts',(371.233090551928,-3.63823283311159,3.91458098755772));
#41324=CARTESIAN_POINT('Ctrl Pts',(371.113081154288,-3.64430435118931,3.92310846421301));
#41325=CARTESIAN_POINT('Ctrl Pts',(370.99738378895,-3.65015771483424,3.93132954190695));
#41326=CARTESIAN_POINT('Ctrl Pts',(370.8812684123,-3.65601107847918,3.93443203439467));
#41327=CARTESIAN_POINT('Ctrl Pts',(370.765222599452,-3.66186444212412,3.93239301773184));
#41328=CARTESIAN_POINT('Ctrl Pts',(370.64919421047,-3.66771692690728,3.93035430722012));
#41329=CARTESIAN_POINT('Ctrl Pts',(370.533235777493,-3.67356941169044,3.92317562979895));
#41330=CARTESIAN_POINT('Ctrl Pts',(370.417834702004,-3.67942189647361,3.91088618918392));
#41331=CARTESIAN_POINT('Ctrl Pts',(370.302423045765,-3.68527491785206,3.89859562179005));
#41332=CARTESIAN_POINT('Ctrl Pts',(370.187569259445,-3.69112793923052,3.8811934034429));
#41333=CARTESIAN_POINT('Ctrl Pts',(370.073754742584,-3.69698096060898,3.85876052052131));
#41334=CARTESIAN_POINT('Ctrl Pts',(369.959902266366,-3.70283593408407,3.83632015579633));
#41335=CARTESIAN_POINT('Ctrl Pts',(369.847090153966,-3.70869090755916,3.80884587006832));
#41336=CARTESIAN_POINT('Ctrl Pts',(369.735788053409,-3.71454588103425,3.77646941983088));
#41337=CARTESIAN_POINT('Ctrl Pts',(369.624359806195,-3.72040749037086,3.74405627503945));
#41338=CARTESIAN_POINT('Ctrl Pts',(369.514445383608,-3.72626909970748,3.70672999180798));
#41339=CARTESIAN_POINT('Ctrl Pts',(369.406497839792,-3.73213070904409,3.66467174645196));
#41340=CARTESIAN_POINT('Ctrl Pts',(369.298477506141,-3.73799627090767,3.62258514090692));
#41341=CARTESIAN_POINT('Ctrl Pts',(369.192427069188,-3.74386183277124,3.57576038611358));
#41342=CARTESIAN_POINT('Ctrl Pts',(369.088776639164,-3.74972739463482,3.52442546665648));
#41343=CARTESIAN_POINT('Ctrl Pts',(368.984974646777,-3.75560153338908,3.47301548295103));
#41344=CARTESIAN_POINT('Ctrl Pts',(368.88358002556,-3.76147567214334,3.41708237147469));
#41345=CARTESIAN_POINT('Ctrl Pts',(368.7849955478,-3.7673498108976,3.35689843285317));
#41346=CARTESIAN_POINT('Ctrl Pts',(368.760065150951,-3.76883528420557,3.34167890227506));
#41347=CARTESIAN_POINT('Ctrl Pts',(368.735314303328,-3.77032075751353,3.32618773625792));
#41348=CARTESIAN_POINT('Ctrl Pts',(368.710749184282,-3.7718062308215,3.31042974676844));
#41349=CARTESIAN_POINT('Ctrl Pts',(368.613616589462,-3.77767992012328,3.2481213001706));
#41350=CARTESIAN_POINT('Ctrl Pts',(368.519066868909,-3.78355360942506,3.18143044890821));
#41351=CARTESIAN_POINT('Ctrl Pts',(368.427521362484,-3.78942729872684,3.11059795733275));
#41352=CARTESIAN_POINT('Ctrl Pts',(368.336094049932,-3.79529340454241,3.03985691717658));
#41353=CARTESIAN_POINT('Ctrl Pts',(368.247663561768,-3.80115951035798,2.96498512114459));
#41354=CARTESIAN_POINT('Ctrl Pts',(368.162623920894,-3.80702561617355,2.88626757802382));
#41355=CARTESIAN_POINT('Ctrl Pts',(368.077671359549,-3.81288571517012,2.80763064068279));
#41356=CARTESIAN_POINT('Ctrl Pts',(367.996103040416,-3.8187458141667,2.72515606823728));
#41357=CARTESIAN_POINT('Ctrl Pts',(367.918280887532,-3.82460591316327,2.63916983438361));
#41358=CARTESIAN_POINT('Ctrl Pts',(367.837651087206,-3.83067743129119,2.55008141149203));
#41359=CARTESIAN_POINT('Ctrl Pts',(367.761043220298,-3.8367489494191,2.45722343393455));
#41360=CARTESIAN_POINT('Ctrl Pts',(367.688819277542,-3.84282046754701,2.36100142108893));
#41361=CARTESIAN_POINT('Ctrl Pts',(367.619190400276,-3.84867383104969,2.26823674407078));
#41362=CARTESIAN_POINT('Ctrl Pts',(367.553636102176,-3.85452719455238,2.17234597521138));
#41363=CARTESIAN_POINT('Ctrl Pts',(367.492439965521,-3.86038055805506,2.07372640039124));
#41364=CARTESIAN_POINT('Ctrl Pts',(367.431253017268,-3.8662330426941,1.97512163298217));
#41365=CARTESIAN_POINT('Ctrl Pts',(367.374423147118,-3.87208552733313,1.87378922524824));
#41366=CARTESIAN_POINT('Ctrl Pts',(367.322190039943,-3.87793801197217,1.77015457606821));
#41367=CARTESIAN_POINT('Ctrl Pts',(367.269952143699,-3.88379103320477,1.66651042499457));
#41368=CARTESIAN_POINT('Ctrl Pts',(367.222312034212,-3.88964405443738,1.56056398181326));
#41369=CARTESIAN_POINT('Ctrl Pts',(367.179462629267,-3.89549707566998,1.45276367379992));
#41370=CARTESIAN_POINT('Ctrl Pts',(367.136598933222,-3.90135204899762,1.34492741231271));
#41371=CARTESIAN_POINT('Ctrl Pts',(367.098529271382,-3.90720702232526,1.23523644025223));
#41372=CARTESIAN_POINT('Ctrl Pts',(367.065397528396,-3.9130619956529,1.1241568329647));
#41373=CARTESIAN_POINT('Ctrl Pts',(367.032228234837,-3.91892360484046,1.01295133121557));
#41374=CARTESIAN_POINT('Ctrl Pts',(367.004008148557,-3.92478521402803,0.900354449080872));
#41375=CARTESIAN_POINT('Ctrl Pts',(366.980830630642,-3.93064682321559,0.786845108896487));
#41376=CARTESIAN_POINT('Ctrl Pts',(366.957637483957,-3.93651238492899,0.67325922853615));
#41377=CARTESIAN_POINT('Ctrl Pts',(366.939493740771,-3.94237794664238,0.558760072016698));
#41378=CARTESIAN_POINT('Ctrl Pts',(366.926440990701,-3.94824350835577,0.443832656930772));
#41379=CARTESIAN_POINT('Ctrl Pts',(366.913369154308,-3.95411764695937,0.328737189769056));
#41380=CARTESIAN_POINT('Ctrl Pts',(366.905403196255,-3.95999178556298,0.213212624846767));
#41381=CARTESIAN_POINT('Ctrl Pts',(366.902532646884,-3.96586592416658,0.0977450316198287));
#41382=CARTESIAN_POINT('Ctrl Pts',(366.901806731355,-3.96735139885544,0.0685451439943927));
#41383=CARTESIAN_POINT('Ctrl Pts',(366.901406409168,-3.96883687354429,0.0393488768402862));
#41384=CARTESIAN_POINT('Ctrl Pts',(366.901330986672,-3.97032234823315,0.0101640313479354));
#41385=CARTESIAN_POINT('Ctrl Pts',(366.901322285313,-3.97049372481045,0.00679702754295266));
#41386=CARTESIAN_POINT('Ctrl Pts',(366.901317907657,-3.97066510138775,0.00343001255941355));
#41387=CARTESIAN_POINT('Ctrl Pts',(366.901317853728,-3.97083647796505,6.29934700403027E-5));
#41388=CARTESIAN_POINT('',(366.901319301027,-5.22083647793354,0.00337467329664299));
#41389=CARTESIAN_POINT('Ctrl Pts',(366.901317853728,-3.97083647799244,6.29929319748385E-5));
#41390=CARTESIAN_POINT('Ctrl Pts',(366.901316006288,-3.97670742792183,-0.115282994231212));
#41391=CARTESIAN_POINT('Ctrl Pts',(366.906392714759,-3.98257837785123,-0.230822054784923));
#41392=CARTESIAN_POINT('Ctrl Pts',(366.916573017939,-3.98844932778063,-0.346069943216802));
#41393=CARTESIAN_POINT('Ctrl Pts',(366.926740174846,-3.99431269629403,-0.461169006978742));
#41394=CARTESIAN_POINT('Ctrl Pts',(366.941997784334,-4.00017606480742,-0.575977238150028));
#41395=CARTESIAN_POINT('Ctrl Pts',(366.962318895233,-4.00603943332082,-0.690009470453848));
#41396=CARTESIAN_POINT('Ctrl Pts',(366.98261920661,-4.01189680042706,-0.803924985916004));
#41397=CARTESIAN_POINT('Ctrl Pts',(367.007972638632,-4.01775416753331,-0.917065677602088));
#41398=CARTESIAN_POINT('Ctrl Pts',(367.038300426437,-4.02361153463955,-1.0289512600367));
#41399=CARTESIAN_POINT('Ctrl Pts',(367.069631422851,-4.02966265676477,-1.14453788984538));
#41400=CARTESIAN_POINT('Ctrl Pts',(367.106271543185,-4.03571377888999,-1.25878448561143));
#41401=CARTESIAN_POINT('Ctrl Pts',(367.148076468894,-4.04176490101521,-1.37117229276752));
#41402=CARTESIAN_POINT('Ctrl Pts',(367.188496474471,-4.04761556061815,-1.47983689903133));
#41403=CARTESIAN_POINT('Ctrl Pts',(367.233744340121,-4.05346622022109,-1.58676350770212));
#41404=CARTESIAN_POINT('Ctrl Pts',(367.283639118081,-4.05931687982403,-1.69149919296599));
#41405=CARTESIAN_POINT('Ctrl Pts',(367.333526485669,-4.06516667048694,-1.79621932288472));
#41406=CARTESIAN_POINT('Ctrl Pts',(367.38805921546,-4.07101646114985,-1.89874880311661));
#41407=CARTESIAN_POINT('Ctrl Pts',(367.447008987533,-4.07686625181276,-1.99865646082808));
#41408=CARTESIAN_POINT('Ctrl Pts',(367.505964297075,-4.08271659197805,-2.09857350340442));
#41409=CARTESIAN_POINT('Ctrl Pts',(367.569337263499,-4.08856693214333,-2.19586787767364));
#41410=CARTESIAN_POINT('Ctrl Pts',(367.636854926471,-4.09441727230861,-2.29013533050827));
#41411=CARTESIAN_POINT('Ctrl Pts',(367.704395301767,-4.10026958047482,-2.38443449405184));
#41412=CARTESIAN_POINT('Ctrl Pts',(367.776082905224,-4.10612188864103,-2.47570437546677));
#41413=CARTESIAN_POINT('Ctrl Pts',(367.851603443936,-4.11197419680724,-2.56357245901625));
#41414=CARTESIAN_POINT('Ctrl Pts',(367.927209624855,-4.11783314163933,-2.65154018720096));
#41415=CARTESIAN_POINT('Ctrl Pts',(368.006657146676,-4.12369208647142,-2.73609810417007));
#41416=CARTESIAN_POINT('Ctrl Pts',(368.08959362769,-4.12955103130351,-2.81690928603809));
#41417=CARTESIAN_POINT('Ctrl Pts',(368.172586341101,-4.13541394860355,-2.89777525931286));
#41418=CARTESIAN_POINT('Ctrl Pts',(368.259072416014,-4.14127686590358,-2.97488916474135));
#41419=CARTESIAN_POINT('Ctrl Pts',(368.348666392974,-4.14713978320362,-3.0479543661541));
#41420=CARTESIAN_POINT('Ctrl Pts',(368.438390871182,-4.15301124034136,-3.12112599324715));
#41421=CARTESIAN_POINT('Ctrl Pts',(368.531231955111,-4.15888269747911,-3.19023690154316));
#41422=CARTESIAN_POINT('Ctrl Pts',(368.626775215789,-4.16475415461685,-3.25503371778361));
#41423=CARTESIAN_POINT('Ctrl Pts',(368.648929193589,-4.16611559162617,-3.27005840103452));
#41424=CARTESIAN_POINT('Ctrl Pts',(368.671228352797,-4.16747702863549,-3.28485133119991));
#41425=CARTESIAN_POINT('Ctrl Pts',(368.693667350086,-4.16883846564481,-3.29940970832898));
#41426=CARTESIAN_POINT('Ctrl Pts',(368.79047660343,-4.1747121550369,-3.362219360721));
#41427=CARTESIAN_POINT('Ctrl Pts',(368.890213818182,-4.18058584442899,-3.42086923500305));
#41428=CARTESIAN_POINT('Ctrl Pts',(368.992485948426,-4.18645953382108,-3.47507470919244));
#41429=CARTESIAN_POINT('Ctrl Pts',(369.094626035744,-4.19232563972848,-3.52921019902339));
#41430=CARTESIAN_POINT('Ctrl Pts',(369.199294168293,-4.19819174563587,-3.57891250832711));
#41431=CARTESIAN_POINT('Ctrl Pts',(369.306068251032,-4.20405785154327,-3.6239401420828));
#41432=CARTESIAN_POINT('Ctrl Pts',(369.412732998472,-4.20991795063308,-3.66892166811612));
#41433=CARTESIAN_POINT('Ctrl Pts',(369.521499028297,-4.21577804972288,-3.70923788037747));
#41434=CARTESIAN_POINT('Ctrl Pts',(369.63192015551,-4.22163814881268,-3.74469341555927));
#41435=CARTESIAN_POINT('Ctrl Pts',(369.746325025037,-4.22770966690618,-3.78142810554859));
#41436=CARTESIAN_POINT('Ctrl Pts',(369.862506271927,-4.23378118499967,-3.81294456082516));
#41437=CARTESIAN_POINT('Ctrl Pts',(369.979945211424,-4.23985270309316,-3.83908014880446));
#41438=CARTESIAN_POINT('Ctrl Pts',(370.093164476022,-4.24570606669193,-3.86427666423187));
#41439=CARTESIAN_POINT('Ctrl Pts',(370.207552170995,-4.2515594302907,-3.8844722379831));
#41440=CARTESIAN_POINT('Ctrl Pts',(370.322629435589,-4.25741279388947,-3.89957227952731));
#41441=CARTESIAN_POINT('Ctrl Pts',(370.43768942172,-4.26326527862549,-3.91467005385136));
#41442=CARTESIAN_POINT('Ctrl Pts',(370.553438362077,-4.26911776336151,-3.92467376349243));
#41443=CARTESIAN_POINT('Ctrl Pts',(370.669389878806,-4.27497024809754,-3.92954040102077));
#41444=CARTESIAN_POINT('Ctrl Pts',(370.785352026734,-4.28082326942793,-3.93440748475452));
#41445=CARTESIAN_POINT('Ctrl Pts',(370.901516375152,-4.28667629075833,-3.93413654274441));
#41446=CARTESIAN_POINT('Ctrl Pts',(371.017394844555,-4.29252931208872,-3.92873666911454));
#41447=CARTESIAN_POINT('Ctrl Pts',(371.133311961667,-4.29838428551486,-3.92333499452244));
#41448=CARTESIAN_POINT('Ctrl Pts',(371.248942597698,-4.30423925894099,-3.91280100608419));
#41449=CARTESIAN_POINT('Ctrl Pts',(371.363802807532,-4.31009423236713,-3.89719574606688));
#41450=CARTESIAN_POINT('Ctrl Pts',(371.478793196663,-4.31595584165372,-3.88157279949143));
#41451=CARTESIAN_POINT('Ctrl Pts',(371.593011007171,-4.32181745094032,-3.8608671650547));
#41452=CARTESIAN_POINT('Ctrl Pts',(371.705981416894,-4.32767906022691,-3.83519121189154));
#41453=CARTESIAN_POINT('Ctrl Pts',(371.819028003395,-4.33354462203976,-3.8094979452443));
#41454=CARTESIAN_POINT('Ctrl Pts',(371.930825116793,-4.33941018385262,-3.77882779527807));
#41455=CARTESIAN_POINT('Ctrl Pts',(372.040913723662,-4.34527574566547,-3.74334281163796));
#41456=CARTESIAN_POINT('Ctrl Pts',(372.151163307077,-4.35114988436842,-3.7078059402479));
#41457=CARTESIAN_POINT('Ctrl Pts',(372.25969901233,-4.35702402307136,-3.66744032764205));
#41458=CARTESIAN_POINT('Ctrl Pts',(372.366082308297,-4.36289816177431,-3.6224558871262));
#41459=CARTESIAN_POINT('Ctrl Pts',(372.392984906742,-4.36438363553503,-3.61108005665875));
#41460=CARTESIAN_POINT('Ctrl Pts',(372.419749985999,-4.36586910929575,-3.59940907819492));
#41461=CARTESIAN_POINT('Ctrl Pts',(372.446370724537,-4.36735458305647,-3.58744679961806));
#41462=CARTESIAN_POINT('Ctrl Pts',(372.55163138508,-4.37322827243772,-3.54014693440975));
#41463=CARTESIAN_POINT('Ctrl Pts',(372.65498382718,-4.37910196181898,-3.48813162499369));
#41464=CARTESIAN_POINT('Ctrl Pts',(372.755975806822,-4.38497565120024,-3.43157685465061));
#41465=CARTESIAN_POINT('Ctrl Pts',(372.856837396328,-4.39084175709653,-3.37509510183072));
#41466=CARTESIAN_POINT('Ctrl Pts',(372.955344226832,-4.39670786299282,-3.31408574345218));
#41467=CARTESIAN_POINT('Ctrl Pts',(373.051064546437,-4.40257396888911,-3.24877255253882));
#41468=CARTESIAN_POINT('Ctrl Pts',(373.146686849652,-4.40843406796754,-3.1835262415027));
#41469=CARTESIAN_POINT('Ctrl Pts',(373.239527978279,-4.41429416704596,-3.11398509543468));
#41470=CARTESIAN_POINT('Ctrl Pts',(373.329181885871,-4.42015426612438,-3.04041813877719));
#41471=CARTESIAN_POINT('Ctrl Pts',(373.422070302121,-4.42622578422203,-2.96419705398699));
#41472=CARTESIAN_POINT('Ctrl Pts',(373.511536785862,-4.43229730231969,-2.88365441067687));
#41473=CARTESIAN_POINT('Ctrl Pts',(373.597163491713,-4.43836882041735,-2.79913789904727));
#41474=CARTESIAN_POINT('Ctrl Pts',(373.679713561403,-4.4442221840042,-2.71765813340982));
#41475=CARTESIAN_POINT('Ctrl Pts',(373.7586947178,-4.45007554759105,-2.63248546851936));
#41476=CARTESIAN_POINT('Ctrl Pts',(373.833767880766,-4.45592891117791,-2.54397101639923));
#41477=CARTESIAN_POINT('Ctrl Pts',(373.908829771748,-4.46178139590183,-2.45546985442746));
#41478=CARTESIAN_POINT('Ctrl Pts',(373.979984568861,-4.46763388062576,-2.36362821790459));
#41479=CARTESIAN_POINT('Ctrl Pts',(374.046932462564,-4.47348636534969,-2.26883149922001));
#41480=CARTESIAN_POINT('Ctrl Pts',(374.113886494489,-4.47933938666779,-2.17402608895058));
#41481=CARTESIAN_POINT('Ctrl Pts',(374.176632617891,-4.4851924079859,-2.07626539540355));
#41482=CARTESIAN_POINT('Ctrl Pts',(374.234913882091,-4.49104542930401,-1.97596448562587));
#41483=CARTESIAN_POINT('Ctrl Pts',(374.293214584218,-4.49690040271769,-1.87563012355893));
#41484=CARTESIAN_POINT('Ctrl Pts',(374.347047258646,-4.50275537613138,-1.77275421764517));
#41485=CARTESIAN_POINT('Ctrl Pts',(374.396200848422,-4.50861034954506,-1.66777652235462));
#41486=CARTESIAN_POINT('Ctrl Pts',(374.445410147478,-4.51447195881902,-1.5626798483311));
#41487=CARTESIAN_POINT('Ctrl Pts',(374.489929601841,-4.52033356809298,-1.45547700475608));
#41488=CARTESIAN_POINT('Ctrl Pts',(374.529596230563,-4.52619517736695,-1.34662790479401));
#41489=CARTESIAN_POINT('Ctrl Pts',(374.569289606785,-4.53206073916705,-1.23770540708521));
#41490=CARTESIAN_POINT('Ctrl Pts',(374.604123517665,-4.53792630096715,-1.127134835646));
#41491=CARTESIAN_POINT('Ctrl Pts',(374.633985288407,-4.54379186276726,-1.01538976851875));
#41492=CARTESIAN_POINT('Ctrl Pts',(374.663890724381,-4.54966600145736,-0.903481302695676));
#41493=CARTESIAN_POINT('Ctrl Pts',(374.688809421587,-4.55554014014746,-0.790395315599256));
#41494=CARTESIAN_POINT('Ctrl Pts',(374.708680039928,-4.56141427883755,-0.676614104371761));
#41495=CARTESIAN_POINT('Ctrl Pts',(374.713704995249,-4.56289975271441,-0.647840691643158));
#41496=CARTESIAN_POINT('Ctrl Pts',(374.718407384881,-4.56438522659127,-0.61902283482409));
#41497=CARTESIAN_POINT('Ctrl Pts',(374.722786744215,-4.56587070046812,-0.590168352076625));
#41498=CARTESIAN_POINT('Ctrl Pts',(374.74010310156,-4.5717443898632,-0.47607528591433));
#41499=CARTESIAN_POINT('Ctrl Pts',(374.752422570739,-4.57761807925828,-0.361029423535447));
#41500=CARTESIAN_POINT('Ctrl Pts',(374.759647866103,-4.58349176865336,-0.245506191346751));
#41501=CARTESIAN_POINT('Ctrl Pts',(374.766863832933,-4.58935787456369,-0.130132110502376));
#41502=CARTESIAN_POINT('Ctrl Pts',(374.768998680004,-4.59522398047402,-0.0142822940982282));
#41503=CARTESIAN_POINT('Ctrl Pts',(374.766006388738,-4.60109008638435,0.101559143872355));
#41504=CARTESIAN_POINT('Ctrl Pts',(374.763017161541,-4.60695018547703,0.217281961687449));
#41505=CARTESIAN_POINT('Ctrl Pts',(374.754911249543,-4.6128102845697,0.332996007581691));
#41506=CARTESIAN_POINT('Ctrl Pts',(374.741694594454,-4.61867038366237,0.448214236826252));
#41507=CARTESIAN_POINT('Ctrl Pts',(374.728001112617,-4.62474190175476,0.567589276798935));
#41508=CARTESIAN_POINT('Ctrl Pts',(374.708821129095,-4.63081341984716,0.686431597997449));
#41509=CARTESIAN_POINT('Ctrl Pts',(374.684220292739,-4.63688493793955,0.804201595508767));
#41510=CARTESIAN_POINT('Ctrl Pts',(374.660503384068,-4.642738301541,0.917740023013324));
#41511=CARTESIAN_POINT('Ctrl Pts',(374.631748561313,-4.64859166514245,1.03028142046676));
#41512=CARTESIAN_POINT('Ctrl Pts',(374.598067048097,-4.6544450287439,1.14135051500074));
#41513=CARTESIAN_POINT('Ctrl Pts',(374.564390592047,-4.66029751348253,1.25240293288441));
#41514=CARTESIAN_POINT('Ctrl Pts',(374.525789036252,-4.66614999822116,1.36198309214184));
#41515=CARTESIAN_POINT('Ctrl Pts',(374.482423699357,-4.67200248295978,1.46963013558091));
#41516=CARTESIAN_POINT('Ctrl Pts',(374.439054386444,-4.67785550429271,1.57728704880895));
#41517=CARTESIAN_POINT('Ctrl Pts',(374.39092057855,-4.68370852562563,1.68301011064146));
#41518=CARTESIAN_POINT('Ctrl Pts',(374.338231764369,-4.68956154695855,1.78635839161207));
#41519=CARTESIAN_POINT('Ctrl Pts',(374.285525377451,-4.69541652038709,1.88974114122974));
#41520=CARTESIAN_POINT('Ctrl Pts',(374.228261150967,-4.70127149381563,1.9907471671861));
#41521=CARTESIAN_POINT('Ctrl Pts',(374.166694198068,-4.70712646724417,2.08896072158416));
#41522=CARTESIAN_POINT('Ctrl Pts',(374.105057466936,-4.71298807653309,2.18728558843171));
#41523=CARTESIAN_POINT('Ctrl Pts',(374.039108495572,-4.71884968582201,2.28281131650771));
#41524=CARTESIAN_POINT('Ctrl Pts',(373.969145399099,-4.72471129511092,2.37515162834309));
#41525=CARTESIAN_POINT('Ctrl Pts',(373.899135125997,-4.73057685692604,2.46755420592903));
#41526=CARTESIAN_POINT('Ctrl Pts',(373.825105601212,-4.73644241874116,2.55676677308016));
#41527=CARTESIAN_POINT('Ctrl Pts',(373.747393694012,-4.74230798055627,2.64243791711714));
#41528=CARTESIAN_POINT('Ctrl Pts',(373.669568152944,-4.74818211926135,2.72823433337842));
#41529=CARTESIAN_POINT('Ctrl Pts',(373.588049772981,-4.75405625796643,2.81047869938095));
#41530=CARTESIAN_POINT('Ctrl Pts',(373.503210579151,-4.75993039667151,2.88885801269218));
#41531=CARTESIAN_POINT('Ctrl Pts',(373.481756132711,-4.7614158704076,2.90867886085772));
#41532=CARTESIAN_POINT('Ctrl Pts',(373.460089473667,-4.76290134414369,2.92825274815523));
#41533=CARTESIAN_POINT('Ctrl Pts',(373.438216919809,-4.76438681787978,2.94757504587028));
#41534=CARTESIAN_POINT('Ctrl Pts',(373.351730983092,-4.77026050727015,3.02397705307453));
#41535=CARTESIAN_POINT('Ctrl Pts',(373.261735543641,-4.77613419666053,3.09669665584062));
#41536=CARTESIAN_POINT('Ctrl Pts',(373.168577366521,-4.7820078860509,3.16539437109851));
#41537=CARTESIAN_POINT('Ctrl Pts',(373.075539465359,-4.78787399195645,3.23400339115201));
#41538=CARTESIAN_POINT('Ctrl Pts',(372.979347276529,-4.793740097862,3.29860060718047));
#41539=CARTESIAN_POINT('Ctrl Pts',(372.880382657707,-4.79960620376755,3.35888490661022));
#41540=CARTESIAN_POINT('Ctrl Pts',(372.781519377394,-4.8054663028554,3.41910747568559));
#41541=CARTESIAN_POINT('Ctrl Pts',(372.679889664702,-4.81132640194326,3.47502569903849));
#41542=CARTESIAN_POINT('Ctrl Pts',(372.575906008195,-4.81718650103112,3.52638053795451));
#41543=CARTESIAN_POINT('Ctrl Pts',(372.468170858581,-4.8232580191253,3.57958814230175));
#41544=CARTESIAN_POINT('Ctrl Pts',(372.357909071984,-4.82932953721947,3.6278966043136));
#41545=CARTESIAN_POINT('Ctrl Pts',(372.245609671513,-4.83540105531365,3.67106856427793));
#41546=CARTESIAN_POINT('Ctrl Pts',(372.137345278253,-4.84125441891024,3.71268932121693));
#41547=CARTESIAN_POINT('Ctrl Pts',(372.027187596029,-4.84710778250683,3.74953617995246));
#41548=CARTESIAN_POINT('Ctrl Pts',(371.915596295746,-4.85296114610342,3.78144495262564));
#41549=CARTESIAN_POINT('Ctrl Pts',(371.80402175052,-4.85881363083717,3.81334893430402));
#41550=CARTESIAN_POINT('Ctrl Pts',(371.691014412357,-4.86466611557092,3.84031619062209));
#41551=CARTESIAN_POINT('Ctrl Pts',(371.577048995543,-4.87051860030466,3.86223244383732));
#41552=CARTESIAN_POINT('Ctrl Pts',(371.46307312963,-4.87637162163269,3.88415070647875));
#41553=CARTESIAN_POINT('Ctrl Pts',(371.348139416176,-4.88222464296072,3.90101696737458));
#41554=CARTESIAN_POINT('Ctrl Pts',(371.232731937483,-4.88807766428875,3.91276822945902));
#41555=CARTESIAN_POINT('Ctrl Pts',(371.117285968168,-4.89393263771242,3.92452341081629));
#41556=CARTESIAN_POINT('Ctrl Pts',(371.001366330216,-4.89978761113609,3.93116015932585));
#41557=CARTESIAN_POINT('Ctrl Pts',(370.885460679113,-4.90564258455976,3.93266746768146));
#41558=CARTESIAN_POINT('Ctrl Pts',(370.769423663841,-4.9115041938438,3.9341764843775));
#41559=CARTESIAN_POINT('Ctrl Pts',(370.653401080399,-4.91736580312783,3.93054445202538));
#41560=CARTESIAN_POINT('Ctrl Pts',(370.537879131819,-4.92322741241187,3.92181247441175));
#41561=CARTESIAN_POINT('Ctrl Pts',(370.42227928594,-4.92909297422208,3.91307460876149));
#41562=CARTESIAN_POINT('Ctrl Pts',(370.307181156296,-4.9349585360323,3.89922999939365));
#41563=CARTESIAN_POINT('Ctrl Pts',(370.193062657751,-4.94082409784251,3.88037121604094));
#41564=CARTESIAN_POINT('Ctrl Pts',(370.078777289972,-4.94669823654274,3.86148485652147));
#41565=CARTESIAN_POINT('Ctrl Pts',(369.965474814808,-4.95257237524297,3.83756977527947));
#41566=CARTESIAN_POINT('Ctrl Pts',(369.853619928964,-4.9584465139432,3.80876890626776));
#41567=CARTESIAN_POINT('Ctrl Pts',(369.82533365435,-4.95993198772594,3.80148563666511));
#41568=CARTESIAN_POINT('Ctrl Pts',(369.797139860427,-4.96141746150869,3.79389016329038));
#41569=CARTESIAN_POINT('Ctrl Pts',(369.769045861673,-4.96290293529143,3.78598528576341));
#41570=CARTESIAN_POINT('Ctrl Pts',(369.657959806633,-4.96877662468105,3.75472872923864));
#41571=CARTESIAN_POINT('Ctrl Pts',(369.548065570126,-4.97465031407066,3.71852684355877));
#41572=CARTESIAN_POINT('Ctrl Pts',(369.43983640708,-4.98052400346028,3.67748698112731));
#41573=CARTESIAN_POINT('Ctrl Pts',(369.331746978052,-4.98639010936504,3.63650010501407));
#41574=CARTESIAN_POINT('Ctrl Pts',(369.225318730081,-4.99225621526981,3.5906878191036));
#41575=CARTESIAN_POINT('Ctrl Pts',(369.121011699104,-4.99812232117457,3.54020776540811));
#41576=CARTESIAN_POINT('Ctrl Pts',(369.016811477197,-5.00398242026166,3.48977940264416));
#41577=CARTESIAN_POINT('Ctrl Pts',(368.914728521473,-5.00984251934875,3.4346929582895));
#41578=CARTESIAN_POINT('Ctrl Pts',(368.815204118168,-5.01570261843584,3.37515462237046));
#41579=CARTESIAN_POINT('Ctrl Pts',(368.712089101421,-5.02177413653031,3.31346827910653));
#41580=CARTESIAN_POINT('Ctrl Pts',(368.611721158483,-5.02784565462478,3.24700291130161));
#41581=CARTESIAN_POINT('Ctrl Pts',(368.514564848662,-5.03391717271925,3.17604077395487));
#41582=CARTESIAN_POINT('Ctrl Pts',(368.420899442719,-5.03977053631499,3.10762836293033));
#41583=CARTESIAN_POINT('Ctrl Pts',(368.330219210943,-5.04562389991074,3.03503703071258));
#41584=CARTESIAN_POINT('Ctrl Pts',(368.242911313649,-5.05147726350649,2.95856403456943));
#41585=CARTESIAN_POINT('Ctrl Pts',(368.155616525342,-5.05732974823937,2.88210252058951));
#41586=CARTESIAN_POINT('Ctrl Pts',(368.071693375414,-5.06318223297226,2.80176077368999));
#41587=CARTESIAN_POINT('Ctrl Pts',(367.99149523948,-5.06903471770514,2.71787574896006));
#41588=CARTESIAN_POINT('Ctrl Pts',(367.911289750453,-5.07488773903229,2.63398303309974));
#41589=CARTESIAN_POINT('Ctrl Pts',(367.834810239874,-5.08074076035944,2.54654669223868));
#41590=CARTESIAN_POINT('Ctrl Pts',(367.762372070291,-5.08659378168659,2.45593935322555));
#41591=CARTESIAN_POINT('Ctrl Pts',(367.68990974118,-5.09244875510936,2.36530179491538));
#41592=CARTESIAN_POINT('Ctrl Pts',(367.621491691082,-5.09830372853214,2.27149145800506));
#41593=CARTESIAN_POINT('Ctrl Pts',(367.5573915322,-5.10415870195491,2.17491215606009));
#41594=CARTESIAN_POINT('Ctrl Pts',(367.49321872402,-5.11002031123802,2.07822339388147));
#41595=CARTESIAN_POINT('Ctrl Pts',(367.43337380333,-5.11588192052113,1.97875974729758));
#41596=CARTESIAN_POINT('Ctrl Pts',(367.378085805582,-5.12174352980424,1.87695205928416));
#41597=CARTESIAN_POINT('Ctrl Pts',(367.322760526731,-5.12760909161352,1.77507572159938));
#41598=CARTESIAN_POINT('Ctrl Pts',(367.27199846984,-5.13347465342279,1.67085256566387));
#41599=CARTESIAN_POINT('Ctrl Pts',(367.225980930032,-5.13934021523207,1.5647343700214));
#41600=CARTESIAN_POINT('Ctrl Pts',(367.179896101293,-5.14521435393135,1.45846100354941));
#41601=CARTESIAN_POINT('Ctrl Pts',(367.138569782313,-5.15108849263063,1.35028745158122));
#41602=CARTESIAN_POINT('Ctrl Pts',(367.102133781073,-5.15696263132991,1.24068168825928));
#41603=CARTESIAN_POINT('Ctrl Pts',(367.092919711119,-5.15844810512097,1.21296417985523));
#41604=CARTESIAN_POINT('Ctrl Pts',(367.08401812311,-5.15993357891203,1.18515513506516));
#41605=CARTESIAN_POINT('Ctrl Pts',(367.075430629752,-5.16141905270309,1.15726221800515));
#41606=CARTESIAN_POINT('Ctrl Pts',(367.034031316038,-5.16858035029366,1.02279368618848));
#41607=CARTESIAN_POINT('Ctrl Pts',(366.99982432457,-5.17574164788424,0.886013496256454));
#41608=CARTESIAN_POINT('Ctrl Pts',(366.973028253342,-5.18290294547481,0.747617299051116));
#41609=CARTESIAN_POINT('Ctrl Pts',(366.946571909388,-5.18997345034808,0.610975723358209));
#41610=CARTESIAN_POINT('Ctrl Pts',(366.927339781937,-5.19704395522134,0.47275885287306));
#41611=CARTESIAN_POINT('Ctrl Pts',(366.915496348917,-5.20411446009461,0.333657035566035));
#41612=CARTESIAN_POINT('Ctrl Pts',(366.906159623003,-5.20968846604092,0.223996640628183));
#41613=CARTESIAN_POINT('Ctrl Pts',(366.901414039019,-5.21526247198723,0.11378665995732));
#41614=CARTESIAN_POINT('Ctrl Pts',(366.901319301027,-5.22083647793354,0.00337467329664173));
#41615=CARTESIAN_POINT('',(366.901318344487,-6.47083647800501,-0.00196577584637884));
#41616=CARTESIAN_POINT('Ctrl Pts',(366.901319301027,-5.22083647796505,0.00337467267254136));
#41617=CARTESIAN_POINT('Ctrl Pts',(366.901220385248,-5.22665628935448,-0.111906319793344));
#41618=CARTESIAN_POINT('Ctrl Pts',(366.906194278261,-5.23247610074391,-0.227277537418665));
#41619=CARTESIAN_POINT('Ctrl Pts',(366.916237979017,-5.23829591213334,-0.342255897440759));
#41620=CARTESIAN_POINT('Ctrl Pts',(366.92627823891,-5.24411372971836,-0.45719486712096));
#41621=CARTESIAN_POINT('Ctrl Pts',(366.94138481826,-5.24993154730338,-0.571740830287758));
#41622=CARTESIAN_POINT('Ctrl Pts',(366.961502674584,-5.25574936488841,-0.685413446100535));
#41623=CARTESIAN_POINT('Ctrl Pts',(366.981618648936,-5.26156663823225,-0.799075428145822));
#41624=CARTESIAN_POINT('Ctrl Pts',(367.006744895332,-5.26738391157609,-0.91186381321898));
#41625=CARTESIAN_POINT('Ctrl Pts',(367.036774959491,-5.27320118491992,-1.02330687980761));
#41626=CARTESIAN_POINT('Ctrl Pts',(367.066809693356,-5.27901936285557,-1.13476727590416));
#41627=CARTESIAN_POINT('Ctrl Pts',(367.101749651619,-5.28483754079121,-1.24488153367752));
#41628=CARTESIAN_POINT('Ctrl Pts',(367.141438277983,-5.29065571872685,-1.35319231551333));
#41629=CARTESIAN_POINT('Ctrl Pts',(367.181168991503,-5.2964800664544,-1.46161795375153));
#41630=CARTESIAN_POINT('Ctrl Pts',(367.225658286707,-5.30230441418196,-1.56823590254402));
#41631=CARTESIAN_POINT('Ctrl Pts',(367.274701058985,-5.30812876190951,-1.67260792721126));
#41632=CARTESIAN_POINT('Ctrl Pts',(367.3237696694,-5.31395617818903,-1.77703494017874));
#41633=CARTESIAN_POINT('Ctrl Pts',(367.377396339998,-5.31978359446856,-1.87921330207371));
#41634=CARTESIAN_POINT('Ctrl Pts',(367.435330423078,-5.32561101074808,-1.97873026198886));
#41635=CARTESIAN_POINT('Ctrl Pts',(367.493362906729,-5.33144832484695,-2.07841625065439));
#41636=CARTESIAN_POINT('Ctrl Pts',(367.555717193792,-5.33728563894582,-2.17543145344911));
#41637=CARTESIAN_POINT('Ctrl Pts',(367.622099516669,-5.34312295304469,-2.26939250864676));
#41638=CARTESIAN_POINT('Ctrl Pts',(367.685829398993,-5.34872702540138,-2.35959915902038));
#41639=CARTESIAN_POINT('Ctrl Pts',(367.753271360859,-5.35433109775806,-2.44699082150734));
#41640=CARTESIAN_POINT('Ctrl Pts',(367.824132815498,-5.35993517011475,-2.53125957551776));
#41641=CARTESIAN_POINT('Ctrl Pts',(367.898403479368,-5.36580885950525,-2.6195825761642));
#41642=CARTESIAN_POINT('Ctrl Pts',(367.976688413826,-5.37168254889576,-2.70478110188886));
#41643=CARTESIAN_POINT('Ctrl Pts',(368.058694720451,-5.37755623828626,-2.7864682350268));
#41644=CARTESIAN_POINT('Ctrl Pts',(368.140595149229,-5.38342234419195,-2.8680499024016));
#41645=CARTESIAN_POINT('Ctrl Pts',(368.226207105284,-5.38928845009763,-2.94612890400528));
#41646=CARTESIAN_POINT('Ctrl Pts',(368.315197321775,-5.39515455600332,-3.02035109681528));
#41647=CARTESIAN_POINT('Ctrl Pts',(368.404096413419,-5.40101465509129,-3.09449728704539));
#41648=CARTESIAN_POINT('Ctrl Pts',(368.496366569283,-5.40687475417926,-3.1647942609626));
#41649=CARTESIAN_POINT('Ctrl Pts',(368.591638020787,-5.41273485326723,-3.2309249711469));
#41650=CARTESIAN_POINT('Ctrl Pts',(368.690346648913,-5.41880637136136,-3.29944152648743));
#41651=CARTESIAN_POINT('Ctrl Pts',(368.792276901224,-5.42487788945549,-3.3634852049364));
#41652=CARTESIAN_POINT('Ctrl Pts',(368.896980114067,-5.43094940754962,-3.42274911210829));
#41653=CARTESIAN_POINT('Ctrl Pts',(368.997921256795,-5.43680277114631,-3.47988361973216));
#41654=CARTESIAN_POINT('Ctrl Pts',(369.101439129703,-5.44265613474301,-3.53257570586139));
#41655=CARTESIAN_POINT('Ctrl Pts',(369.207103307448,-5.4485094983397,-3.58059517706402));
#41656=CARTESIAN_POINT('Ctrl Pts',(369.312751620072,-5.45436198307355,-3.62860743830468));
#41657=CARTESIAN_POINT('Ctrl Pts',(369.420545220731,-5.4602144678074,-3.67194830873207));
#41658=CARTESIAN_POINT('Ctrl Pts',(369.530031443503,-5.46606695254125,-3.71043474021793));
#41659=CARTESIAN_POINT('Ctrl Pts',(369.63952770469,-5.47191997386937,-3.74892470039278));
#41660=CARTESIAN_POINT('Ctrl Pts',(369.750716506707,-5.47777299519749,-3.78255919981777));
#41661=CARTESIAN_POINT('Ctrl Pts',(369.863128354181,-5.4836260165256,-3.81120452835425));
#41662=CARTESIAN_POINT('Ctrl Pts',(369.975577693176,-5.48948098994937,-3.83985941066103));
#41663=CARTESIAN_POINT('Ctrl Pts',(370.089250488604,-5.49533596337313,-3.86352171135541));
#41664=CARTESIAN_POINT('Ctrl Pts',(370.203666042502,-5.5011909367969,-3.88210861435288));
#41665=CARTESIAN_POINT('Ctrl Pts',(370.318211271734,-5.507052546081,-3.9007165832175));
#41666=CARTESIAN_POINT('Ctrl Pts',(370.433500531635,-5.51291415536509,-3.91423760683375));
#41667=CARTESIAN_POINT('Ctrl Pts',(370.549046874426,-5.51877576464919,-3.92264062445891));
#41668=CARTESIAN_POINT('Ctrl Pts',(370.664671130964,-5.52464132645946,-3.93104930830056));
#41669=CARTESIAN_POINT('Ctrl Pts',(370.780552403619,-5.53050688826974,-3.93433310255362));
#41670=CARTESIAN_POINT('Ctrl Pts',(370.896204350897,-5.53637245008002,-3.93251307199427));
#41671=CARTESIAN_POINT('Ctrl Pts',(371.012025409687,-5.54224658878028,-3.93069038010385));
#41672=CARTESIAN_POINT('Ctrl Pts',(371.12761606305,-5.54812072748055,-3.92374899371211));
#41673=CARTESIAN_POINT('Ctrl Pts',(371.242495614349,-5.55399486618082,-3.91176174061286));
#41674=CARTESIAN_POINT('Ctrl Pts',(371.271546777462,-5.55548033996268,-3.90873035999623));
#41675=CARTESIAN_POINT('Ctrl Pts',(371.300552521484,-5.55696581374454,-3.90537654957443));
#41676=CARTESIAN_POINT('Ctrl Pts',(371.329505198997,-5.5584512875264,-3.90170199945949));
#41677=CARTESIAN_POINT('Ctrl Pts',(371.443986542801,-5.56432497691687,-3.88717251648342));
#41678=CARTESIAN_POINT('Ctrl Pts',(371.558018540075,-5.57019866630734,-3.86757600285981));
#41679=CARTESIAN_POINT('Ctrl Pts',(371.67111727785,-5.57607235569782,-3.84294883168461));
#41680=CARTESIAN_POINT('Ctrl Pts',(371.784069994528,-5.58193846160348,-3.81835345650102));
#41681=CARTESIAN_POINT('Ctrl Pts',(371.896091447911,-5.58780456750914,-3.78874042739306));
#41682=CARTESIAN_POINT('Ctrl Pts',(372.006703381712,-5.5936706734148,-3.75419780680135));
#41683=CARTESIAN_POINT('Ctrl Pts',(372.117202050302,-5.59953077250276,-3.71969055741302));
#41684=CARTESIAN_POINT('Ctrl Pts',(372.226293678196,-5.60539087159071,-3.68026387953297));
#41685=CARTESIAN_POINT('Ctrl Pts',(372.333511392892,-5.61125097067867,-3.63605661818084));
#41686=CARTESIAN_POINT('Ctrl Pts',(372.444597278135,-5.61732248877281,-3.59025445969113));
#41687=CARTESIAN_POINT('Ctrl Pts',(372.553671042936,-5.62339400686695,-3.53932035601467));
#41688=CARTESIAN_POINT('Ctrl Pts',(372.660231576705,-5.62946552496109,-3.4834649523722));
#41689=CARTESIAN_POINT('Ctrl Pts',(372.762963305331,-5.63531888855774,-3.42961647802234));
#41690=CARTESIAN_POINT('Ctrl Pts',(372.863358902254,-5.64117225215439,-3.37119447813759));
#41691=CARTESIAN_POINT('Ctrl Pts',(372.960991596452,-5.64702561575104,-3.3084358524636));
#41692=CARTESIAN_POINT('Ctrl Pts',(373.058609631429,-5.65287810048484,-3.24568664978606));
#41693=CARTESIAN_POINT('Ctrl Pts',(373.153465241097,-5.65873058521864,-3.17860233934789));
#41694=CARTESIAN_POINT('Ctrl Pts',(373.245159214173,-5.66458306995244,-3.10746406774643));
#41695=CARTESIAN_POINT('Ctrl Pts',(373.336861594356,-5.67043609128049,-3.0363192737209));
#41696=CARTESIAN_POINT('Ctrl Pts',(373.42540143525,-5.67628911260855,-2.96112003290217));
#41697=CARTESIAN_POINT('Ctrl Pts',(373.51041186127,-5.68214213393659,-2.88218838039787));
#41698=CARTESIAN_POINT('Ctrl Pts',(373.595450639909,-5.68799710736029,-2.80323040266316));
#41699=CARTESIAN_POINT('Ctrl Pts',(373.676957360409,-5.69385208078399,-2.72053781891182));
#41700=CARTESIAN_POINT('Ctrl Pts',(373.754601840828,-5.69970705420768,-2.6344696680252));
#41701=CARTESIAN_POINT('Ctrl Pts',(373.832334321293,-5.70556866349174,-2.54830396994421));
#41702=CARTESIAN_POINT('Ctrl Pts',(373.906195547849,-5.71143027277579,-2.45875537565285));
#41703=CARTESIAN_POINT('Ctrl Pts',(373.975895440889,-5.71729188205984,-2.36621623286639));
#41704=CARTESIAN_POINT('Ctrl Pts',(374.045642333079,-5.72315744387009,-2.27361469025631));
#41705=CARTESIAN_POINT('Ctrl Pts',(374.111222071213,-5.72902300568033,-2.17801892359745));
#41706=CARTESIAN_POINT('Ctrl Pts',(374.172388705838,-5.73488856749057,-2.0798490288792));
#41707=CARTESIAN_POINT('Ctrl Pts',(374.233644781085,-5.7407627061908,-1.98153558569724));
#41708=CARTESIAN_POINT('Ctrl Pts',(374.290474672201,-5.74663684489102,-1.88064086103138));
#41709=CARTESIAN_POINT('Ctrl Pts',(374.342678986736,-5.75251098359125,-1.77760826867542));
#41710=CARTESIAN_POINT('Ctrl Pts',(374.355880605649,-5.75399645737352,-1.75155300807049));
#41711=CARTESIAN_POINT('Ctrl Pts',(374.368786662145,-5.75548193115579,-1.7253611212195));
#41712=CARTESIAN_POINT('Ctrl Pts',(374.381394430701,-5.75696740493806,-1.69903995053452));
#41713=CARTESIAN_POINT('Ctrl Pts',(374.431246617451,-5.76284109432869,-1.5949638080628));
#41714=CARTESIAN_POINT('Ctrl Pts',(374.476597343558,-5.76871478371933,-1.48851836949951));
#41715=CARTESIAN_POINT('Ctrl Pts',(374.517214839797,-5.77458847310996,-1.38012998891218));
#41716=CARTESIAN_POINT('Ctrl Pts',(374.557779895031,-5.78045457901578,-1.27188154790683));
#41717=CARTESIAN_POINT('Ctrl Pts',(374.593623729609,-5.7863206849216,-1.16169553684183));
#41718=CARTESIAN_POINT('Ctrl Pts',(374.624561075807,-5.79218679082742,-1.05002157771301));
#41719=CARTESIAN_POINT('Ctrl Pts',(374.655466742557,-5.79804688991551,-0.938461971295911));
#41720=CARTESIAN_POINT('Ctrl Pts',(374.681475804798,-5.8039069890036,-0.8254178432435));
#41721=CARTESIAN_POINT('Ctrl Pts',(374.702451839065,-5.80976708809169,-0.711356779387259));
#41722=CARTESIAN_POINT('Ctrl Pts',(374.724184640795,-5.81583860618577,-0.593180652563559));
#41723=CARTESIAN_POINT('Ctrl Pts',(374.740514239084,-5.82191012427986,-0.473913250040106));
#41724=CARTESIAN_POINT('Ctrl Pts',(374.751345983948,-5.82798164237394,-0.35408985175764));
#41725=CARTESIAN_POINT('Ctrl Pts',(374.761788535562,-5.83383500597076,-0.238571803934091));
#41726=CARTESIAN_POINT('Ctrl Pts',(374.767121478564,-5.83968836956758,-0.122537474222565));
#41727=CARTESIAN_POINT('Ctrl Pts',(374.767312525039,-5.8455417331644,-0.00647390726555887));
#41728=CARTESIAN_POINT('Ctrl Pts',(374.767503542829,-5.85139421789838,0.109572233137454));
#41729=CARTESIAN_POINT('Ctrl Pts',(374.762554198516,-5.85724670263235,0.22564718902378));
#41730=CARTESIAN_POINT('Ctrl Pts',(374.752484325558,-5.86309918736633,0.341263087776295));
#41731=CARTESIAN_POINT('Ctrl Pts',(374.742413529328,-5.86895220869458,0.456889586954512));
#41732=CARTESIAN_POINT('Ctrl Pts',(374.727221307014,-5.87480523002283,0.572056533719801));
#41733=CARTESIAN_POINT('Ctrl Pts',(374.7069793805,-5.88065825135108,0.686281061344037));
#41734=CARTESIAN_POINT('Ctrl Pts',(374.686730702912,-5.88651322477496,0.800543685053763));
#41735=CARTESIAN_POINT('Ctrl Pts',(374.661429044272,-5.89236819819884,0.913862858034044));
#41736=CARTESIAN_POINT('Ctrl Pts',(374.631197112997,-5.89822317162272,1.02576648741553));
#41737=CARTESIAN_POINT('Ctrl Pts',(374.600930917711,-5.90408478090695,1.13779694518774));
#41738=CARTESIAN_POINT('Ctrl Pts',(374.56572340463,-5.90994639019118,1.24840825813228));
#41739=CARTESIAN_POINT('Ctrl Pts',(374.525747011703,-5.91580799947541,1.35714397465026));
#41740=CARTESIAN_POINT('Ctrl Pts',(374.485743662401,-5.92167356128584,1.46595301246082));
#41741=CARTESIAN_POINT('Ctrl Pts',(374.440965189286,-5.92753912309628,1.5728835553525));
#41742=CARTESIAN_POINT('Ctrl Pts',(374.391631270778,-5.93340468490672,1.67750119203868));
#41743=CARTESIAN_POINT('Ctrl Pts',(374.342225213981,-5.93927882360712,1.78227180536844));
#41744=CARTESIAN_POINT('Ctrl Pts',(374.288250609583,-5.94515296230752,1.88472239868276));
#41745=CARTESIAN_POINT('Ctrl Pts',(374.229971969129,-5.95102710100793,1.98444504210553));
#41746=CARTESIAN_POINT('Ctrl Pts',(374.215234252371,-5.95251257478852,2.00966327063081));
#41747=CARTESIAN_POINT('Ctrl Pts',(374.20022150031,-5.95399804856911,2.03470720212601));
#41748=CARTESIAN_POINT('Ctrl Pts',(374.1849384053,-5.95548352234971,2.05957056592035));
#41749=CARTESIAN_POINT('Ctrl Pts',(374.124507750657,-5.96135721174026,2.15788241634833));
#41750=CARTESIAN_POINT('Ctrl Pts',(374.059645873288,-5.96723090113082,2.25369607201985));
#41751=CARTESIAN_POINT('Ctrl Pts',(373.99058539756,-5.97310459052138,2.34658564484079));
#41752=CARTESIAN_POINT('Ctrl Pts',(373.921614085394,-5.97897069642712,2.43935528849655));
#41753=CARTESIAN_POINT('Ctrl Pts',(373.84845519928,-5.98483680233285,2.52920802854297));
#41754=CARTESIAN_POINT('Ctrl Pts',(373.771386124717,-5.99070290823859,2.61574443870009));
#41755=CARTESIAN_POINT('Ctrl Pts',(373.694395967904,-5.99656300732661,2.70219223667548));
#41756=CARTESIAN_POINT('Ctrl Pts',(373.613503860036,-6.00242310641462,2.78533015275468));
#41757=CARTESIAN_POINT('Ctrl Pts',(373.529028760698,-6.00828320550263,2.86479006650444));
#41758=CARTESIAN_POINT('Ctrl Pts',(373.441505992494,-6.01435472359674,2.94711671266566));
#41759=CARTESIAN_POINT('Ctrl Pts',(373.350137088781,-6.02042624169086,3.02549459551221));
#41760=CARTESIAN_POINT('Ctrl Pts',(373.255320538837,-6.02649775978497,3.09955399957096));
#41761=CARTESIAN_POINT('Ctrl Pts',(373.163910823308,-6.03235112338171,3.17095239005482));
#41762=CARTESIAN_POINT('Ctrl Pts',(373.06929730463,-6.03820448697844,3.23833701764739));
#41763=CARTESIAN_POINT('Ctrl Pts',(372.971871746654,-6.04405785057518,3.30141671902837));
#41764=CARTESIAN_POINT('Ctrl Pts',(372.874460816798,-6.04991033530907,3.36448694920454));
#41765=CARTESIAN_POINT('Ctrl Pts',(372.774239033879,-6.05576282004297,3.42325331391514));
#41766=CARTESIAN_POINT('Ctrl Pts',(372.671627112992,-6.06161530477687,3.47746799898576));
#41767=CARTESIAN_POINT('Ctrl Pts',(372.56900578397,-6.06746832610504,3.53168765481516));
#41768=CARTESIAN_POINT('Ctrl Pts',(372.463994246656,-6.07332134743322,3.58135460838357));
#41769=CARTESIAN_POINT('Ctrl Pts',(372.357037138867,-6.07917436876139,3.62626736150693));
#41770=CARTESIAN_POINT('Ctrl Pts',(372.250044358818,-6.08502934218518,3.67119509390058));
#41771=CARTESIAN_POINT('Ctrl Pts',(372.141105098732,-6.09088431560897,3.71136531305037));
#41772=CARTESIAN_POINT('Ctrl Pts',(372.030682583354,-6.09673928903277,3.74662520576861));
#41773=CARTESIAN_POINT('Ctrl Pts',(371.920134918237,-6.10260089831691,3.78192506104642));
#41774=CARTESIAN_POINT('Ctrl Pts',(371.808101036282,-6.10846250760106,3.81230335629673));
#41775=CARTESIAN_POINT('Ctrl Pts',(371.695057977601,-6.1143241168852,3.83765754572866));
#41776=CARTESIAN_POINT('Ctrl Pts',(371.581938693155,-6.12018967869554,3.86302883167673));
#41777=CARTESIAN_POINT('Ctrl Pts',(371.467809282695,-6.12605524050587,3.88336919365227));
#41778=CARTESIAN_POINT('Ctrl Pts',(371.353153875195,-6.1319208023162,3.89862773066437));
#41779=CARTESIAN_POINT('Ctrl Pts',(371.238330813369,-6.13779494101652,3.91390857939995));
#41780=CARTESIAN_POINT('Ctrl Pts',(371.12298062946,-6.14366907971683,3.9240927368195));
#41781=CARTESIAN_POINT('Ctrl Pts',(371.007589504371,-6.14954321841715,3.92918133138555));
#41782=CARTESIAN_POINT('Ctrl Pts',(370.978408972608,-6.15102869219855,3.93046815387949));
#41783=CARTESIAN_POINT('Ctrl Pts',(370.949225804753,-6.15251416597996,3.93142937397184));
#41784=CARTESIAN_POINT('Ctrl Pts',(370.92004781387,-6.15399963976136,3.93206553529409));
#41785=CARTESIAN_POINT('Ctrl Pts',(370.804675561844,-6.15987332915193,3.93458097114762));
#41786=CARTESIAN_POINT('Ctrl Pts',(370.68900035449,-6.16574701854249,3.93201852063393));
#41787=CARTESIAN_POINT('Ctrl Pts',(370.573506176798,-6.17162070793306,3.92434278184764));
#41788=CARTESIAN_POINT('Ctrl Pts',(370.458161112939,-6.1774868138388,3.91667695316123));
#41789=CARTESIAN_POINT('Ctrl Pts',(370.342997022408,-6.18335291974455,3.90391099203652));
#41790=CARTESIAN_POINT('Ctrl Pts',(370.228499919559,-6.18921902565029,3.88606145489872));
#41791=CARTESIAN_POINT('Ctrl Pts',(370.114120060284,-6.19507912473834,3.86823019545951));
#41792=CARTESIAN_POINT('Ctrl Pts',(370.00040623596,-6.20093922382639,3.84532577747242));
#41793=CARTESIAN_POINT('Ctrl Pts',(369.887840692103,-6.20679932291444,3.81741666359283));
#41794=CARTESIAN_POINT('Ctrl Pts',(369.771214040227,-6.21287084100855,3.78850065255539));
#41795=CARTESIAN_POINT('Ctrl Pts',(369.65582053851,-6.21894235910265,3.75421204151894));
#41796=CARTESIAN_POINT('Ctrl Pts',(369.542186886595,-6.22501387719676,3.71468525787553));
#41797=CARTESIAN_POINT('Ctrl Pts',(369.432636182606,-6.23086724079351,3.67657870315747));
#41798=CARTESIAN_POINT('Ctrl Pts',(369.324721462914,-6.23672060439025,3.63360406847479));
#41799=CARTESIAN_POINT('Ctrl Pts',(369.21889977325,-6.242573967987,3.58593271365957));
#41800=CARTESIAN_POINT('Ctrl Pts',(369.113093972357,-6.2484264527209,3.53826851653782));
#41801=CARTESIAN_POINT('Ctrl Pts',(369.009380953208,-6.25427893745481,3.48590917112673));
#41802=CARTESIAN_POINT('Ctrl Pts',(368.908197029654,-6.26013142218871,3.4290738652016));
#41803=CARTESIAN_POINT('Ctrl Pts',(368.807003828892,-6.26598444351687,3.37223334824221));
#41804=CARTESIAN_POINT('Ctrl Pts',(368.708340544919,-6.27183746484502,3.31091625730278));
#41805=CARTESIAN_POINT('Ctrl Pts',(368.612617540628,-6.27769048617318,3.24538699094737));
#41806=CARTESIAN_POINT('Ctrl Pts',(368.516862610866,-6.28354545959698,3.1798358693162));
#41807=CARTESIAN_POINT('Ctrl Pts',(368.424050251476,-6.28940043302078,3.11007001205794));
#41808=CARTESIAN_POINT('Ctrl Pts',(368.334559991117,-6.29525540644457,3.03639582907697));
#41809=CARTESIAN_POINT('Ctrl Pts',(368.244968305043,-6.30111701572871,2.96263814587257));
#41810=CARTESIAN_POINT('Ctrl Pts',(368.158706552196,-6.30697862501285,2.88496355849596));
#41811=CARTESIAN_POINT('Ctrl Pts',(368.076119510592,-6.31284023429699,2.80371733644894));
#41812=CARTESIAN_POINT('Ctrl Pts',(367.99347677994,-6.31870579610733,2.72241632947761));
#41813=CARTESIAN_POINT('Ctrl Pts',(367.914513975261,-6.32457135791766,2.63753919395571));
#41814=CARTESIAN_POINT('Ctrl Pts',(367.839536319979,-6.33043691972799,2.54946515334727));
#41815=CARTESIAN_POINT('Ctrl Pts',(367.764449028975,-6.33631105842832,2.46126232688987));
#41816=CARTESIAN_POINT('Ctrl Pts',(367.693358769784,-6.34218519712865,2.36985359077362));
#41817=CARTESIAN_POINT('Ctrl Pts',(367.626528157443,-6.34805933582898,2.27564809837513));
#41818=CARTESIAN_POINT('Ctrl Pts',(367.609627786598,-6.34954480961033,2.2518250672626));
#41819=CARTESIAN_POINT('Ctrl Pts',(367.592999592957,-6.35103028339168,2.22782330886293));
#41820=CARTESIAN_POINT('Ctrl Pts',(367.576647355237,-6.35251575717303,2.20364968326253));
#41821=CARTESIAN_POINT('Ctrl Pts',(367.510968455758,-6.35848217503169,2.10655611399077));
#41822=CARTESIAN_POINT('Ctrl Pts',(367.449530811241,-6.36444859289036,2.00637148061744));
#41823=CARTESIAN_POINT('Ctrl Pts',(367.392633063595,-6.37041501074903,1.90349541865323));
#41824=CARTESIAN_POINT('Ctrl Pts',(367.335814919807,-6.37637308117918,1.80076328736784));
#41825=CARTESIAN_POINT('Ctrl Pts',(367.283524226256,-6.38233115160934,1.69534756210725));
#41826=CARTESIAN_POINT('Ctrl Pts',(367.236017055976,-6.3882892220395,1.58767766644368));
#41827=CARTESIAN_POINT('Ctrl Pts',(367.188566178526,-6.39424023255341,1.48013535242832));
#41828=CARTESIAN_POINT('Ctrl Pts',(367.145887704166,-6.40019124306732,1.37034454303869));
#41829=CARTESIAN_POINT('Ctrl Pts',(367.108192119715,-6.40614225358123,1.25875971419715));
#41830=CARTESIAN_POINT('Ctrl Pts',(367.070540033329,-6.41208639704585,1.14730364643201));
#41831=CARTESIAN_POINT('Ctrl Pts',(367.037859510265,-6.41803054051047,1.03405805614495));
#41832=CARTESIAN_POINT('Ctrl Pts',(367.010312890166,-6.42397468397509,0.919497168298037));
#41833=CARTESIAN_POINT('Ctrl Pts',(366.982784981765,-6.42991478973863,0.805014098664051));
#41834=CARTESIAN_POINT('Ctrl Pts',(366.960384129132,-6.43585489550216,0.689217893220492));
#41835=CARTESIAN_POINT('Ctrl Pts',(366.943222766006,-6.44179500126569,0.572597609344167));
#41836=CARTESIAN_POINT('Ctrl Pts',(366.926069341682,-6.44773235915183,0.456031273706099));
#41837=CARTESIAN_POINT('Ctrl Pts',(366.914150640268,-6.45366971703798,0.33864200960788));
#41838=CARTESIAN_POINT('Ctrl Pts',(366.907527853233,-6.45960707492412,0.220928259789999));
#41839=CARTESIAN_POINT('Ctrl Pts',(366.903352598499,-6.4633502092711,0.14671707217018));
#41840=CARTESIAN_POINT('Ctrl Pts',(366.901281186748,-6.46709334361807,0.0723770988410905));
#41841=CARTESIAN_POINT('Ctrl Pts',(366.901318344487,-6.47083647796505,-0.00196577505274522));
#41842=CARTESIAN_POINT('',(366.901318562436,-7.72083647791836,-0.00236191956902979));
#41843=CARTESIAN_POINT('Ctrl Pts',(366.901318344487,-6.47083647800501,-0.00196577584638068));
#41844=CARTESIAN_POINT('Ctrl Pts',(366.90138468552,-6.47751942771998,-0.134696701814077));
#41845=CARTESIAN_POINT('Ctrl Pts',(366.908174895024,-6.48420237743496,-0.267198358871215));
#41846=CARTESIAN_POINT('Ctrl Pts',(366.921591070369,-6.49088532714993,-0.398820915615153));
#41847=CARTESIAN_POINT('Ctrl Pts',(366.934591876209,-6.49736137039203,-0.526368391724456));
#41848=CARTESIAN_POINT('Ctrl Pts',(366.953814296689,-6.50383741363414,-0.653090193759929));
#41849=CARTESIAN_POINT('Ctrl Pts',(366.979118129333,-6.51031345687624,-0.778411259497541));
#41850=CARTESIAN_POINT('Ctrl Pts',(367.005634629937,-6.51709985982765,-0.909738247073178));
#41851=CARTESIAN_POINT('Ctrl Pts',(367.038829661962,-6.52388626277905,-1.03952658214836));
#41852=CARTESIAN_POINT('Ctrl Pts',(367.078485202183,-6.53067266573046,-1.16713756574511));
#41853=CARTESIAN_POINT('Ctrl Pts',(367.118140742404,-6.53745906868187,-1.29474854934185));
#41854=CARTESIAN_POINT('Ctrl Pts',(367.164256593428,-6.54424547163327,-1.42018191676854));
#41855=CARTESIAN_POINT('Ctrl Pts',(367.216559571197,-6.55103187458468,-1.5428266308395));
#41856=CARTESIAN_POINT('Ctrl Pts',(367.26182824266,-6.55690556397525,-1.64897667247503));
#41857=CARTESIAN_POINT('Ctrl Pts',(367.311848152075,-6.56277925336581,-1.75330944973659));
#41858=CARTESIAN_POINT('Ctrl Pts',(367.366452037994,-6.56865294275637,-1.85536942077916));
#41859=CARTESIAN_POINT('Ctrl Pts',(367.420985425167,-6.57451904866213,-1.95729762281101));
#41860=CARTESIAN_POINT('Ctrl Pts',(367.480090826079,-6.58038515456788,-2.05695849323852));
#41861=CARTESIAN_POINT('Ctrl Pts',(367.543552804627,-6.58625126047363,-2.15391606032704));
#41862=CARTESIAN_POINT('Ctrl Pts',(367.606949798918,-6.59211135956167,-2.25077434410206));
#41863=CARTESIAN_POINT('Ctrl Pts',(367.674694272473,-6.59797145864971,-2.34493448698793));
#41864=CARTESIAN_POINT('Ctrl Pts',(367.746525052225,-6.60383155773775,-2.43598534849786));
#41865=CARTESIAN_POINT('Ctrl Pts',(367.820947322637,-6.60990307583185,-2.53032111737081));
#41866=CARTESIAN_POINT('Ctrl Pts',(367.899756102272,-6.61597459392596,-2.62131861919165));
#41867=CARTESIAN_POINT('Ctrl Pts',(367.98261179353,-6.62204611202007,-2.70855340525223));
#41868=CARTESIAN_POINT('Ctrl Pts',(368.062490413584,-6.62789947561682,-2.7926537757333));
#41869=CARTESIAN_POINT('Ctrl Pts',(368.146129823731,-6.63375283921357,-2.87325684653535));
#41870=CARTESIAN_POINT('Ctrl Pts',(368.233185491794,-6.63960620281031,-2.95001685390454));
#41871=CARTESIAN_POINT('Ctrl Pts',(368.320228088741,-6.64545868754421,-3.02676533601691));
#41872=CARTESIAN_POINT('Ctrl Pts',(368.410685613885,-6.65131117227811,-3.09967162887043));
#41873=CARTESIAN_POINT('Ctrl Pts',(368.504178506474,-6.65716365701201,-3.1684285733985));
#41874=CARTESIAN_POINT('Ctrl Pts',(368.597679971106,-6.66301667834019,-3.23719182201525));
#41875=CARTESIAN_POINT('Ctrl Pts',(368.694217023573,-6.66886969966836,-3.30180472124366));
#41876=CARTESIAN_POINT('Ctrl Pts',(368.793379610461,-6.67472272099653,-3.36200239280498));
#41877=CARTESIAN_POINT('Ctrl Pts',(368.892575269986,-6.68057769442036,-3.42222014145235));
#41878=CARTESIAN_POINT('Ctrl Pts',(368.994397852182,-6.68643266784418,-3.47801952002925));
#41879=CARTESIAN_POINT('Ctrl Pts',(369.098411738974,-6.69228764126801,-3.52918106116823));
#41880=CARTESIAN_POINT('Ctrl Pts',(369.202543512145,-6.69814925055216,-3.58040058734258));
#41881=CARTESIAN_POINT('Ctrl Pts',(369.30887117602,-6.70401085983632,-3.62697160218351));
#41882=CARTESIAN_POINT('Ctrl Pts',(369.416938033824,-6.70987246912047,-3.66872231813177));
#41883=CARTESIAN_POINT('Ctrl Pts',(369.525077761904,-6.71573803093081,-3.71050118689439));
#41884=CARTESIAN_POINT('Ctrl Pts',(369.634958628495,-6.72160359274114,-3.74745315320668));
#41885=CARTESIAN_POINT('Ctrl Pts',(369.746109307894,-6.72746915455148,-3.77945646381478));
#41886=CARTESIAN_POINT('Ctrl Pts',(369.857422516848,-6.73334329325182,-3.81150657111234));
#41887=CARTESIAN_POINT('Ctrl Pts',(369.970008844132,-6.73921743195215,-3.83859348490398));
#41888=CARTESIAN_POINT('Ctrl Pts',(370.083387260216,-6.74509157065248,-3.86064660963485));
#41889=CARTESIAN_POINT('Ctrl Pts',(370.112058810727,-6.74657704443377,-3.86622348485934));
#41890=CARTESIAN_POINT('Ctrl Pts',(370.140780994845,-6.74806251821505,-3.87147870792583));
#41891=CARTESIAN_POINT('Ctrl Pts',(370.169546004779,-6.74954799199634,-3.87641166409289));
#41892=CARTESIAN_POINT('Ctrl Pts',(370.283285295097,-6.7554216813869,-3.89591699139492));
#41893=CARTESIAN_POINT('Ctrl Pts',(370.398073215185,-6.76129537077747,-3.91044465986015));
#41894=CARTESIAN_POINT('Ctrl Pts',(370.513436295632,-6.76716906016804,-3.91988826702975));
#41895=CARTESIAN_POINT('Ctrl Pts',(370.628650431505,-6.77303516607379,-3.9293196816153));
#41896=CARTESIAN_POINT('Ctrl Pts',(370.744437842971,-6.77890127197954,-3.93368005515114));
#41897=CARTESIAN_POINT('Ctrl Pts',(370.860315389599,-6.7847673778853,-3.9329140758606));
#41898=CARTESIAN_POINT('Ctrl Pts',(370.976074279097,-6.79062747697333,-3.93214888092309));
#41899=CARTESIAN_POINT('Ctrl Pts',(371.09192270949,-6.79648757606136,-3.92626777720643));
#41900=CARTESIAN_POINT('Ctrl Pts',(371.207373611798,-6.80234767514939,-3.9152673473206));
#41901=CARTESIAN_POINT('Ctrl Pts',(371.326989719275,-6.8084191932435,-3.90387004702048));
#41902=CARTESIAN_POINT('Ctrl Pts',(371.446178623122,-6.81449071133761,-3.88697702227996));
#41903=CARTESIAN_POINT('Ctrl Pts',(371.56439955667,-6.82056222943172,-3.86464354194443));
#41904=CARTESIAN_POINT('Ctrl Pts',(371.678372717596,-6.82641559302847,-3.84311252140584));
#41905=CARTESIAN_POINT('Ctrl Pts',(371.791445830236,-6.83226895662522,-3.81652536002251));
#41906=CARTESIAN_POINT('Ctrl Pts',(371.903141572424,-6.83812232022197,-3.7849841290653));
#41907=CARTESIAN_POINT('Ctrl Pts',(372.014820543872,-6.84397480495587,-3.75344763391778));
#41908=CARTESIAN_POINT('Ctrl Pts',(372.12512215859,-6.84982728968977,-3.71695866046873));
#41909=CARTESIAN_POINT('Ctrl Pts',(372.233582544911,-6.85567977442367,-3.67566964274513));
#41910=CARTESIAN_POINT('Ctrl Pts',(372.342052875593,-6.86153279575184,-3.63437683937295));
#41911=CARTESIAN_POINT('Ctrl Pts',(372.448681256152,-6.86738581708002,-3.58828326384426));
#41912=CARTESIAN_POINT('Ctrl Pts',(372.553022813437,-6.87323883840819,-3.53758989422734));
#41913=CARTESIAN_POINT('Ctrl Pts',(372.657399170646,-6.87909381183201,-3.48687961739263));
#41914=CARTESIAN_POINT('Ctrl Pts',(372.759486816577,-6.88494878525584,-3.4315666763854));
#41915=CARTESIAN_POINT('Ctrl Pts',(372.858865178378,-6.89080375867967,-3.37189814914575));
#41916=CARTESIAN_POINT('Ctrl Pts',(372.958356172787,-6.89666536796382,-3.31216199529465));
#41917=CARTESIAN_POINT('Ctrl Pts',(373.05513139988,-6.90252697724797,-3.24806061504836));
#41918=CARTESIAN_POINT('Ctrl Pts',(373.148798925558,-6.90838858653212,-3.17988464661986));
#41919=CARTESIAN_POINT('Ctrl Pts',(373.242529611936,-6.91425414834247,-3.11166270663513));
#41920=CARTESIAN_POINT('Ctrl Pts',(373.333148102055,-6.92011971015281,-3.03936096456918));
#41921=CARTESIAN_POINT('Ctrl Pts',(373.420296575553,-6.92598527196315,-2.96330947551237));
#41922=CARTESIAN_POINT('Ctrl Pts',(373.507572481494,-6.93185941066348,-2.88714678052573));
#41923=CARTESIAN_POINT('Ctrl Pts',(373.59136794654,-6.93773354936381,-2.80722367981111));
#41924=CARTESIAN_POINT('Ctrl Pts',(373.671362878008,-6.94360768806415,-2.72390611573636));
#41925=CARTESIAN_POINT('Ctrl Pts',(373.69159229025,-6.94509316184543,-2.70283646395128));
#41926=CARTESIAN_POINT('Ctrl Pts',(373.711578864619,-6.94657863562671,-2.68154989365513));
#41927=CARTESIAN_POINT('Ctrl Pts',(373.731317851865,-6.94806410940799,-2.66005263253818));
#41928=CARTESIAN_POINT('Ctrl Pts',(373.809367482516,-6.95393779879856,-2.57505063779416));
#41929=CARTESIAN_POINT('Ctrl Pts',(373.883802819557,-6.95981148818913,-2.48646903502814));
#41930=CARTESIAN_POINT('Ctrl Pts',(373.954277779898,-6.96568517757969,-2.39464800251529));
#41931=CARTESIAN_POINT('Ctrl Pts',(374.024661750443,-6.97155128348545,-2.30294551958161));
#41932=CARTESIAN_POINT('Ctrl Pts',(374.091095263553,-6.97741738939121,-2.20801224908474));
#41933=CARTESIAN_POINT('Ctrl Pts',(374.153269925284,-6.98328349529696,-2.11022419267893));
#41934=CARTESIAN_POINT('Ctrl Pts',(374.215380920954,-6.989143594385,-2.01253626999715));
#41935=CARTESIAN_POINT('Ctrl Pts',(374.273241519302,-6.99500369347304,-1.91199972259126));
#41936=CARTESIAN_POINT('Ctrl Pts',(374.326584803942,-7.00086379256108,-1.80902198574878));
#41937=CARTESIAN_POINT('Ctrl Pts',(374.381852592596,-7.00693531065518,-1.70232904709086));
#41938=CARTESIAN_POINT('Ctrl Pts',(374.432270689726,-7.01300682874929,-1.59301580650699));
#41939=CARTESIAN_POINT('Ctrl Pts',(374.477592383421,-7.0190783468434,-1.48156663623885));
#41940=CARTESIAN_POINT('Ctrl Pts',(374.521285632442,-7.02493171044015,-1.37412192372638));
#41941=CARTESIAN_POINT('Ctrl Pts',(374.560242241898,-7.0307850740369,-1.26469254681109));
#41942=CARTESIAN_POINT('Ctrl Pts',(374.594289222193,-7.03663843763365,-1.15373493686026));
#41943=CARTESIAN_POINT('Ctrl Pts',(374.628331090449,-7.04249092236755,-1.04279398682117));
#41944=CARTESIAN_POINT('Ctrl Pts',(374.657464674142,-7.04834340710146,-0.930325654860274));
#41945=CARTESIAN_POINT('Ctrl Pts',(374.681566595537,-7.05419589183536,-0.816802371915838));
#41946=CARTESIAN_POINT('Ctrl Pts',(374.705670726756,-7.06004891316354,-0.703268680410562));
#41947=CARTESIAN_POINT('Ctrl Pts',(374.724742192778,-7.06590193449171,-0.588680249801158));
#41948=CARTESIAN_POINT('Ctrl Pts',(374.738708707085,-7.07175495581989,-0.473519862611013));
#41949=CARTESIAN_POINT('Ctrl Pts',(374.752679879494,-7.07760992924371,-0.358321067207775));
#41950=CARTESIAN_POINT('Ctrl Pts',(374.76154266493,-7.08346490266754,-0.242550345827211));
#41951=CARTESIAN_POINT('Ctrl Pts',(374.76527668838,-7.08931987609136,-0.126695052439334));
#41952=CARTESIAN_POINT('Ctrl Pts',(374.769014943865,-7.09518148537551,-0.0107084519574659));
#41953=CARTESIAN_POINT('Ctrl Pts',(374.767612822065,-7.10104309465967,0.105362498684048));
#41954=CARTESIAN_POINT('Ctrl Pts',(374.761102077346,-7.10690470394382,0.22103089644694));
#41955=CARTESIAN_POINT('Ctrl Pts',(374.754586942385,-7.11277026575416,0.336777290259909));
#41956=CARTESIAN_POINT('Ctrl Pts',(374.742956366527,-7.11863582756451,0.452120180645069));
#41957=CARTESIAN_POINT('Ctrl Pts',(374.726293719834,-7.12450138937485,0.566579962341262));
#41958=CARTESIAN_POINT('Ctrl Pts',(374.709606708265,-7.13037552807518,0.681207112311389));
#41959=CARTESIAN_POINT('Ctrl Pts',(374.687873018142,-7.13624966677552,0.794948172196397));
#41960=CARTESIAN_POINT('Ctrl Pts',(374.661226628422,-7.14212380547585,0.907335784765218));
#41961=CARTESIAN_POINT('Ctrl Pts',(374.654488191467,-7.14360927925711,0.935756777242086));
#41962=CARTESIAN_POINT('Ctrl Pts',(374.647435831465,-7.14509475303838,0.964091304736905));
#41963=CARTESIAN_POINT('Ctrl Pts',(374.640072206979,-7.14658022681965,0.992332000327942));
#41964=CARTESIAN_POINT('Ctrl Pts',(374.610955810874,-7.15245391621022,1.10399810724093));
#41965=CARTESIAN_POINT('Ctrl Pts',(374.576872099117,-7.15832760560079,1.21456763442592));
#41966=CARTESIAN_POINT('Ctrl Pts',(374.537919311246,-7.16420129499136,1.32356535166729));
#41967=CARTESIAN_POINT('Ctrl Pts',(374.499016815084,-7.17006740089712,1.43242234261573));
#41968=CARTESIAN_POINT('Ctrl Pts',(374.455257882231,-7.17593350680287,1.53971117384656));
#41969=CARTESIAN_POINT('Ctrl Pts',(374.406791286539,-7.18179961270863,1.64496886543727));
#41970=CARTESIAN_POINT('Ctrl Pts',(374.358374320023,-7.18765971179667,1.75011877449274));
#41971=CARTESIAN_POINT('Ctrl Pts',(374.305259450984,-7.19351981088471,1.85324130788152));
#41972=CARTESIAN_POINT('Ctrl Pts',(374.24764435258,-7.19937990997275,1.95389129912461));
#41973=CARTESIAN_POINT('Ctrl Pts',(374.187950632866,-7.20545142806686,2.05817251243229));
#41974=CARTESIAN_POINT('Ctrl Pts',(374.123425988981,-7.21152294616097,2.1597989824911));
#41975=CARTESIAN_POINT('Ctrl Pts',(374.054343697848,-7.21759446425507,2.2583008125483));
#41976=CARTESIAN_POINT('Ctrl Pts',(373.987743588644,-7.22344782785183,2.35326339313092));
#41977=CARTESIAN_POINT('Ctrl Pts',(373.91690797301,-7.22930119144858,2.44532164376667));
#41978=CARTESIAN_POINT('Ctrl Pts',(373.8421266145,-7.23515455504533,2.53408276415575));
#41979=CARTESIAN_POINT('Ctrl Pts',(373.76735648416,-7.24100703977924,2.62283055736129));
#41980=CARTESIAN_POINT('Ctrl Pts',(373.688642055061,-7.24685952451315,2.70828188879879));
#41981=CARTESIAN_POINT('Ctrl Pts',(373.606313430384,-7.25271200924705,2.79007697388538));
#41982=CARTESIAN_POINT('Ctrl Pts',(373.523977257278,-7.25856503057523,2.87187955848303));
#41983=CARTESIAN_POINT('Ctrl Pts',(373.438026522958,-7.26441805190341,2.95002493912412));
#41984=CARTESIAN_POINT('Ctrl Pts',(373.348827726156,-7.27027107323158,3.02419065188158));
#41985=CARTESIAN_POINT('Ctrl Pts',(373.259599179833,-7.27612604665541,3.09838110033653));
#41986=CARTESIAN_POINT('Ctrl Pts',(373.167120734459,-7.28198102007923,3.16858897764277));
#41987=CARTESIAN_POINT('Ctrl Pts',(373.071790871911,-7.28783599350305,3.23453296329564));
#41988=CARTESIAN_POINT('Ctrl Pts',(372.976352965209,-7.29369760278721,3.30055168798608));
#41989=CARTESIAN_POINT('Ctrl Pts',(372.878057530989,-7.29955921207137,3.36229664032892));
#41990=CARTESIAN_POINT('Ctrl Pts',(372.777330932039,-7.30542082135552,3.41953054900116));
#41991=CARTESIAN_POINT('Ctrl Pts',(372.676536412404,-7.31128638316587,3.47680305091834));
#41992=CARTESIAN_POINT('Ctrl Pts',(372.573307830703,-7.31715194497621,3.52955826466241));
#41993=CARTESIAN_POINT('Ctrl Pts',(372.468093398704,-7.32301750678656,3.57760624817654));
#41994=CARTESIAN_POINT('Ctrl Pts',(372.362725117399,-7.32889164548689,3.62572448962713));
#41995=CARTESIAN_POINT('Ctrl Pts',(372.255365572104,-7.33476578418723,3.66912160962422));
#41996=CARTESIAN_POINT('Ctrl Pts',(372.146480118032,-7.34063992288757,3.70765683293566));
#41997=CARTESIAN_POINT('Ctrl Pts',(372.118944764266,-7.34212539666881,3.71740176181865));
#41998=CARTESIAN_POINT('Ctrl Pts',(372.091311887034,-7.34361087045006,3.72683602521229));
#41999=CARTESIAN_POINT('Ctrl Pts',(372.063589118049,-7.3450963442313,3.7359578634502));
#42000=CARTESIAN_POINT('Ctrl Pts',(371.953970936889,-7.35097003362186,3.77202638593574));
#42001=CARTESIAN_POINT('Ctrl Pts',(371.842581391219,-7.35684372301243,3.80332636779904));
#42002=CARTESIAN_POINT('Ctrl Pts',(371.729873077309,-7.36271741240299,3.82968273367564));
#42003=CARTESIAN_POINT('Ctrl Pts',(371.617310280421,-7.36858351830874,3.8560050710078));
#42004=CARTESIAN_POINT('Ctrl Pts',(371.503432499929,-7.37444962421448,3.87739639218139));
#42005=CARTESIAN_POINT('Ctrl Pts',(371.388709433216,-7.38031573012023,3.89373072721186));
#42006=CARTESIAN_POINT('Ctrl Pts',(371.274103841462,-7.38617582920826,3.91004833609135));
#42007=CARTESIAN_POINT('Ctrl Pts',(371.15865509175,-7.39203592829629,3.92131920098413));
#42008=CARTESIAN_POINT('Ctrl Pts',(371.042844421464,-7.39789602738432,3.92746809921326));
#42009=CARTESIAN_POINT('Ctrl Pts',(370.922855566402,-7.40396754547843,3.93383883566263));
#42010=CARTESIAN_POINT('Ctrl Pts',(370.802478622983,-7.41003906357254,3.93471094705704));
#42011=CARTESIAN_POINT('Ctrl Pts',(370.682256595156,-7.41611058166665,3.93005933464048));
#42012=CARTESIAN_POINT('Ctrl Pts',(370.566354240868,-7.4219639452634,3.92557485837552));
#42013=CARTESIAN_POINT('Ctrl Pts',(370.450596309506,-7.42781730886014,3.91595678793313));
#42014=CARTESIAN_POINT('Ctrl Pts',(370.335469957822,-7.43367067245688,3.90123567312369));
#42015=CARTESIAN_POINT('Ctrl Pts',(370.220360891973,-7.43952315719078,3.88651676864012));
#42016=CARTESIAN_POINT('Ctrl Pts',(370.105883626943,-7.44537564192467,3.86669639568048));
#42017=CARTESIAN_POINT('Ctrl Pts',(369.992519444617,-7.45122812665857,3.84185689989449));
#42018=CARTESIAN_POINT('Ctrl Pts',(369.879144868317,-7.45708114798674,3.81701512666023));
#42019=CARTESIAN_POINT('Ctrl Pts',(369.766883981189,-7.46293416931491,3.78715340422476));
#42020=CARTESIAN_POINT('Ctrl Pts',(369.656206434648,-7.46878719064308,3.75240489358781));
#42021=CARTESIAN_POINT('Ctrl Pts',(369.545491975009,-7.4746421640669,3.71764479365149));
#42022=CARTESIAN_POINT('Ctrl Pts',(369.436362299972,-7.48049713749072,3.67799478834188));
#42023=CARTESIAN_POINT('Ctrl Pts',(369.329269826182,-7.48635211091454,3.63363721858656));
#42024=CARTESIAN_POINT('Ctrl Pts',(369.222055976828,-7.49221372019868,3.58922937522347));
#42025=CARTESIAN_POINT('Ctrl Pts',(369.11688431907,-7.49807532948283,3.54010347642571));
#42026=CARTESIAN_POINT('Ctrl Pts',(369.014185369185,-7.50393693876697,3.48648917114978));
#42027=CARTESIAN_POINT('Ctrl Pts',(368.911417168643,-7.50980250057731,3.43283871335409));
#42028=CARTESIAN_POINT('Ctrl Pts',(368.811125352605,-7.51566806238764,3.37469402922101));
#42029=CARTESIAN_POINT('Ctrl Pts',(368.713712510734,-7.52153362419797,3.31232878522059));
#42030=CARTESIAN_POINT('Ctrl Pts',(368.616157227395,-7.52740776289829,3.24987234793736));
#42031=CARTESIAN_POINT('Ctrl Pts',(368.521489656313,-7.53328190159861,3.18318327105412));
#42032=CARTESIAN_POINT('Ctrl Pts',(368.430080365508,-7.53915604029894,3.11257628061743));
#42033=CARTESIAN_POINT('Ctrl Pts',(368.406964448131,-7.54064151408028,3.094720925403));
#42034=CARTESIAN_POINT('Ctrl Pts',(368.384056717002,-7.54212698786162,3.07661520573756));
#42035=CARTESIAN_POINT('Ctrl Pts',(368.361362788011,-7.54361246164296,3.05826458067907));
#42036=CARTESIAN_POINT('Ctrl Pts',(368.272792509054,-7.5494099957431,2.9866454273343));
#42037=CARTESIAN_POINT('Ctrl Pts',(368.187169953114,-7.55520752984324,2.91104090485572));
#42038=CARTESIAN_POINT('Ctrl Pts',(368.104882304396,-7.56100506394338,2.83172572555944));
#42039=CARTESIAN_POINT('Ctrl Pts',(368.022701404712,-7.56679507709507,2.7525134392111));
#42040=CARTESIAN_POINT('Ctrl Pts',(367.943847116321,-7.57258509024677,2.66960035561438));
#42041=CARTESIAN_POINT('Ctrl Pts',(367.868675111064,-7.57837510339846,2.58330256181359));
#42042=CARTESIAN_POINT('Ctrl Pts',(367.791609172166,-7.58431099400346,2.49483052383489));
#42043=CARTESIAN_POINT('Ctrl Pts',(367.718413913144,-7.59024688460845,2.40280120236307));
#42044=CARTESIAN_POINT('Ctrl Pts',(367.649434223809,-7.59618277521345,2.30759729309164));
#42045=CARTESIAN_POINT('Ctrl Pts',(367.582267264402,-7.60196267545875,2.21489526484194));
#42046=CARTESIAN_POINT('Ctrl Pts',(367.519097337803,-7.60774257570405,2.11918379009273));
#42047=CARTESIAN_POINT('Ctrl Pts',(367.460202815846,-7.61352247594935,2.02085049287173));
#42048=CARTESIAN_POINT('Ctrl Pts',(367.401329349346,-7.619300309815,1.92255235091569));
#42049=CARTESIAN_POINT('Ctrl Pts',(367.346728467926,-7.62507814368065,1.821634613281));
#42050=CARTESIAN_POINT('Ctrl Pts',(367.296634832238,-7.63085597754629,1.71851326530402));
#42051=CARTESIAN_POINT('Ctrl Pts',(367.246546243089,-7.63663322934065,1.61540230599123));
#42052=CARTESIAN_POINT('Ctrl Pts',(367.200964181829,-7.64241048113501,1.51008856014474));
#42053=CARTESIAN_POINT('Ctrl Pts',(367.16007661686,-7.64818773292937,1.40301116781184));
#42054=CARTESIAN_POINT('Ctrl Pts',(367.117229971858,-7.65424179501179,1.29080328699221));
#42055=CARTESIAN_POINT('Ctrl Pts',(367.079539067204,-7.6602958570942,1.17665902241042));
#42056=CARTESIAN_POINT('Ctrl Pts',(367.04716232087,-7.66634991917662,1.06110412955548));
#42057=CARTESIAN_POINT('Ctrl Pts',(367.016232762133,-7.67213337458751,0.950714351380221));
#42058=CARTESIAN_POINT('Ctrl Pts',(366.990152592752,-7.67791682999841,0.83903776885068));
#42059=CARTESIAN_POINT('Ctrl Pts',(366.969007692485,-7.6837002854093,0.726544122050305));
#42060=CARTESIAN_POINT('Ctrl Pts',(366.947850984632,-7.68948697037646,0.613987657343232));
#42061=CARTESIAN_POINT('Ctrl Pts',(366.931635090475,-7.69527365534362,0.500613639997401));
#42062=CARTESIAN_POINT('Ctrl Pts',(366.920394058982,-7.70106034031079,0.386897315662876));
#42063=CARTESIAN_POINT('Ctrl Pts',(366.909138803071,-7.70685434775759,0.273037094524837));
#42064=CARTESIAN_POINT('Ctrl Pts',(366.902870989076,-7.7126483552044,0.158834124779586));
#42065=CARTESIAN_POINT('Ctrl Pts',(366.90157260312,-7.7184423626512,0.0447637999302818));
#42066=CARTESIAN_POINT('Ctrl Pts',(366.90139376975,-7.71924040107359,0.0290523078551138));
#42067=CARTESIAN_POINT('Ctrl Pts',(366.901309130825,-7.72003843949597,0.0133433237785408));
#42068=CARTESIAN_POINT('Ctrl Pts',(366.901318562436,-7.72083647791836,-0.00236191956903193));
#42069=CARTESIAN_POINT('',(366.901319333012,-8.9708364780123,0.00341174547326769));
#42070=CARTESIAN_POINT('Ctrl Pts',(366.901318562437,-7.72083647796505,-0.0023619204878646));
#42071=CARTESIAN_POINT('Ctrl Pts',(366.901402442653,-7.7279338449949,-0.142036744660448));
#42072=CARTESIAN_POINT('Ctrl Pts',(366.908926347075,-7.73503121202476,-0.281485965734132));
#42073=CARTESIAN_POINT('Ctrl Pts',(366.923821666102,-7.74212857905462,-0.420129230717656));
#42074=CARTESIAN_POINT('Ctrl Pts',(366.936148839964,-7.74800226844519,-0.534868608177298));
#42075=CARTESIAN_POINT('Ctrl Pts',(366.95355074276,-7.75387595783576,-0.649256079205153));
#42076=CARTESIAN_POINT('Ctrl Pts',(366.976000305937,-7.75974964722634,-0.762807121295737));
#42077=CARTESIAN_POINT('Ctrl Pts',(366.99842088462,-7.76561575313211,-0.876211558323485));
#42078=CARTESIAN_POINT('Ctrl Pts',(367.025876084103,-7.77148185903788,-0.988781312399423));
#42079=CARTESIAN_POINT('Ctrl Pts',(367.058287047345,-7.77734796494365,-1.10003652350796));
#42080=CARTESIAN_POINT('Ctrl Pts',(367.090664822173,-7.7832080640317,-1.21117781069763));
#42081=CARTESIAN_POINT('Ctrl Pts',(367.127988152016,-7.78906816311975,-1.32100683807669));
#42082=CARTESIAN_POINT('Ctrl Pts',(367.170127187901,-7.7949282622078,-1.42905415158391));
#42083=CARTESIAN_POINT('Ctrl Pts',(367.213786504066,-7.8009997803019,-1.54099956566681));
#42084=CARTESIAN_POINT('Ctrl Pts',(367.262615478618,-7.807071298396,-1.65103183515777));
#42085=CARTESIAN_POINT('Ctrl Pts',(367.316413133483,-7.81314281649011,-1.75864589466598));
#42086=CARTESIAN_POINT('Ctrl Pts',(367.368277795615,-7.81899618008686,-1.86239329501314));
#42087=CARTESIAN_POINT('Ctrl Pts',(367.424760025071,-7.82484954368361,-1.96389286992876));
#42088=CARTESIAN_POINT('Ctrl Pts',(367.485631165751,-7.83070290728036,-2.0627133754206));
#42089=CARTESIAN_POINT('Ctrl Pts',(367.546493166833,-7.83655539201427,-2.16151904334619));
#42090=CARTESIAN_POINT('Ctrl Pts',(367.611742552217,-7.84240787674818,-2.25764609000768));
#42091=CARTESIAN_POINT('Ctrl Pts',(367.681105897591,-7.84826036148209,-2.35068997591156));
#42092=CARTESIAN_POINT('Ctrl Pts',(367.750475602651,-7.85411338281026,-2.44374239269048));
#42093=CARTESIAN_POINT('Ctrl Pts',(367.823959770586,-7.85996640413844,-2.53371075551181));
#42094=CARTESIAN_POINT('Ctrl Pts',(367.901243474826,-7.86581942546662,-2.62022206898342));
#42095=CARTESIAN_POINT('Ctrl Pts',(367.978552954675,-7.87167439889044,-2.70676223564876));
#42096=CARTESIAN_POINT('Ctrl Pts',(368.059664215542,-7.87752937231427,-2.78984275234909));
#42097=CARTESIAN_POINT('Ctrl Pts',(368.144224628892,-7.88338434573809,-2.86912659957709));
#42098=CARTESIAN_POINT('Ctrl Pts',(368.228880880608,-7.88924595502225,-2.94850030486232));
#42099=CARTESIAN_POINT('Ctrl Pts',(368.31699378572,-7.89510756430641,-3.02406846933119));
#42100=CARTESIAN_POINT('Ctrl Pts',(368.408176642485,-7.90096917359057,-3.09553352841674));
#42101=CARTESIAN_POINT('Ctrl Pts',(368.499420984519,-7.90683473540091,-3.1670467769164));
#42102=CARTESIAN_POINT('Ctrl Pts',(368.593739064917,-7.91270029721125,-3.23445117118938));
#42103=CARTESIAN_POINT('Ctrl Pts',(368.690715590874,-7.91856585902159,-3.29749273552617));
#42104=CARTESIAN_POINT('Ctrl Pts',(368.787833920297,-7.92443999772192,-3.36062648209201));
#42105=CARTESIAN_POINT('Ctrl Pts',(368.887618098713,-7.93031413642226,-3.41938445795903));
#42106=CARTESIAN_POINT('Ctrl Pts',(368.989628625279,-7.93618827512259,-3.47355878780037));
#42107=CARTESIAN_POINT('Ctrl Pts',(369.015425422113,-7.93767374890381,-3.48725859141413));
#42108=CARTESIAN_POINT('Ctrl Pts',(369.041364498861,-7.93915922268503,-3.50066551228921));
#42109=CARTESIAN_POINT('Ctrl Pts',(369.067438566835,-7.94064469646626,-3.51377668432853));
#42110=CARTESIAN_POINT('Ctrl Pts',(369.170537644293,-7.94651838585683,-3.56561937120658));
#42111=CARTESIAN_POINT('Ctrl Pts',(369.276092070835,-7.95239207524741,-3.61300695171539));
#42112=CARTESIAN_POINT('Ctrl Pts',(369.383680024278,-7.95826576463798,-3.65569950751313));
#42113=CARTESIAN_POINT('Ctrl Pts',(369.491129071567,-7.96413187054375,-3.69833694321054));
#42114=CARTESIAN_POINT('Ctrl Pts',(369.600606044041,-7.96999797644951,-3.73629125797482));
#42115=CARTESIAN_POINT('Ctrl Pts',(369.711664962412,-7.97586408235528,-3.76936857931826));
#42116=CARTESIAN_POINT('Ctrl Pts',(369.822610157866,-7.98172418144332,-3.80241202990603));
#42117=CARTESIAN_POINT('Ctrl Pts',(369.935133683513,-7.98758428053137,-3.83058830328234));
#42118=CARTESIAN_POINT('Ctrl Pts',(370.048770661061,-7.99344437961942,-3.85375201704581));
#42119=CARTESIAN_POINT('Ctrl Pts',(370.16650740151,-7.99951589771352,-3.87775142475692));
#42120=CARTESIAN_POINT('Ctrl Pts',(370.285439032527,-8.00558741580763,-3.89636959407894));
#42121=CARTESIAN_POINT('Ctrl Pts',(370.405032191574,-8.01165893390173,-3.90950160771183));
#42122=CARTESIAN_POINT('Ctrl Pts',(370.52032827284,-8.01751229749849,-3.92216177760008));
#42123=CARTESIAN_POINT('Ctrl Pts',(370.63623871592,-8.02336566109525,-3.92972320188565));
#42124=CARTESIAN_POINT('Ctrl Pts',(370.752277186458,-8.02921902469201,-3.93214424061436));
#42125=CARTESIAN_POINT('Ctrl Pts',(370.86829823421,-8.03507150942593,-3.93456491583224));
#42126=CARTESIAN_POINT('Ctrl Pts',(370.984446858253,-8.04092399415985,-3.93184673152891));
#42127=CARTESIAN_POINT('Ctrl Pts',(371.100234894955,-8.04677647889376,-3.92400014359292));
#42128=CARTESIAN_POINT('Ctrl Pts',(371.216033547865,-8.05262950022194,-3.91615283623018));
#42129=CARTESIAN_POINT('Ctrl Pts',(371.331471135489,-8.05848252155013,-3.90317621844472));
#42130=CARTESIAN_POINT('Ctrl Pts',(371.446063502186,-8.06433554287831,-3.88513272115326));
#42131=CARTESIAN_POINT('Ctrl Pts',(371.56069408765,-8.07019051630214,-3.86708320600699));
#42132=CARTESIAN_POINT('Ctrl Pts',(371.67447848375,-8.07604548972597,-3.84396351528625));
#42133=CARTESIAN_POINT('Ctrl Pts',(371.786942327064,-8.08190046314981,-3.81588726403724));
#42134=CARTESIAN_POINT('Ctrl Pts',(371.899533633699,-8.08776207243397,-3.78777919196371));
#42135=CARTESIAN_POINT('Ctrl Pts',(372.010800999204,-8.09362368171813,-3.75470344704641));
#42136=CARTESIAN_POINT('Ctrl Pts',(372.120284743048,-8.0994852910023,-3.71682366521157));
#42137=CARTESIAN_POINT('Ctrl Pts',(372.229842312584,-8.10535085281265,-3.67891834076162));
#42138=CARTESIAN_POINT('Ctrl Pts',(372.337613482471,-8.11121641462301,-3.63620268088925));
#42139=CARTESIAN_POINT('Ctrl Pts',(372.44315970075,-8.11708197643337,-3.58888797674841));
#42140=CARTESIAN_POINT('Ctrl Pts',(372.548860253486,-8.12295611513371,-3.54150408690548));
#42141=CARTESIAN_POINT('Ctrl Pts',(372.652328993861,-8.12883025383405,-3.48950791632073));
#42142=CARTESIAN_POINT('Ctrl Pts',(372.753152985018,-8.13470439253439,-3.43315608980911));
#42143=CARTESIAN_POINT('Ctrl Pts',(372.778649726416,-8.13618986631557,-3.41890563283574));
#42144=CARTESIAN_POINT('Ctrl Pts',(372.803977487445,-8.13767534009675,-3.40437684241504));
#42145=CARTESIAN_POINT('Ctrl Pts',(372.829129908435,-8.13916081387793,-3.38957428955091));
#42146=CARTESIAN_POINT('Ctrl Pts',(372.928584715504,-8.14503450326849,-3.33104373935702));
#42147=CARTESIAN_POINT('Ctrl Pts',(373.025626929823,-8.15090819265906,-3.26803478452432));
#42148=CARTESIAN_POINT('Ctrl Pts',(373.119826272309,-8.15678188204962,-3.20077182352833));
#42149=CARTESIAN_POINT('Ctrl Pts',(373.213903994593,-8.16264798795536,-3.1335957053341));
#42150=CARTESIAN_POINT('Ctrl Pts',(373.30514581114,-8.1685140938611,-3.06217674129362));
#42151=CARTESIAN_POINT('Ctrl Pts',(373.39314703976,-8.17438019976685,-2.98678459118341));
#42152=CARTESIAN_POINT('Ctrl Pts',(373.481058156244,-8.18024029885488,-2.91146964167446));
#42153=CARTESIAN_POINT('Ctrl Pts',(373.565734973332,-8.18610039794291,-2.83218986585995));
#42154=CARTESIAN_POINT('Ctrl Pts',(373.646803310109,-8.19196049703093,-2.74925709143605));
#42155=CARTESIAN_POINT('Ctrl Pts',(373.73079640753,-8.19803201512504,-2.66333229171069));
#42156=CARTESIAN_POINT('Ctrl Pts',(373.810915369646,-8.20410353321915,-2.57348619555379));
#42157=CARTESIAN_POINT('Ctrl Pts',(373.886782892722,-8.21017505131326,-2.48011011502372));
#42158=CARTESIAN_POINT('Ctrl Pts',(373.959924435062,-8.21602841491001,-2.39008911169156));
#42159=CARTESIAN_POINT('Ctrl Pts',(374.029114512845,-8.22188177850675,-2.29678777682011));
#42160=CARTESIAN_POINT('Ctrl Pts',(374.094054489208,-8.22773514210349,-2.2005922075712));
#42161=CARTESIAN_POINT('Ctrl Pts',(374.158984715053,-8.23358762683738,-2.1044110817633));
#42162=CARTESIAN_POINT('Ctrl Pts',(374.219665877236,-8.23944011157128,-2.0053369279751));
#42163=CARTESIAN_POINT('Ctrl Pts',(374.275842123777,-8.24529259630518,-1.90378562217344));
#42164=CARTESIAN_POINT('Ctrl Pts',(374.332023520925,-8.25114561763334,-1.80222500548052));
#42165=CARTESIAN_POINT('Ctrl Pts',(374.383698981349,-8.25699863896151,-1.69818714681505));
#42166=CARTESIAN_POINT('Ctrl Pts',(374.43065850086,-8.26285166028968,-1.59211273035663));
#42167=CARTESIAN_POINT('Ctrl Pts',(374.477633682277,-8.26870663371349,-1.48600293603182));
#42168=CARTESIAN_POINT('Ctrl Pts',(374.519889628069,-8.2745616071373,-1.37785561086923));
#42169=CARTESIAN_POINT('Ctrl Pts',(374.557264652929,-8.28041658056112,-1.26813095797046));
#42170=CARTESIAN_POINT('Ctrl Pts',(374.59468203758,-8.28627818984526,-1.15828194627123));
#42171=CARTESIAN_POINT('Ctrl Pts',(374.627207326679,-8.29213979912941,-1.046852429996));
#42172=CARTESIAN_POINT('Ctrl Pts',(374.654728827592,-8.29800140841355,-0.934317390895616));
#42173=CARTESIAN_POINT('Ctrl Pts',(374.682268886454,-8.30386697022389,-0.821706468591917));
#42174=CARTESIAN_POINT('Ctrl Pts',(374.704798358474,-8.30973253203422,-0.707988943347631));
#42175=CARTESIAN_POINT('Ctrl Pts',(374.722257050076,-8.31559809384455,-0.59364787676059));
#42176=CARTESIAN_POINT('Ctrl Pts',(374.739741270567,-8.32147223254488,-0.479139615490211));
#42177=CARTESIAN_POINT('Ctrl Pts',(374.75213986865,-8.3273463712452,-0.364006402403479));
#42178=CARTESIAN_POINT('Ctrl Pts',(374.759444631172,-8.33322050994552,-0.248734350333146));
#42179=CARTESIAN_POINT('Ctrl Pts',(374.761291886363,-8.33470598372688,-0.219583930193503));
#42180=CARTESIAN_POINT('Ctrl Pts',(374.762813649909,-8.33619145750822,-0.190424618374459));
#42181=CARTESIAN_POINT('Ctrl Pts',(374.764010315222,-8.33767693128958,-0.161264236942478));
#42182=CARTESIAN_POINT('Ctrl Pts',(374.768742031421,-8.34355062068014,-0.0459616141751332));
#42183=CARTESIAN_POINT('Ctrl Pts',(374.768402619582,-8.34942431007071,0.069741473720703));
#42184=CARTESIAN_POINT('Ctrl Pts',(374.762947385123,-8.35529799946127,0.185361811307516));
#42185=CARTESIAN_POINT('Ctrl Pts',(374.757499193884,-8.36116410536702,0.300832872176412));
#42186=CARTESIAN_POINT('Ctrl Pts',(374.746948334513,-8.36703021127278,0.416220986286223));
#42187=CARTESIAN_POINT('Ctrl Pts',(374.731302022173,-8.37289631717853,0.531039910890018));
#42188=CARTESIAN_POINT('Ctrl Pts',(374.715671731458,-8.37875641626656,0.645741262377757));
#42189=CARTESIAN_POINT('Ctrl Pts',(374.694956421622,-8.3846165153546,0.759874176753556));
#42190=CARTESIAN_POINT('Ctrl Pts',(374.669215276891,-8.39047661444263,0.872955182096241));
#42191=CARTESIAN_POINT('Ctrl Pts',(374.642545450384,-8.39654813253674,0.99011589213267));
#42192=CARTESIAN_POINT('Ctrl Pts',(374.610480322117,-8.40261965063085,1.10614690796203));
#42193=CARTESIAN_POINT('Ctrl Pts',(374.573144174743,-8.40869116872496,1.22051904430707));
#42194=CARTESIAN_POINT('Ctrl Pts',(374.537149544982,-8.4145445323217,1.33078169838924));
#42195=CARTESIAN_POINT('Ctrl Pts',(374.496256300368,-8.42039789591845,1.43950220472217));
#42196=CARTESIAN_POINT('Ctrl Pts',(374.450626987493,-8.4262512595152,1.54622030946448));
#42197=CARTESIAN_POINT('Ctrl Pts',(374.405004525706,-8.4321037442491,1.65292239084248));
#42198=CARTESIAN_POINT('Ctrl Pts',(374.354647571982,-8.437956228983,1.75762228866674));
#42199=CARTESIAN_POINT('Ctrl Pts',(374.299766890365,-8.4438087137169,1.8598795581918));
#42200=CARTESIAN_POINT('Ctrl Pts',(374.244881176926,-8.44966173504508,1.96214620333555));
#42201=CARTESIAN_POINT('Ctrl Pts',(374.185471106465,-8.45551475637325,2.06196941092536));
#42202=CARTESIAN_POINT('Ctrl Pts',(374.121793144086,-8.46136777770143,2.15893381370774));
#42203=CARTESIAN_POINT('Ctrl Pts',(374.058093943877,-8.46722275112525,2.25593055599101));
#42204=CARTESIAN_POINT('Ctrl Pts',(373.990124247999,-8.47307772454907,2.3500662523921));
#42205=CARTESIAN_POINT('Ctrl Pts',(373.918183117588,-8.47893269797289,2.44095555700047));
#42206=CARTESIAN_POINT('Ctrl Pts',(373.846160451145,-8.48479430725704,2.5319478729613));
#42207=CARTESIAN_POINT('Ctrl Pts',(373.770157622778,-8.49065591654119,2.61968612920407));
#42208=CARTESIAN_POINT('Ctrl Pts',(373.690513213738,-8.49651752582534,2.70381897740561));
#42209=CARTESIAN_POINT('Ctrl Pts',(373.610815099888,-8.50238308763569,2.78800855700461));
#42210=CARTESIAN_POINT('Ctrl Pts',(373.52747081212,-8.50824864944603,2.86858760113921));
#42211=CARTESIAN_POINT('Ctrl Pts',(373.440853639376,-8.51411421125637,2.94524365639019));
#42212=CARTESIAN_POINT('Ctrl Pts',(373.354109811082,-8.5199883499567,3.02201180159505));
#42213=CARTESIAN_POINT('Ctrl Pts',(373.264083866595,-8.52586248865703,3.09484525070521));
#42214=CARTESIAN_POINT('Ctrl Pts',(373.171179837916,-8.53173662735736,3.16347357575554));
#42215=CARTESIAN_POINT('Ctrl Pts',(373.147685925732,-8.53322210113865,3.18082855879511));
#42216=CARTESIAN_POINT('Ctrl Pts',(373.124008089684,-8.53470757491995,3.19791484891524));
#42217=CARTESIAN_POINT('Ctrl Pts',(373.100153115988,-8.53619304870124,3.2147285362866));
#42218=CARTESIAN_POINT('Ctrl Pts',(373.005828525628,-8.54206673809182,3.2812112829856));
#42219=CARTESIAN_POINT('Ctrl Pts',(372.908418314537,-8.5479404274824,3.34364981695572));
#42220=CARTESIAN_POINT('Ctrl Pts',(372.808304303081,-8.55381411687297,3.40174462530341));
#42221=CARTESIAN_POINT('Ctrl Pts',(372.708319548219,-8.55968022277874,3.45976442779571));
#42222=CARTESIAN_POINT('Ctrl Pts',(372.605638289244,-8.5655463286845,3.51345145198771));
#42223=CARTESIAN_POINT('Ctrl Pts',(372.50067303116,-8.57141243459026,3.56254816402041));
#42224=CARTESIAN_POINT('Ctrl Pts',(372.395815256163,-8.57727253367831,3.61159460164546));
#42225=CARTESIAN_POINT('Ctrl Pts',(372.288678506103,-8.58313263276635,3.65605990263535));
#42226=CARTESIAN_POINT('Ctrl Pts',(372.179701130561,-8.5889927318544,3.69573170523268));
#42227=CARTESIAN_POINT('Ctrl Pts',(372.066792099926,-8.5950642499485,3.73683477596177));
#42228=CARTESIAN_POINT('Ctrl Pts',(371.951907515801,-8.60113576804261,3.77279171431096));
#42229=CARTESIAN_POINT('Ctrl Pts',(371.835559431533,-8.60720728613671,3.80342007959487));
#42230=CARTESIAN_POINT('Ctrl Pts',(371.723391826915,-8.61306064973347,3.83294794323661));
#42231=CARTESIAN_POINT('Ctrl Pts',(371.60986451545,-8.61891401333023,3.85752344941456));
#42232=CARTESIAN_POINT('Ctrl Pts',(371.495452370106,-8.62476737692699,3.87703367932076));
#42233=CARTESIAN_POINT('Ctrl Pts',(371.38105740336,-8.6306198616609,3.89654097983159));
#42234=CARTESIAN_POINT('Ctrl Pts',(371.265778274057,-8.63647234639481,3.91098444686756));
#42235=CARTESIAN_POINT('Ctrl Pts',(371.150099348566,-8.64232483112872,3.92030241782435));
#42236=CARTESIAN_POINT('Ctrl Pts',(371.034409816871,-8.6481778524569,3.92962124311395));
#42237=CARTESIAN_POINT('Ctrl Pts',(370.918320827953,-8.65403087378508,3.93381360495592));
#42238=CARTESIAN_POINT('Ctrl Pts',(370.802320450348,-8.65988389511326,3.93286983845248));
#42239=CARTESIAN_POINT('Ctrl Pts',(370.686281384377,-8.66573886853708,3.93192575718468));
#42240=CARTESIAN_POINT('Ctrl Pts',(370.570331401394,-8.67159384196091,3.92584214471076));
#42241=CARTESIAN_POINT('Ctrl Pts',(370.454956434475,-8.67744881538473,3.91466140476607));
#42242=CARTESIAN_POINT('Ctrl Pts',(370.339450704851,-8.68331042466889,3.90346799288874));
#42243=CARTESIAN_POINT('Ctrl Pts',(370.224521703509,-8.68917203395306,3.88716596299029));
#42244=CARTESIAN_POINT('Ctrl Pts',(370.110648219318,-8.69503364323723,3.86584935828623));
#42245=CARTESIAN_POINT('Ctrl Pts',(369.9966979494,-8.70089920504758,3.84451837963907));
#42246=CARTESIAN_POINT('Ctrl Pts',(369.883805015206,-8.70676476685793,3.81816618682113));
#42247=CARTESIAN_POINT('Ctrl Pts',(369.772434337282,-8.71263032866828,3.78693707348965));
#42248=CARTESIAN_POINT('Ctrl Pts',(369.660900808111,-8.71850446736863,3.75566229553502));
#42249=CARTESIAN_POINT('Ctrl Pts',(369.55089436854,-8.72437860606897,3.71949649341231));
#42250=CARTESIAN_POINT('Ctrl Pts',(369.442861290902,-8.73025274476931,3.67863257681035));
#42251=CARTESIAN_POINT('Ctrl Pts',(369.415541489222,-8.73173821855051,3.6682987594108));
#42252=CARTESIAN_POINT('Ctrl Pts',(369.388347765434,-8.7332236923317,3.65766472835756));
#42253=CARTESIAN_POINT('Ctrl Pts',(369.361287083872,-8.73470916611289,3.64673406660575));
#42254=CARTESIAN_POINT('Ctrl Pts',(369.254286852561,-8.74058285550345,3.60351330244529));
#42255=CARTESIAN_POINT('Ctrl Pts',(369.149012260597,-8.74645654489401,3.55550726078663));
#42256=CARTESIAN_POINT('Ctrl Pts',(369.045921979465,-8.75233023428457,3.50287441949075));
#42257=CARTESIAN_POINT('Ctrl Pts',(368.942964797571,-8.75819634019032,3.45030953213762));
#42258=CARTESIAN_POINT('Ctrl Pts',(368.842186682757,-8.76406244609607,3.39312991089222));
#42259=CARTESIAN_POINT('Ctrl Pts',(368.744027665632,-8.76992855200182,3.33154257539275));
#42260=CARTESIAN_POINT('Ctrl Pts',(368.645969162089,-8.77578865108985,3.27001830454031));
#42261=CARTESIAN_POINT('Ctrl Pts',(368.550524769553,-8.78164875017787,3.20409551531753));
#42262=CARTESIAN_POINT('Ctrl Pts',(368.458110570752,-8.7875088492659,3.13402743298867));
#42263=CARTESIAN_POINT('Ctrl Pts',(368.362362278488,-8.79358036736001,3.06143145410011));
#42264=CARTESIAN_POINT('Ctrl Pts',(368.269867355309,-8.79965188545412,2.98438563480252));
#42265=CARTESIAN_POINT('Ctrl Pts',(368.181056696544,-8.80572340354823,2.90322135471163));
#42266=CARTESIAN_POINT('Ctrl Pts',(368.095437075725,-8.81157676714497,2.82497337206943));
#42267=CARTESIAN_POINT('Ctrl Pts',(368.01324184973,-8.81743013074171,2.7428980970104));
#42268=CARTESIAN_POINT('Ctrl Pts',(367.934823338273,-8.82328349433845,2.65733335465643));
#42269=CARTESIAN_POINT('Ctrl Pts',(367.856416601092,-8.82913597907235,2.57178145956058));
#42270=CARTESIAN_POINT('Ctrl Pts',(367.781785729985,-8.83498846380625,2.48274144344072));
#42271=CARTESIAN_POINT('Ctrl Pts',(367.711245120138,-8.84084094854014,2.39058689527376));
#42272=CARTESIAN_POINT('Ctrl Pts',(367.640698042664,-8.84669396986833,2.29842389777182));
#42273=CARTESIAN_POINT('Ctrl Pts',(367.574242223094,-8.85254699119651,2.2031461286382));
#42274=CARTESIAN_POINT('Ctrl Pts',(367.512150369513,-8.85840001252469,2.1051584762604));
#42275=CARTESIAN_POINT('Ctrl Pts',(367.450037807099,-8.86425498594849,2.00713814310867));
#42276=CARTESIAN_POINT('Ctrl Pts',(367.392292325824,-8.87010995937229,1.90640647834122));
#42277=CARTESIAN_POINT('Ctrl Pts',(367.339141722438,-8.87596493279609,1.80339480280505));
#42278=CARTESIAN_POINT('Ctrl Pts',(367.28593087967,-8.88182654208024,1.70026637676576));
#42279=CARTESIAN_POINT('Ctrl Pts',(367.237325498601,-8.88768815136438,1.59485314960982));
#42280=CARTESIAN_POINT('Ctrl Pts',(367.193506109978,-8.89354976064853,1.48760843310357));
#42281=CARTESIAN_POINT('Ctrl Pts',(367.149657173619,-8.89941532245886,1.38029140069752));
#42282=CARTESIAN_POINT('Ctrl Pts',(367.110600794683,-8.90528088426918,1.27114080783832));
#42283=CARTESIAN_POINT('Ctrl Pts',(367.076467759926,-8.91114644607951,1.16062555387311));
#42284=CARTESIAN_POINT('Ctrl Pts',(367.042284814301,-8.91702058477984,1.04994869950075));
#42285=CARTESIAN_POINT('Ctrl Pts',(367.013039684462,-8.92289472348017,0.937903599782908));
#42286=CARTESIAN_POINT('Ctrl Pts',(366.988812195358,-8.9287688621805,0.824969839038923));
#42287=CARTESIAN_POINT('Ctrl Pts',(366.982685458881,-8.93025433596185,0.796410734602832));
#42288=CARTESIAN_POINT('Ctrl Pts',(366.976879342316,-8.9317398097432,0.767794825732123));
#42289=CARTESIAN_POINT('Ctrl Pts',(366.971394610312,-8.93322528352455,0.739129906964237));
#42290=CARTESIAN_POINT('Ctrl Pts',(366.939445662096,-8.9418782723808,0.57215474673101));
#42291=CARTESIAN_POINT('Ctrl Pts',(366.918315437461,-8.95053126123704,0.40304846186944));
#42292=CARTESIAN_POINT('Ctrl Pts',(366.908222919179,-8.95918425009329,0.232954005898987));
#42293=CARTESIAN_POINT('Ctrl Pts',(366.903692680176,-8.96306832605054,0.156603533493056));
#42294=CARTESIAN_POINT('Ctrl Pts',(366.901385817882,-8.9669524020078,0.08005428134596));
#42295=CARTESIAN_POINT('Ctrl Pts',(366.901319333012,-8.97083647796505,0.00341174640567556));
#42296=CARTESIAN_POINT('',(366.901317864546,-10.2208364779364,0.000298426845041825));
#42297=CARTESIAN_POINT('Ctrl Pts',(366.901319333012,-8.9708364780123,0.00341174547327817));
#42298=CARTESIAN_POINT('Ctrl Pts',(366.901220434153,-8.97661419535868,-0.110597071159494));
#42299=CARTESIAN_POINT('Ctrl Pts',(366.906083007808,-8.98239191270507,-0.224772387134529));
#42300=CARTESIAN_POINT('Ctrl Pts',(366.915923782789,-8.98816963005145,-0.338639792082648));
#42301=CARTESIAN_POINT('Ctrl Pts',(366.926112765496,-8.99415178717165,-0.45653630145333));
#42302=CARTESIAN_POINT('Ctrl Pts',(366.941638841141,-9.00013394429185,-0.57410224769329));
#42303=CARTESIAN_POINT('Ctrl Pts',(366.962461634196,-9.00611610141205,-0.690809973273278));
#42304=CARTESIAN_POINT('Ctrl Pts',(366.982542839518,-9.0118852086149,-0.803361243115248));
#42305=CARTESIAN_POINT('Ctrl Pts',(367.007549840669,-9.01765431581776,-0.915113919845186));
#42306=CARTESIAN_POINT('Ctrl Pts',(367.037393713836,-9.02342342302062,-1.0256003508848));
#42307=CARTESIAN_POINT('Ctrl Pts',(367.067229917836,-9.02919104769962,-1.1360583895296));
#42308=CARTESIAN_POINT('Ctrl Pts',(367.101900412987,-9.03495867237862,-1.24525041765691));
#42309=CARTESIAN_POINT('Ctrl Pts',(367.141265616119,-9.04072629705762,-1.35272102593688));
#42310=CARTESIAN_POINT('Ctrl Pts',(367.180630876692,-9.04649393015267,-1.46019179103654));
#42311=CARTESIAN_POINT('Ctrl Pts',(367.224690711424,-9.05226156324771,-1.56594073115193));
#42312=CARTESIAN_POINT('Ctrl Pts',(367.273256621578,-9.05802919634276,-1.66953044430808));
#42313=CARTESIAN_POINT('Ctrl Pts',(367.321835155203,-9.06379832858696,-1.77314708296887));
#42314=CARTESIAN_POINT('Ctrl Pts',(367.37492190967,-9.06956746083117,-1.8746029939876));
#42315=CARTESIAN_POINT('Ctrl Pts',(367.432281886025,-9.07533659307538,-1.97348429886904));
#42316=CARTESIAN_POINT('Ctrl Pts',(367.489703183547,-9.08111189285922,-2.07247131364609));
#42317=CARTESIAN_POINT('Ctrl Pts',(367.551406604029,-9.08688719264307,-2.16887786140994));
#42318=CARTESIAN_POINT('Ctrl Pts',(367.617113228884,-9.09266249242691,-2.262318148521));
#42319=CARTESIAN_POINT('Ctrl Pts',(367.682861813838,-9.09844148030378,-2.3558181063823));
#42320=CARTESIAN_POINT('Ctrl Pts',(367.752618429645,-9.10422046818064,-2.44634769830393));
#42321=CARTESIAN_POINT('Ctrl Pts',(367.8260644028,-9.10999945605751,-2.53355485001079));
#42322=CARTESIAN_POINT('Ctrl Pts',(367.899616566023,-9.11578679934301,-2.62088808805033));
#42323=CARTESIAN_POINT('Ctrl Pts',(367.976868439654,-9.12157414262851,-2.70488899160559));
#42324=CARTESIAN_POINT('Ctrl Pts',(368.057465231478,-9.127361485914,-2.78524299067516));
#42325=CARTESIAN_POINT('Ctrl Pts',(368.077797364424,-9.12882145758807,-2.80551387435225));
#42326=CARTESIAN_POINT('Ctrl Pts',(368.098342209705,-9.13028142926214,-2.8255528739549));
#42327=CARTESIAN_POINT('Ctrl Pts',(368.11909376202,-9.13174140093621,-2.84535536173312));
#42328=CARTESIAN_POINT('Ctrl Pts',(368.202580431545,-9.13761509032677,-2.92502379944022));
#42329=CARTESIAN_POINT('Ctrl Pts',(368.289715492768,-9.14348877971733,-3.00114738878479));
#42330=CARTESIAN_POINT('Ctrl Pts',(368.380165479798,-9.1493624691079,-3.07337357443067));
#42331=CARTESIAN_POINT('Ctrl Pts',(368.470498687398,-9.15522857501364,-3.14550650928551));
#42332=CARTESIAN_POINT('Ctrl Pts',(368.564137989628,-9.16109468091939,-3.21375179182564));
#42333=CARTESIAN_POINT('Ctrl Pts',(368.660713379682,-9.16696078682514,-3.27779386060144));
#42334=CARTESIAN_POINT('Ctrl Pts',(368.757189877765,-9.17282088591317,-3.3417703511146));
#42335=CARTESIAN_POINT('Ctrl Pts',(368.856596141189,-9.1786809850012,-3.4015519619796));
#42336=CARTESIAN_POINT('Ctrl Pts',(368.958529938369,-9.18454108408922,-3.45686399768413));
#42337=CARTESIAN_POINT('Ctrl Pts',(369.064141274403,-9.19061260218333,-3.51417156545006));
#42338=CARTESIAN_POINT('Ctrl Pts',(369.172465609875,-9.19668412027744,-3.56668068303703));
#42339=CARTESIAN_POINT('Ctrl Pts',(369.283023402244,-9.20275563837155,-3.6141353774254));
#42340=CARTESIAN_POINT('Ctrl Pts',(369.389608764777,-9.20860900196829,-3.65988498671947));
#42341=CARTESIAN_POINT('Ctrl Pts',(369.498269434401,-9.21446236556504,-3.70093696388293));
#42342=CARTESIAN_POINT('Ctrl Pts',(369.608552387805,-9.22031572916178,-3.73710958145271));
#42343=CARTESIAN_POINT('Ctrl Pts',(369.718818782594,-9.22616821389568,-3.77327676782572));
#42344=CARTESIAN_POINT('Ctrl Pts',(369.83070658437,-9.23202069862958,-3.80456592260076));
#42345=CARTESIAN_POINT('Ctrl Pts',(369.943745819968,-9.23787318336348,-3.83084461360448));
#42346=CARTESIAN_POINT('Ctrl Pts',(370.056795419746,-9.24372620469165,-3.85712571401131));
#42347=CARTESIAN_POINT('Ctrl Pts',(370.170996260775,-9.24957922601982,-3.87839534386206));
#42348=CARTESIAN_POINT('Ctrl Pts',(370.285867038557,-9.25543224734799,-3.89457195387263));
#42349=CARTESIAN_POINT('Ctrl Pts',(370.400776127962,-9.26128722077182,-3.91075395909506));
#42350=CARTESIAN_POINT('Ctrl Pts',(370.516355189526,-9.26714219419565,-3.92183950926494));
#42351=CARTESIAN_POINT('Ctrl Pts',(370.63211735073,-9.27299716761947,-3.92779886918755));
#42352=CARTESIAN_POINT('Ctrl Pts',(370.748010713473,-9.27885877690362,-3.93376498327918));
#42353=CARTESIAN_POINT('Ctrl Pts',(370.864087177224,-9.28472038618776,-3.93459328970434));
#42354=CARTESIAN_POINT('Ctrl Pts',(370.979859318703,-9.29058199547191,-3.93030618168944));
#42355=CARTESIAN_POINT('Ctrl Pts',(371.095709526187,-9.29644755728224,-3.92601618284613));
#42356=CARTESIAN_POINT('Ctrl Pts',(371.211254592026,-9.30231311909258,-3.91660393457928));
#42357=CARTESIAN_POINT('Ctrl Pts',(371.326013397635,-9.30817868090291,-3.90214357649817));
#42358=CARTESIAN_POINT('Ctrl Pts',(371.440940008765,-9.31405281960324,-3.88766207382687));
#42359=CARTESIAN_POINT('Ctrl Pts',(371.55507765949,-9.31992695830357,-3.86811779903549));
#42360=CARTESIAN_POINT('Ctrl Pts',(371.667956504604,-9.3258010970039,-3.8436357266169));
#42361=CARTESIAN_POINT('Ctrl Pts',(371.696501721773,-9.32728657078522,-3.83744461017491));
#42362=CARTESIAN_POINT('Ctrl Pts',(371.72496652159,-9.32877204456654,-3.8309379673117));
#42363=CARTESIAN_POINT('Ctrl Pts',(371.753343487414,-9.33025751834786,-3.82411831455329));
#42364=CARTESIAN_POINT('Ctrl Pts',(371.865548418386,-9.33613120773843,-3.79715282882194));
#42365=CARTESIAN_POINT('Ctrl Pts',(371.976752413301,-9.342004897129,-3.76519987490544));
#42366=CARTESIAN_POINT('Ctrl Pts',(372.086478442113,-9.34787858651956,-3.728348543207));
#42367=CARTESIAN_POINT('Ctrl Pts',(372.196062804313,-9.35374469242532,-3.69154479003982));
#42368=CARTESIAN_POINT('Ctrl Pts',(372.30417260711,-9.35961079833107,-3.64985536631478));
#42369=CARTESIAN_POINT('Ctrl Pts',(372.41034209753,-9.36547690423682,-3.60342012279424));
#42370=CARTESIAN_POINT('Ctrl Pts',(372.516402871746,-9.37133700332487,-3.5570324283714));
#42371=CARTESIAN_POINT('Ctrl Pts',(372.62052690933,-9.37719710241292,-3.50590874498824));
#42372=CARTESIAN_POINT('Ctrl Pts',(372.722265327923,-9.38305720150097,-3.45023815595081));
#42373=CARTESIAN_POINT('Ctrl Pts',(372.827674236555,-9.38912871959508,-3.392559099066));
#42374=CARTESIAN_POINT('Ctrl Pts',(372.930521712646,-9.39520023768918,-3.32999900198444));
#42375=CARTESIAN_POINT('Ctrl Pts',(373.030332695486,-9.40127175578329,-3.26282206265745));
#42376=CARTESIAN_POINT('Ctrl Pts',(373.126557389946,-9.40712511938004,-3.19805884444691));
#42377=CARTESIAN_POINT('Ctrl Pts',(373.219959670976,-9.4129784829768,-3.12900509834453));
#42378=CARTESIAN_POINT('Ctrl Pts',(373.310141243316,-9.41883184657355,-3.05594298720925));
#42379=CARTESIAN_POINT('Ctrl Pts',(373.400309275196,-9.42468433130745,-2.98289184610411));
#42380=CARTESIAN_POINT('Ctrl Pts',(373.487257238995,-9.43053681604136,-2.90583379665994));
#42381=CARTESIAN_POINT('Ctrl Pts',(373.570619073994,-9.43638930077526,-2.82509196827481));
#42382=CARTESIAN_POINT('Ctrl Pts',(373.653988552155,-9.44224232210342,-2.74434273694828));
#42383=CARTESIAN_POINT('Ctrl Pts',(373.733770951112,-9.44809534343159,-2.65990934271192));
#42384=CARTESIAN_POINT('Ctrl Pts',(373.809636824618,-9.45394836475975,-2.57215202086995));
#42385=CARTESIAN_POINT('Ctrl Pts',(373.885528000857,-9.45980333818357,-2.4843654302663));
#42386=CARTESIAN_POINT('Ctrl Pts',(373.957499784203,-9.46565831160738,-2.39325302004316));
#42387=CARTESIAN_POINT('Ctrl Pts',(374.025263249713,-9.4715132850312,-2.2992077932684));
#42388=CARTESIAN_POINT('Ctrl Pts',(374.093103516408,-9.47737489431535,-2.20505597830862));
#42389=CARTESIAN_POINT('Ctrl Pts',(374.1567257038,-9.4832365035995,-2.10796504773429));
#42390=CARTESIAN_POINT('Ctrl Pts',(374.215884392299,-9.48909811288366,-2.00835672673192));
#42391=CARTESIAN_POINT('Ctrl Pts',(374.275082971936,-9.49496367469401,-1.90868123910711));
#42392=CARTESIAN_POINT('Ctrl Pts',(374.329811864999,-9.50082923650436,-1.80648534427119));
#42393=CARTESIAN_POINT('Ctrl Pts',(374.379872552623,-9.5066947983147,-1.70221352173318));
#42394=CARTESIAN_POINT('Ctrl Pts',(374.43000644125,-9.51256893701503,-1.59778922821634));
#42395=CARTESIAN_POINT('Ctrl Pts',(374.475458339797,-9.51844307571537,-1.49128332740049));
#42396=CARTESIAN_POINT('Ctrl Pts',(374.516078557755,-9.5243172144157,-1.38315838376092));
#42397=CARTESIAN_POINT('Ctrl Pts',(374.526350747747,-9.52580268819698,-1.35581535066756));
#42398=CARTESIAN_POINT('Ctrl Pts',(374.5363142034,-9.52728816197824,-1.32836884303156));
#42399=CARTESIAN_POINT('Ctrl Pts',(374.545967018738,-9.52877363575952,-1.30082645734895));
#42400=CARTESIAN_POINT('Ctrl Pts',(374.584135069736,-9.53464732515008,-1.19192152707408));
#42401=CARTESIAN_POINT('Ctrl Pts',(374.617569495124,-9.54052101454064,-1.08115393728371));
#42402=CARTESIAN_POINT('Ctrl Pts',(374.646086555742,-9.5463947039312,-0.968972836823832));
#42403=CARTESIAN_POINT('Ctrl Pts',(374.674566798156,-9.55226080983695,-0.856936572703568));
#42404=CARTESIAN_POINT('Ctrl Pts',(374.698142200584,-9.5581269157427,-0.743490823943879));
#42405=CARTESIAN_POINT('Ctrl Pts',(374.716677791602,-9.56399302164845,-0.629102780851182));
#42406=CARTESIAN_POINT('Ctrl Pts',(374.735194402412,-9.56985312073649,-0.514831869657354));
#42407=CARTESIAN_POINT('Ctrl Pts',(374.748681401187,-9.57571321982452,-0.399620988792879));
#42408=CARTESIAN_POINT('Ctrl Pts',(374.757054332714,-9.58157331891256,-0.28394984148724));
#42409=CARTESIAN_POINT('Ctrl Pts',(374.765729340509,-9.58764483700666,-0.164105543074864));
#42410=CARTESIAN_POINT('Ctrl Pts',(374.768914194981,-9.59371635510078,-0.0437675782129017));
#42411=CARTESIAN_POINT('Ctrl Pts',(374.766573368814,-9.59978787319488,0.0765216316346329));
#42412=CARTESIAN_POINT('Ctrl Pts',(374.764316650403,-9.60564123679164,0.192488754039612));
#42413=CARTESIAN_POINT('Ctrl Pts',(374.75692451057,-9.61149460038838,0.308410116268769));
#42414=CARTESIAN_POINT('Ctrl Pts',(374.744418133333,-9.61734796398514,0.423798064520112));
#42415=CARTESIAN_POINT('Ctrl Pts',(374.731913633886,-9.62320044871903,0.539168687659114));
#42416=CARTESIAN_POINT('Ctrl Pts',(374.714296468386,-9.62905293345293,0.654005645440778));
#42417=CARTESIAN_POINT('Ctrl Pts',(374.691639720005,-9.63490541818682,0.767826162651834));
#42418=CARTESIAN_POINT('Ctrl Pts',(374.668980894304,-9.64075843951499,0.881657115676215));
#42419=CARTESIAN_POINT('Ctrl Pts',(374.641281647847,-9.64661146084317,0.99447103765158));
#42420=CARTESIAN_POINT('Ctrl Pts',(374.608666093242,-9.65246448217134,1.10579580532458));
#42421=CARTESIAN_POINT('Ctrl Pts',(374.576039660719,-9.65831945559515,1.21715770195731));
#42422=CARTESIAN_POINT('Ctrl Pts',(374.538493775707,-9.66417442901895,1.32702906043275));
#42423=CARTESIAN_POINT('Ctrl Pts',(374.496202052808,-9.67002940244276,1.43495404415433));
#42424=CARTESIAN_POINT('Ctrl Pts',(374.453862397674,-9.67589101172692,1.54300134698282));
#42425=CARTESIAN_POINT('Ctrl Pts',(374.406766319716,-9.68175262101108,1.64909748720203));
#42426=CARTESIAN_POINT('Ctrl Pts',(374.355135153625,-9.68761423029524,1.75280761556911));
#42427=CARTESIAN_POINT('Ctrl Pts',(374.303469172259,-9.69347979210557,1.85658767643717));
#42428=CARTESIAN_POINT('Ctrl Pts',(374.247262213333,-9.6993453539159,1.95797816132318));
#42429=CARTESIAN_POINT('Ctrl Pts',(374.186780157501,-9.70521091572624,2.05657129669788));
#42430=CARTESIAN_POINT('Ctrl Pts',(374.126209662069,-9.71108505442656,2.15530859941809));
#42431=CARTESIAN_POINT('Ctrl Pts',(374.061351824335,-9.71695919312688,2.25124004824819));
#42432=CARTESIAN_POINT('Ctrl Pts',(373.992514192211,-9.72283333182721,2.34398909647804));
#42433=CARTESIAN_POINT('Ctrl Pts',(373.975106278829,-9.72431880560853,2.36744381663647));
#42434=CARTESIAN_POINT('Ctrl Pts',(373.957444047156,-9.72580427938985,2.39069519944109));
#42435=CARTESIAN_POINT('Ctrl Pts',(373.939532847338,-9.72728975317117,2.41373752515246));
#42436=CARTESIAN_POINT('Ctrl Pts',(373.868710443291,-9.73316344256175,2.50484883641686));
#42437=CARTESIAN_POINT('Ctrl Pts',(373.793756688372,-9.73903713195232,2.59299221037434));
#42438=CARTESIAN_POINT('Ctrl Pts',(373.714949399135,-9.7449108213429,2.67776976170557));
#42439=CARTESIAN_POINT('Ctrl Pts',(373.636243857511,-9.75077692724865,2.76243785725346));
#42440=CARTESIAN_POINT('Ctrl Pts',(373.553694954478,-9.75664303315441,2.84374847230078));
#42441=CARTESIAN_POINT('Ctrl Pts',(373.467622104424,-9.76250913906017,2.92133492099278));
#42442=CARTESIAN_POINT('Ctrl Pts',(373.381637391872,-9.76836923814823,2.99884192214994));
#42443=CARTESIAN_POINT('Ctrl Pts',(373.292136214908,-9.77422933723629,3.07263206734381));
#42444=CARTESIAN_POINT('Ctrl Pts',(373.199475887948,-9.78008943632435,3.1423743365141));
#42445=CARTESIAN_POINT('Ctrl Pts',(373.103472587783,-9.78616095441845,3.21463274764817));
#42446=CARTESIAN_POINT('Ctrl Pts',(373.004078191493,-9.79223247251256,3.28254536114066));
#42447=CARTESIAN_POINT('Ctrl Pts',(372.901729240396,-9.79830399060666,3.34578827127365));
#42448=CARTESIAN_POINT('Ctrl Pts',(372.803057768906,-9.80415735420342,3.40675881310319));
#42449=CARTESIAN_POINT('Ctrl Pts',(372.701640789256,-9.81001071780017,3.46338921298782));
#42450=CARTESIAN_POINT('Ctrl Pts',(372.597899564819,-9.81586408139693,3.51543291025817));
#42451=CARTESIAN_POINT('Ctrl Pts',(372.494173916778,-9.82171656613084,3.56746879334252));
#42452=CARTESIAN_POINT('Ctrl Pts',(372.38812508703,-9.82756905086475,3.61491915795601));
#42453=CARTESIAN_POINT('Ctrl Pts',(372.280198374458,-9.83342153559866,3.65758369942712));
#42454=CARTESIAN_POINT('Ctrl Pts',(372.172261766456,-9.83927455692684,3.70025215266382));
#42455=CARTESIAN_POINT('Ctrl Pts',(372.062447317594,-9.84512757825502,3.73813375858133));
#42456=CARTESIAN_POINT('Ctrl Pts',(371.951219039372,-9.8509805995832,3.77107686747186));
#42457=CARTESIAN_POINT('Ctrl Pts',(371.839953664371,-9.85683557300702,3.80403096352541));
#42458=CARTESIAN_POINT('Ctrl Pts',(371.727273918296,-9.86269054643084,3.83204317013627));
#42459=CARTESIAN_POINT('Ctrl Pts',(371.613656962345,-9.86854551985467,3.85501226366336));
#42460=CARTESIAN_POINT('Ctrl Pts',(371.499911236167,-9.87440712913882,3.87800738970768));
#42461=CARTESIAN_POINT('Ctrl Pts',(371.385226585191,-9.88026873842297,3.89594791252142));
#42462=CARTESIAN_POINT('Ctrl Pts',(371.270088404287,-9.88613034770712,3.90878408547029));
#42463=CARTESIAN_POINT('Ctrl Pts',(371.154872584862,-9.89199590951749,3.9216289139449));
#42464=CARTESIAN_POINT('Ctrl Pts',(371.039203037761,-9.89786147132785,3.92936251147408));
#42465=CARTESIAN_POINT('Ctrl Pts',(370.923566554713,-9.90372703313821,3.93198724174972));
#42466=CARTESIAN_POINT('Ctrl Pts',(370.807760982765,-9.90960117183855,3.93461581002477));
#42467=CARTESIAN_POINT('Ctrl Pts',(370.69198898282,-9.9154753105389,3.93212061084011));
#42468=CARTESIAN_POINT('Ctrl Pts',(370.576733694681,-9.92134944923924,3.92455594956524));
#42469=CARTESIAN_POINT('Ctrl Pts',(370.547587513869,-9.92283492302045,3.92264297022295));
#42470=CARTESIAN_POINT('Ctrl Pts',(370.518474330667,-9.92432039680165,3.92040605411119));
#42471=CARTESIAN_POINT('Ctrl Pts',(370.489401851781,-9.92580587058285,3.91784659627567));
#42472=CARTESIAN_POINT('Ctrl Pts',(370.374446803131,-9.93167955997341,3.90772628279431));
#42473=CARTESIAN_POINT('Ctrl Pts',(370.259746090888,-9.93755324936398,3.89252541571314));
#42474=CARTESIAN_POINT('Ctrl Pts',(370.145784668205,-9.94342693875455,3.87226174904637));
#42475=CARTESIAN_POINT('Ctrl Pts',(370.031970380425,-9.94929304466028,3.85202424467705));
#42476=CARTESIAN_POINT('Ctrl Pts',(369.918893887083,-9.955159150566,3.82673701144358));
#42477=CARTESIAN_POINT('Ctrl Pts',(369.807036474757,-9.96102525647173,3.79646967187357));
#42478=CARTESIAN_POINT('Ctrl Pts',(369.695293602997,-9.96688535555974,3.76623332567367));
#42479=CARTESIAN_POINT('Ctrl Pts',(369.584767725666,-9.97274545464776,3.7310271238657));
#42480=CARTESIAN_POINT('Ctrl Pts',(369.475930705063,-9.97860555373578,3.6909718714331));
#42481=CARTESIAN_POINT('Ctrl Pts',(369.363167093052,-9.98467707182989,3.64947151687319));
#42482=CARTESIAN_POINT('Ctrl Pts',(369.252216943441,-9.99074858992401,3.60276569939484));
#42483=CARTESIAN_POINT('Ctrl Pts',(369.143589089944,-9.99682010801812,3.55104565572135));
#42484=CARTESIAN_POINT('Ctrl Pts',(369.038864322037,-10.0026734716149,3.50118395455078));
#42485=CARTESIAN_POINT('Ctrl Pts',(368.936298243377,-10.0085268352116,3.44666234910111));
#42486=CARTESIAN_POINT('Ctrl Pts',(368.836326411713,-10.0143801988084,3.38770116740654));
#42487=CARTESIAN_POINT('Ctrl Pts',(368.736369590482,-10.0202326835422,3.32874883853505));
#42488=CARTESIAN_POINT('Ctrl Pts',(368.639006597507,-10.0260851682761,3.26535846866901));
#42489=CARTESIAN_POINT('Ctrl Pts',(368.544647151135,-10.03193765301,3.19779565888662));
#42490=CARTESIAN_POINT('Ctrl Pts',(368.450279053268,-10.0377906743382,3.13022665450154));
#42491=CARTESIAN_POINT('Ctrl Pts',(368.358915385376,-10.0436436956664,3.05848469024652));
#42492=CARTESIAN_POINT('Ctrl Pts',(368.270935124946,-10.0494967169946,2.98287746787704));
#42493=CARTESIAN_POINT('Ctrl Pts',(368.182925521401,-10.0553516904184,2.90724502903869));
#42494=CARTESIAN_POINT('Ctrl Pts',(368.098301882323,-10.0612066638422,2.82774503781916));
#42495=CARTESIAN_POINT('Ctrl Pts',(368.017407940355,-10.0670616372661,2.74472358221788));
#42496=CARTESIAN_POINT('Ctrl Pts',(367.936422315496,-10.0729232465502,2.66160803246076));
#42497=CARTESIAN_POINT('Ctrl Pts',(367.859175113332,-10.0787848558343,2.57496334834159));
#42498=CARTESIAN_POINT('Ctrl Pts',(367.785971273526,-10.0846464651185,2.48517044285603));
#42499=CARTESIAN_POINT('Ctrl Pts',(367.712718071834,-10.0905120269288,2.39531698935458));
#42500=CARTESIAN_POINT('Ctrl Pts',(367.643513907526,-10.0963775887392,2.30231141801826));
#42501=CARTESIAN_POINT('Ctrl Pts',(367.578620688798,-10.1022431505495,2.20656406513605));
#42502=CARTESIAN_POINT('Ctrl Pts',(367.513632580269,-10.1081172892499,2.11067670614044));
#42503=CARTESIAN_POINT('Ctrl Pts',(367.452968213445,-10.1139914279502,2.01203991489076));
#42504=CARTESIAN_POINT('Ctrl Pts',(367.396843869782,-10.1198655666505,1.91108911701175));
#42505=CARTESIAN_POINT('Ctrl Pts',(367.382650939506,-10.1213510404318,1.88556030826137));
#42506=CARTESIAN_POINT('Ctrl Pts',(367.368748104157,-10.1228365142132,1.85988361845735));
#42507=CARTESIAN_POINT('Ctrl Pts',(367.355138369347,-10.1243219879945,1.83406627987422));
#42508=CARTESIAN_POINT('Ctrl Pts',(367.298199692195,-10.1305367242282,1.72605498303068));
#42509=CARTESIAN_POINT('Ctrl Pts',(367.246223172796,-10.1367514604618,1.61525459220924));
#42510=CARTESIAN_POINT('Ctrl Pts',(367.199474743866,-10.1429661966954,1.50213333973738));
#42511=CARTESIAN_POINT('Ctrl Pts',(367.150661820684,-10.1494553867988,1.38401645039109));
#42512=CARTESIAN_POINT('Ctrl Pts',(367.107549552707,-10.1559445769023,1.2633692950333));
#42513=CARTESIAN_POINT('Ctrl Pts',(367.070388455924,-10.1624337670057,1.1407561054578));
#42514=CARTESIAN_POINT('Ctrl Pts',(367.034959130744,-10.1686205495883,1.02385690331095));
#42515=CARTESIAN_POINT('Ctrl Pts',(367.00493902324,-10.174807332171,0.905171141912029));
#42516=CARTESIAN_POINT('Ctrl Pts',(366.980497169477,-10.1809941147536,0.785210250520267));
#42517=CARTESIAN_POINT('Ctrl Pts',(366.956093310278,-10.187171280058,0.665435836874832));
#42518=CARTESIAN_POINT('Ctrl Pts',(366.937250502295,-10.1933484453624,0.544390574405071));
#42519=CARTESIAN_POINT('Ctrl Pts',(366.92408797741,-10.1995256106668,0.422600660547639));
#42520=CARTESIAN_POINT('Ctrl Pts',(366.91095107282,-10.2056907523818,0.30104780557353));
#42521=CARTESIAN_POINT('Ctrl Pts',(366.903472449916,-10.2118558940969,0.178753527193132));
#42522=CARTESIAN_POINT('Ctrl Pts',(366.901720164552,-10.2180210358119,0.0562531692756094));
#42523=CARTESIAN_POINT('Ctrl Pts',(366.901453425184,-10.2189595165201,0.0376057110399778));
#42524=CARTESIAN_POINT('Ctrl Pts',(366.901319280049,-10.2198979972282,0.0189534950297947));
#42525=CARTESIAN_POINT('Ctrl Pts',(366.901317864546,-10.2208364779364,0.000298426845041434));
#42526=CARTESIAN_POINT('',(366.901319464936,-11.4708364779244,-0.00356057907672602));
#42527=CARTESIAN_POINT('Ctrl Pts',(366.901317864546,-10.2208364779651,0.000298426274699534));
#42528=CARTESIAN_POINT('Ctrl Pts',(366.901308669822,-10.2269326063234,-0.120880079791976));
#42529=CARTESIAN_POINT('Ctrl Pts',(366.90690418874,-10.2330287346816,-0.241964705586346));
#42530=CARTESIAN_POINT('Ctrl Pts',(366.918052542601,-10.2391248630399,-0.36242932664784));
#42531=CARTESIAN_POINT('Ctrl Pts',(366.929214108592,-10.2452282160379,-0.483036712663392));
#42532=CARTESIAN_POINT('Ctrl Pts',(366.945941599533,-10.2513315690359,-0.60302226985431));
#42533=CARTESIAN_POINT('Ctrl Pts',(366.968131703025,-10.2574349220339,-0.721868168026967));
#42534=CARTESIAN_POINT('Ctrl Pts',(366.990371034528,-10.2635518151187,-0.840977721895112));
#42535=CARTESIAN_POINT('Ctrl Pts',(367.018097133237,-10.2696687082035,-0.958942208026564));
#42536=CARTESIAN_POINT('Ctrl Pts',(367.051155958216,-10.2757856012883,-1.07525581893695));
#42537=CARTESIAN_POINT('Ctrl Pts',(367.084254289864,-10.2819098043146,-1.19170842944621));
#42538=CARTESIAN_POINT('Ctrl Pts',(367.12269794591,-10.2880340073408,-1.30650588769926));
#42539=CARTESIAN_POINT('Ctrl Pts',(367.166284231668,-10.2941582103671,-1.41916114347041));
#42540=CARTESIAN_POINT('Ctrl Pts',(367.209966847428,-10.3002959484877,-1.53206537849831));
#42541=CARTESIAN_POINT('Ctrl Pts',(367.258814666438,-10.3064336866083,-1.64281761691705));
#42542=CARTESIAN_POINT('Ctrl Pts',(367.312577893879,-10.312571424729,-1.75095307154533));
#42543=CARTESIAN_POINT('Ctrl Pts',(367.342554728856,-10.3159936516214,-1.81124630230529));
#42544=CARTESIAN_POINT('Ctrl Pts',(367.374058892957,-10.3194158785138,-1.870726494836));
#42545=CARTESIAN_POINT('Ctrl Pts',(367.407041277237,-10.3228381054062,-1.92931704799599));
#42546=CARTESIAN_POINT('Ctrl Pts',(367.463650113153,-10.3287117947967,-2.0298780923987));
#42547=CARTESIAN_POINT('Ctrl Pts',(367.524782882167,-10.3345854841873,-2.12811303680054));
#42548=CARTESIAN_POINT('Ctrl Pts',(367.590223494545,-10.3404591735779,-2.2235873699918));
#42549=CARTESIAN_POINT('Ctrl Pts',(367.655579616944,-10.3463252794836,-2.31893843684947));
#42550=CARTESIAN_POINT('Ctrl Pts',(367.725232290604,-10.3521913853894,-2.41153564287257));
#42551=CARTESIAN_POINT('Ctrl Pts',(367.79891968103,-10.3580574912951,-2.50096919937823));
#42552=CARTESIAN_POINT('Ctrl Pts',(367.872531616506,-10.3639175903831,-2.59031117706125));
#42553=CARTESIAN_POINT('Ctrl Pts',(367.9501697897,-10.3697776894712,-2.67649563197347));
#42554=CARTESIAN_POINT('Ctrl Pts',(368.031529619935,-10.3756377885592,-2.75914246086288));
#42555=CARTESIAN_POINT('Ctrl Pts',(368.115824727233,-10.3817093066533,-2.8447709987913));
#42556=CARTESIAN_POINT('Ctrl Pts',(368.20411484412,-10.3877808247474,-2.92660145977786));
#42557=CARTESIAN_POINT('Ctrl Pts',(368.29601598023,-10.3938523428415,-3.00424909113004));
#42558=CARTESIAN_POINT('Ctrl Pts',(368.384615035074,-10.3997057064382,-3.07910678103308));
#42559=CARTESIAN_POINT('Ctrl Pts',(368.47656973873,-10.405559070035,-3.15007676361596));
#42560=CARTESIAN_POINT('Ctrl Pts',(368.571499803274,-10.4114124336317,-3.21685303873542));
#42561=CARTESIAN_POINT('Ctrl Pts',(368.666415614389,-10.4172649183656,-3.2836192876219));
#42562=CARTESIAN_POINT('Ctrl Pts',(368.764305560277,-10.4231174030995,-3.34619284343195));
#42563=CARTESIAN_POINT('Ctrl Pts',(368.864758757646,-10.4289698878334,-3.40430991083745));
#42564=CARTESIAN_POINT('Ctrl Pts',(368.965221165224,-10.4348229091615,-3.46243230679768));
#42565=CARTESIAN_POINT('Ctrl Pts',(369.068246933843,-10.4406759304897,-3.51609719518931));
#42566=CARTESIAN_POINT('Ctrl Pts',(369.173399495664,-10.4465289518179,-3.56508614335217));
#42567=CARTESIAN_POINT('Ctrl Pts',(369.278587127895,-10.4523839252417,-3.61409143027528));
#42568=CARTESIAN_POINT('Ctrl Pts',(369.385902589497,-10.4582388986655,-3.65841750156267));
#42569=CARTESIAN_POINT('Ctrl Pts',(369.49488886892,-10.4640938720893,-3.69789385948342));
#42570=CARTESIAN_POINT('Ctrl Pts',(369.603998670291,-10.4699554813734,-3.73741495878536));
#42571=CARTESIAN_POINT('Ctrl Pts',(369.714782680444,-10.4758170906575,-3.77207523320338));
#42572=CARTESIAN_POINT('Ctrl Pts',(369.826768151356,-10.4816786999417,-3.80175388449402));
#42573=CARTESIAN_POINT('Ctrl Pts',(369.938829134893,-10.487544261752,-3.83145254831726));
#42574=CARTESIAN_POINT('Ctrl Pts',(370.052092789734,-10.4934098235623,-3.85616281236528));
#42575=CARTESIAN_POINT('Ctrl Pts',(370.166077300005,-10.4992753853727,-3.87581521270471));
#42576=CARTESIAN_POINT('Ctrl Pts',(370.280228483586,-10.505149524073,-3.89549634967348));
#42577=CARTESIAN_POINT('Ctrl Pts',(370.395102217982,-10.5110236627733,-3.91010481078231));
#42578=CARTESIAN_POINT('Ctrl Pts',(370.510212637904,-10.5168978014736,-3.91962304429937));
#42579=CARTESIAN_POINT('Ctrl Pts',(370.539322183913,-10.518383275255,-3.92203005016969));
#42580=CARTESIAN_POINT('Ctrl Pts',(370.568446873907,-10.5198687490364,-3.92411179532515));
#42581=CARTESIAN_POINT('Ctrl Pts',(370.597578879703,-10.5213542228178,-3.92586852281327));
#42582=CARTESIAN_POINT('Ctrl Pts',(370.712769302795,-10.5272279122084,-3.93281477237919));
#42583=CARTESIAN_POINT('Ctrl Pts',(370.828457552963,-10.5331016015989,-3.93469852452861));
#42584=CARTESIAN_POINT('Ctrl Pts',(370.944161362727,-10.5389752909895,-3.93146580850197));
#42585=CARTESIAN_POINT('Ctrl Pts',(371.059715788002,-10.5448413968953,-3.92823726621543));
#42586=CARTESIAN_POINT('Ctrl Pts',(371.175285323712,-10.5507075028011,-3.919905404038));
#42587=CARTESIAN_POINT('Ctrl Pts',(371.290383678238,-10.5565736087068,-3.90646809320824));
#42588=CARTESIAN_POINT('Ctrl Pts',(371.405364173516,-10.5624337077949,-3.8930445420136));
#42589=CARTESIAN_POINT('Ctrl Pts',(371.519874039392,-10.5682938068829,-3.87452598854464));
#42590=CARTESIAN_POINT('Ctrl Pts',(371.633428756039,-10.5741539059709,-3.8509623167465));
#42591=CARTESIAN_POINT('Ctrl Pts',(371.751080267803,-10.580225424065,-3.82654852142728));
#42592=CARTESIAN_POINT('Ctrl Pts',(371.867705958403,-10.5862969421592,-3.79671871456764));
#42593=CARTESIAN_POINT('Ctrl Pts',(371.982774352302,-10.5923684602533,-3.76158698819061));
#42594=CARTESIAN_POINT('Ctrl Pts',(372.093708246849,-10.59822182385,-3.72771757281882));
#42595=CARTESIAN_POINT('Ctrl Pts',(372.203194399564,-10.6040751874468,-3.68892081630316));
#42596=CARTESIAN_POINT('Ctrl Pts',(372.310769518424,-10.6099285510435,-3.64535039198271));
#42597=CARTESIAN_POINT('Ctrl Pts',(372.418328485242,-10.6157810357774,-3.60178650961494));
#42598=CARTESIAN_POINT('Ctrl Pts',(372.523976605915,-10.6216335205113,-3.55345053966426));
#42599=CARTESIAN_POINT('Ctrl Pts',(372.627269467417,-10.6274860052452,-3.5005447446308));
#42600=CARTESIAN_POINT('Ctrl Pts',(372.730571799488,-10.6333390265734,-3.44763409884617));
#42601=CARTESIAN_POINT('Ctrl Pts',(372.831518075371,-10.6391920479016,-3.39015298341494));
#42602=CARTESIAN_POINT('Ctrl Pts',(372.929688076808,-10.6450450692298,-3.32834983529612));
#42603=CARTESIAN_POINT('Ctrl Pts',(373.027890819837,-10.6509000426536,-3.26652607463396));
#42604=CARTESIAN_POINT('Ctrl Pts',(373.123315097789,-10.6567550160774,-3.20037763495378));
#42605=CARTESIAN_POINT('Ctrl Pts',(373.215569889773,-10.6626099895012,-3.13019611820589));
#42606=CARTESIAN_POINT('Ctrl Pts',(373.307929240714,-10.6684715987854,-3.05993505972314));
#42607=CARTESIAN_POINT('Ctrl Pts',(373.397111606866,-10.6743332080695,-2.98563205106249));
#42608=CARTESIAN_POINT('Ctrl Pts',(373.482759199316,-10.6801948173537,-2.90761886022049));
#42609=CARTESIAN_POINT('Ctrl Pts',(373.568464544566,-10.686060379164,-2.8295530645113));
#42610=CARTESIAN_POINT('Ctrl Pts',(373.650630077893,-10.6919259409744,-2.74777239570561));
#42611=CARTESIAN_POINT('Ctrl Pts',(373.728936231239,-10.6977915027847,-2.66264407040357));
#42612=CARTESIAN_POINT('Ctrl Pts',(373.807356887388,-10.703665641485,-2.5773912666105));
#42613=CARTESIAN_POINT('Ctrl Pts',(373.881906635875,-10.7095397801854,-2.48878135186763));
#42614=CARTESIAN_POINT('Ctrl Pts',(373.952307335647,-10.7154139188857,-2.39721308762895));
#42615=CARTESIAN_POINT('Ctrl Pts',(373.970110523319,-10.716899392667,-2.37405696846678));
#42616=CARTESIAN_POINT('Ctrl Pts',(373.987648601557,-10.7183848664482,-2.35071179676868));
#42617=CARTESIAN_POINT('Ctrl Pts',(374.004917530866,-10.7198703402294,-2.32718428237531));
#42618=CARTESIAN_POINT('Ctrl Pts',(374.073200342821,-10.72574402962,-2.23415449388353));
#42619=CARTESIAN_POINT('Ctrl Pts',(374.137498975262,-10.7316177190106,-2.13796194939481));
#42620=CARTESIAN_POINT('Ctrl Pts',(374.19750663435,-10.7374914084011,-2.03898264399467));
#42621=CARTESIAN_POINT('Ctrl Pts',(374.257436817912,-10.7433575143069,-1.94013113017638));
#42622=CARTESIAN_POINT('Ctrl Pts',(374.313086833233,-10.7492236202127,-1.83850036069155));
#42623=CARTESIAN_POINT('Ctrl Pts',(374.364191268188,-10.7550897261184,-1.73449781617942));
#42624=CARTESIAN_POINT('Ctrl Pts',(374.415243372852,-10.7609498252065,-1.6306017689479));
#42625=CARTESIAN_POINT('Ctrl Pts',(374.461758974449,-10.7668099242945,-1.52433914610418));
#42626=CARTESIAN_POINT('Ctrl Pts',(374.503517328043,-10.7726700233826,-1.41614413602247));
#42627=CARTESIAN_POINT('Ctrl Pts',(374.546782227767,-10.7787415414767,-1.30404569680955));
#42628=CARTESIAN_POINT('Ctrl Pts',(374.584939903085,-10.7848130595708,-1.18987319180289));
#42629=CARTESIAN_POINT('Ctrl Pts',(374.617798108474,-10.7908845776649,-1.07413507443666));
#42630=CARTESIAN_POINT('Ctrl Pts',(374.649475692284,-10.7967379412616,-0.962555520122967));
#42631=CARTESIAN_POINT('Ctrl Pts',(374.676227958048,-10.8025913048584,-0.849521356133328));
#42632=CARTESIAN_POINT('Ctrl Pts',(374.697932883667,-10.8084446684551,-0.735505198168392));
#42633=CARTESIAN_POINT('Ctrl Pts',(374.719634550365,-10.814297153189,-0.621506159345897));
#42634=CARTESIAN_POINT('Ctrl Pts',(374.736290306551,-10.8201496379229,-0.506525825467728));
#42635=CARTESIAN_POINT('Ctrl Pts',(374.747829194461,-10.8260021226568,-0.391047288712072));
#42636=CARTESIAN_POINT('Ctrl Pts',(374.759369140333,-10.831855143985,-0.27555816412495));
#42637=CARTESIAN_POINT('Ctrl Pts',(374.765791244227,-10.8377081653132,-0.15957115697606));
#42638=CARTESIAN_POINT('Ctrl Pts',(374.767076465356,-10.8435611866414,-0.0435740600023058));
#42639=CARTESIAN_POINT('Ctrl Pts',(374.768362115131,-10.8494161600652,0.0724617242429357));
#42640=CARTESIAN_POINT('Ctrl Pts',(374.764507470846,-10.855271133489,0.188507192107884));
#42641=CARTESIAN_POINT('Ctrl Pts',(374.755545591765,-10.8611261069128,0.304075685480253));
#42642=CARTESIAN_POINT('Ctrl Pts',(374.746573555545,-10.8669877161969,0.419775160896118));
#42643=CARTESIAN_POINT('Ctrl Pts',(374.732482763201,-10.8728493254811,0.534996170696944));
#42644=CARTESIAN_POINT('Ctrl Pts',(374.713358041213,-10.8787109347653,0.649258207466544));
#42645=CARTESIAN_POINT('Ctrl Pts',(374.694220423285,-10.8845764965756,0.763597291966407));
#42646=CARTESIAN_POINT('Ctrl Pts',(374.670042202632,-10.8904420583859,0.876975712766699));
#42647=CARTESIAN_POINT('Ctrl Pts',(374.640958713361,-10.8963076201963,0.988925862710946));
#42648=CARTESIAN_POINT('Ctrl Pts',(374.611832696895,-10.9021817588966,1.10103971123219));
#42649=CARTESIAN_POINT('Ctrl Pts',(374.577787217894,-10.9080558975969,1.21172072744426));
#42650=CARTESIAN_POINT('Ctrl Pts',(374.539006575828,-10.9139300362973,1.32051901486169));
#42651=CARTESIAN_POINT('Ctrl Pts',(374.529199584548,-10.9154155100785,1.3480323256042));
#42652=CARTESIAN_POINT('Ctrl Pts',(374.519090012593,-10.9169009838598,1.37542534998755));
#42653=CARTESIAN_POINT('Ctrl Pts',(374.508681308446,-10.9183864576411,1.40269105612236));
#42654=CARTESIAN_POINT('Ctrl Pts',(374.467524408952,-10.9242601470317,1.51050197198515));
#42655=CARTESIAN_POINT('Ctrl Pts',(374.421549959167,-10.9301338364222,1.61667951064537));
#42656=CARTESIAN_POINT('Ctrl Pts',(374.370907594853,-10.9360075258128,1.72076204031954));
#42657=CARTESIAN_POINT('Ctrl Pts',(374.320330614589,-10.9418736317185,1.82471018966963));
#42658=CARTESIAN_POINT('Ctrl Pts',(374.265097884067,-10.9477397376243,1.92656834098959));
#42659=CARTESIAN_POINT('Ctrl Pts',(374.205407930028,-10.95360584353,2.0258925672578));
#42660=CARTESIAN_POINT('Ctrl Pts',(374.145779097742,-10.959465942618,2.1251150867839));
#42661=CARTESIAN_POINT('Ctrl Pts',(374.081702331938,-10.9653260417061,2.22180849033149));
#42662=CARTESIAN_POINT('Ctrl Pts',(374.013422816585,-10.9711861407941,2.31555190655123));
#42663=CARTESIAN_POINT('Ctrl Pts',(373.942679932089,-10.9772576588882,2.41267737136529));
#42664=CARTESIAN_POINT('Ctrl Pts',(373.867425518904,-10.9833291769823,2.50663556622539));
#42665=CARTESIAN_POINT('Ctrl Pts',(373.787982616316,-10.9894006950764,2.59698930826947));
#42666=CARTESIAN_POINT('Ctrl Pts',(373.711394160708,-10.9952540586732,2.68409656815289));
#42667=CARTESIAN_POINT('Ctrl Pts',(373.630913323417,-11.0011074222699,2.76785360237273));
#42668=CARTESIAN_POINT('Ctrl Pts',(373.546871097785,-11.0069607858667,2.84790166533533));
#42669=CARTESIAN_POINT('Ctrl Pts',(373.462841490811,-11.0128132706006,2.92793770935062));
#42670=CARTESIAN_POINT('Ctrl Pts',(373.37525185782,-11.0186657553344,3.00426560454857));
#42671=CARTESIAN_POINT('Ctrl Pts',(373.284469678083,-11.0245182400683,3.07656383570034));
#42672=CARTESIAN_POINT('Ctrl Pts',(373.193679174839,-11.0303712613965,3.14886869562922));
#42673=CARTESIAN_POINT('Ctrl Pts',(373.09969586616,-11.0362242827247,3.2171428996557));
#42674=CARTESIAN_POINT('Ctrl Pts',(373.002919325918,-11.0420773040529,3.28110601057466));
#42675=CARTESIAN_POINT('Ctrl Pts',(372.906110508831,-11.0479322774767,3.34509045442614));
#42676=CARTESIAN_POINT('Ctrl Pts',(372.806506952223,-11.0537872509004,3.40476071842432));
#42677=CARTESIAN_POINT('Ctrl Pts',(372.704535520467,-11.0596422243242,3.45988076053695));
#42678=CARTESIAN_POINT('Ctrl Pts',(372.602448517189,-11.0655038336084,3.51506327413752));
#42679=CARTESIAN_POINT('Ctrl Pts',(372.497988645944,-11.0713654428925,3.56568507603903));
#42680=CARTESIAN_POINT('Ctrl Pts',(372.391605666124,-11.0772270521767,3.61155695895714));
#42681=CARTESIAN_POINT('Ctrl Pts',(372.28515095148,-11.083092613987,3.65745977362282));
#42682=CARTESIAN_POINT('Ctrl Pts',(372.176770931402,-11.0889581757973,3.69860614533514));
#42683=CARTESIAN_POINT('Ctrl Pts',(372.066931905761,-11.0948237376077,3.73485630212038));
#42684=CARTESIAN_POINT('Ctrl Pts',(371.956932268524,-11.100697876308,3.77115946552583));
#42685=CARTESIAN_POINT('Ctrl Pts',(371.845469764092,-11.1065720150084,3.80255201393653));
#42686=CARTESIAN_POINT('Ctrl Pts',(371.733022354505,-11.1124461537087,3.82894492247894));
#42687=CARTESIAN_POINT('Ctrl Pts',(371.704586240337,-11.11393162749,3.83561925818212));
#42688=CARTESIAN_POINT('Ctrl Pts',(371.676087171879,-11.1154171012714,3.84197412459062));
#42689=CARTESIAN_POINT('Ctrl Pts',(371.647532927538,-11.1169025750527,3.8480086074369));
#42690=CARTESIAN_POINT('Ctrl Pts',(371.534627022264,-11.1227762644433,3.87186946470481));
#42691=CARTESIAN_POINT('Ctrl Pts',(371.420482016839,-11.1286499538339,3.89079662734259));
#42692=CARTESIAN_POINT('Ctrl Pts',(371.305566943042,-11.1345236432244,3.90466558047495));
#42693=CARTESIAN_POINT('Ctrl Pts',(371.190800235401,-11.1403897491302,3.91851662748592));
#42694=CARTESIAN_POINT('Ctrl Pts',(371.075265843009,-11.146255855036,3.92732240321006));
#42695=CARTESIAN_POINT('Ctrl Pts',(370.959444424461,-11.1521219609418,3.93100907416535));
#42696=CARTESIAN_POINT('Ctrl Pts',(370.843741605572,-11.1579820600298,3.93469197001653));
#42697=CARTESIAN_POINT('Ctrl Pts',(370.727752755621,-11.1638421591178,3.93326617460275));
#42698=CARTESIAN_POINT('Ctrl Pts',(370.611964452668,-11.1697022582059,3.92670955957546));
#42699=CARTESIAN_POINT('Ctrl Pts',(370.4919987719,-11.1757737763,3.91991639683599));
#42700=CARTESIAN_POINT('Ctrl Pts',(370.372248830317,-11.1818452943941,3.90761515397088));
#42701=CARTESIAN_POINT('Ctrl Pts',(370.253257118779,-11.1879168124882,3.88984028243908));
#42702=CARTESIAN_POINT('Ctrl Pts',(370.138540874531,-11.1937701760849,3.87270407624671));
#42703=CARTESIAN_POINT('Ctrl Pts',(370.024529754068,-11.1996235396817,3.85048088198586));
#42704=CARTESIAN_POINT('Ctrl Pts',(369.911704648765,-11.2054769032785,3.82325435656048));
#42705=CARTESIAN_POINT('Ctrl Pts',(369.798896483773,-11.2113293880124,3.79603191910633));
#42706=CARTESIAN_POINT('Ctrl Pts',(369.687274381367,-11.2171818727463,3.76380774111228));
#42707=CARTESIAN_POINT('Ctrl Pts',(369.577307727326,-11.2230343574802,3.72671632182953));
#42708=CARTESIAN_POINT('Ctrl Pts',(369.467330990819,-11.2288873788083,3.68962150176155));
#42709=CARTESIAN_POINT('Ctrl Pts',(369.359010395903,-11.2347404001365,3.6476586853312));
#42710=CARTESIAN_POINT('Ctrl Pts',(369.252798208958,-11.2405934214647,3.60101160992311));
#42711=CARTESIAN_POINT('Ctrl Pts',(369.146550598198,-11.2464483948885,3.55434897681455));
#42712=CARTESIAN_POINT('Ctrl Pts',(369.042413171748,-11.2523033683124,3.50299914422488));
#42713=CARTESIAN_POINT('Ctrl Pts',(368.940815684815,-11.2581583417362,3.44719284900503));
#42714=CARTESIAN_POINT('Ctrl Pts',(368.839103050181,-11.2640199510204,3.39132330451753));
#42715=CARTESIAN_POINT('Ctrl Pts',(368.739936463082,-11.2698815603045,3.33098741526696));
#42716=CARTESIAN_POINT('Ctrl Pts',(368.64371873473,-11.2757431695887,3.26646054653273));
#42717=CARTESIAN_POINT('Ctrl Pts',(368.547436126058,-11.281608731399,3.20189016685768));
#42718=CARTESIAN_POINT('Ctrl Pts',(368.454106667338,-11.2874742932093,3.13312342495507));
#42719=CARTESIAN_POINT('Ctrl Pts',(368.364100595649,-11.2933398550196,3.06047638454874));
#42720=CARTESIAN_POINT('Ctrl Pts',(368.273962913008,-11.2992139937199,2.9877231163509));
#42721=CARTESIAN_POINT('Ctrl Pts',(368.187158624461,-11.3050881324203,2.91107849827512));
#42722=CARTESIAN_POINT('Ctrl Pts',(368.104021646077,-11.3109622711206,2.83089590434556));
#42723=CARTESIAN_POINT('Ctrl Pts',(368.082997661466,-11.3124477449019,2.81061903533164));
#42724=CARTESIAN_POINT('Ctrl Pts',(368.06220800129,-11.3139332186832,2.79011607799069));
#42725=CARTESIAN_POINT('Ctrl Pts',(368.041657650564,-11.3154186924644,2.7693930729458));
#42726=CARTESIAN_POINT('Ctrl Pts',(367.961508675604,-11.3212122286667,2.68857072423641));
#42727=CARTESIAN_POINT('Ctrl Pts',(367.884719897014,-11.327005764869,2.60411321589936));
#42728=CARTESIAN_POINT('Ctrl Pts',(367.811645983487,-11.3327993010713,2.51633538462223));
#42729=CARTESIAN_POINT('Ctrl Pts',(367.738687843669,-11.3385836583596,2.42869662301526));
#42730=CARTESIAN_POINT('Ctrl Pts',(367.669433128666,-11.3443680156479,2.33774832840426));
#42731=CARTESIAN_POINT('Ctrl Pts',(367.604200404663,-11.3501523729361,2.24384274593864));
#42732=CARTESIAN_POINT('Ctrl Pts',(367.539026703765,-11.3559314964904,2.15002213001591));
#42733=CARTESIAN_POINT('Ctrl Pts',(367.477868005425,-11.3617106200446,2.05324988897528));
#42734=CARTESIAN_POINT('Ctrl Pts',(367.421003061589,-11.3674897435988,1.95391175164293));
#42735=CARTESIAN_POINT('Ctrl Pts',(367.364174919228,-11.3732651270585,1.85463790330231));
#42736=CARTESIAN_POINT('Ctrl Pts',(367.311635219995,-11.3790405105182,1.75280182649306));
#42737=CARTESIAN_POINT('Ctrl Pts',(367.263619271642,-11.3848158939779,1.64881795219631));
#42738=CARTESIAN_POINT('Ctrl Pts',(367.215622031528,-11.3905890272007,1.54487459267253));
#42739=CARTESIAN_POINT('Ctrl Pts',(367.17214521611,-11.3963621604235,1.43878548518357));
#42740=CARTESIAN_POINT('Ctrl Pts',(367.133377649361,-11.4021352936463,1.33098858275673));
#42741=CARTESIAN_POINT('Ctrl Pts',(367.094601015693,-11.4079097770835,1.22316646890099));
#42742=CARTESIAN_POINT('Ctrl Pts',(367.060535985716,-11.4136842605208,1.11363615900919));
#42743=CARTESIAN_POINT('Ctrl Pts',(367.031322638993,-11.4194587439581,1.00285412724623));
#42744=CARTESIAN_POINT('Ctrl Pts',(367.002107164036,-11.4252336480747,0.892064024853437));
#42745=CARTESIAN_POINT('Ctrl Pts',(366.977744175852,-11.4310085521914,0.780022433116942));
#42746=CARTESIAN_POINT('Ctrl Pts',(366.958323041382,-11.436783456308,0.667198035500687));
#42747=CARTESIAN_POINT('Ctrl Pts',(366.938882937663,-11.4425640009601,0.554263438651138));
#42748=CARTESIAN_POINT('Ctrl Pts',(366.924394394745,-11.4483445456121,0.440544929953996));
#42749=CARTESIAN_POINT('Ctrl Pts',(366.914895097852,-11.4541250902642,0.326518398678384));
#42750=CARTESIAN_POINT('Ctrl Pts',(366.90574103352,-11.4596955528176,0.216635928980348));
#42751=CARTESIAN_POINT('Ctrl Pts',(366.901219855256,-11.465266015371,0.106467790374153));
#42752=CARTESIAN_POINT('Ctrl Pts',(366.901319464936,-11.4708364779244,-0.00356057907674602));
#42753=CARTESIAN_POINT('',(366.901318279586,-12.7208364780083,0.00183132834481399));
#42754=CARTESIAN_POINT('Ctrl Pts',(366.901319464937,-11.470836477965,-0.00356057987879464));
#42755=CARTESIAN_POINT('Ctrl Pts',(366.901464067762,-11.4789230860767,-0.163288124293369));
#42756=CARTESIAN_POINT('Ctrl Pts',(366.911342487007,-11.4870096941884,-0.322591275985424));
#42757=CARTESIAN_POINT('Ctrl Pts',(366.930779443932,-11.4950963023001,-0.480496500694793));
#42758=CARTESIAN_POINT('Ctrl Pts',(366.945872845072,-11.5013758048254,-0.603114815275443));
#42759=CARTESIAN_POINT('Ctrl Pts',(366.966729094728,-11.5076553073508,-0.724891027394278));
#42760=CARTESIAN_POINT('Ctrl Pts',(366.993247465156,-11.5139348098761,-0.845379958307364));
#42761=CARTESIAN_POINT('Ctrl Pts',(367.018052084696,-11.5198084992667,-0.958082286609465));
#42762=CARTESIAN_POINT('Ctrl Pts',(367.047862483551,-11.5256821886572,-1.06987969207649));
#42763=CARTESIAN_POINT('Ctrl Pts',(367.082598753345,-11.5315558780478,-1.18029352095419));
#42764=CARTESIAN_POINT('Ctrl Pts',(367.117290175353,-11.5374219839536,-1.29056479520598));
#42765=CARTESIAN_POINT('Ctrl Pts',(367.156894697966,-11.5432880898593,-1.39945565478516));
#42766=CARTESIAN_POINT('Ctrl Pts',(367.201281445146,-11.5491541957651,-1.50649774562716));
#42767=CARTESIAN_POINT('Ctrl Pts',(367.245622740862,-11.5550142948531,-1.61343022673162));
#42768=CARTESIAN_POINT('Ctrl Pts',(367.294736363421,-11.5608743939411,-1.71851732529604));
#42769=CARTESIAN_POINT('Ctrl Pts',(367.348441889177,-11.5667344930292,-1.82130660880631));
#42770=CARTESIAN_POINT('Ctrl Pts',(367.404084987781,-11.5728060111233,-1.9278042951658));
#42771=CARTESIAN_POINT('Ctrl Pts',(367.464657440499,-11.5788775292174,-2.03183480538736));
#42772=CARTESIAN_POINT('Ctrl Pts',(367.529904225892,-11.5849490473115,-2.13291809020064));
#42773=CARTESIAN_POINT('Ctrl Pts',(367.592806642143,-11.5908024109082,-2.23036937180685));
#42774=CARTESIAN_POINT('Ctrl Pts',(367.660053023659,-11.596655774505,-2.32508119855194));
#42775=CARTESIAN_POINT('Ctrl Pts',(367.731368912453,-11.6025091381017,-2.41664992726858));
#42776=CARTESIAN_POINT('Ctrl Pts',(367.802674093406,-11.6083616228356,-2.50820490724874));
#42777=CARTESIAN_POINT('Ctrl Pts',(367.878047312904,-11.6142141075695,-2.59661740170169));
#42778=CARTESIAN_POINT('Ctrl Pts',(367.957172534633,-11.6200665923034,-2.6815152089275));
#42779=CARTESIAN_POINT('Ctrl Pts',(368.036305011083,-11.6259196136316,-2.76642080014239));
#42780=CARTESIAN_POINT('Ctrl Pts',(368.119189891923,-11.6317726349598,-2.8478107612795));
#42781=CARTESIAN_POINT('Ctrl Pts',(368.205473338279,-11.637625656288,-2.92534878540034));
#42782=CARTESIAN_POINT('Ctrl Pts',(368.291785561831,-11.6434806297118,-3.0029126699497));
#42783=CARTESIAN_POINT('Ctrl Pts',(368.381498297658,-11.6493356031356,-3.07662178692343));
#42784=CARTESIAN_POINT('Ctrl Pts',(368.474224166602,-11.6551905765595,-3.14617971361588));
#42785=CARTESIAN_POINT('Ctrl Pts',(368.567055128408,-11.6610521858436,-3.21581647528381));
#42786=CARTESIAN_POINT('Ctrl Pts',(368.662905708786,-11.6669137951278,-3.2812924080347));
#42787=CARTESIAN_POINT('Ctrl Pts',(368.761358975856,-11.6727754044119,-3.34235403461983));
#42788=CARTESIAN_POINT('Ctrl Pts',(368.859878630686,-11.6786409662223,-3.40345683550811));
#42789=CARTESIAN_POINT('Ctrl Pts',(368.961004107323,-11.6845065280326,-3.46013920165616));
#42790=CARTESIAN_POINT('Ctrl Pts',(369.06429482262,-11.690372089843,-3.5121941106853));
#42791=CARTESIAN_POINT('Ctrl Pts',(369.167736574278,-11.6962462285433,-3.56432513675877));
#42792=CARTESIAN_POINT('Ctrl Pts',(369.273349508,-11.7021203672436,-3.61181503274357));
#42793=CARTESIAN_POINT('Ctrl Pts',(369.380674020833,-11.7079945059439,-3.65450524812225));
#42794=CARTESIAN_POINT('Ctrl Pts',(369.407814638043,-11.7094799797252,-3.66530090666838));
#42795=CARTESIAN_POINT('Ctrl Pts',(369.435064642667,-11.7109654535065,-3.67578987601305));
#42796=CARTESIAN_POINT('Ctrl Pts',(369.462416476234,-11.7124509272877,-3.68597010457407));
#42797=CARTESIAN_POINT('Ctrl Pts',(369.570567947274,-11.7183246166783,-3.72622359221322));
#42798=CARTESIAN_POINT('Ctrl Pts',(369.680672685131,-11.7241983060688,-3.76178011693693));
#42799=CARTESIAN_POINT('Ctrl Pts',(369.792285154209,-11.7300719954594,-3.79244734362707));
#42800=CARTESIAN_POINT('Ctrl Pts',(369.903753521104,-11.7359381013651,-3.82307497604649));
#42801=CARTESIAN_POINT('Ctrl Pts',(370.016725353285,-11.7418042072709,-3.84882575554942));
#42802=CARTESIAN_POINT('Ctrl Pts',(370.130736140009,-11.7476703131766,-3.86955575910594));
#42803=CARTESIAN_POINT('Ctrl Pts',(370.244630181141,-11.7535304122646,-3.89026453540292));
#42804=CARTESIAN_POINT('Ctrl Pts',(370.359560656613,-11.7593905113527,-3.9059626885785));
#42805=CARTESIAN_POINT('Ctrl Pts',(370.475049574461,-11.7652506104407,-3.91655656206763));
#42806=CARTESIAN_POINT('Ctrl Pts',(370.594705068994,-11.7713221285348,-3.92753263834379));
#42807=CARTESIAN_POINT('Ctrl Pts',(370.714959625805,-11.7773936466289,-3.93302906002744));
#42808=CARTESIAN_POINT('Ctrl Pts',(370.83527160618,-11.783465164723,-3.9329998843574));
#42809=CARTESIAN_POINT('Ctrl Pts',(370.951260680948,-11.7893185283198,-3.9329717569925));
#42810=CARTESIAN_POINT('Ctrl Pts',(371.067302675186,-11.7951718919165,-3.92780827699223));
#42811=CARTESIAN_POINT('Ctrl Pts',(371.182909618086,-11.8010252555132,-3.9175212547567));
#42812=CARTESIAN_POINT('Ctrl Pts',(371.298499202993,-11.8068777402471,-3.90723577708294));
#42813=CARTESIAN_POINT('Ctrl Pts',(371.413653455037,-11.812730224981,-3.89182832340498));
#42814=CARTESIAN_POINT('Ctrl Pts',(371.527888283919,-11.8185827097149,-3.87136268743516));
#42815=CARTESIAN_POINT('Ctrl Pts',(371.642133586601,-11.8244357310431,-3.85089517504131));
#42816=CARTESIAN_POINT('Ctrl Pts',(371.755458891851,-11.8302887523712,-3.82536863129001));
#42817=CARTESIAN_POINT('Ctrl Pts',(371.867389778888,-11.8361417736994,-3.79489807457389));
#42818=CARTESIAN_POINT('Ctrl Pts',(371.979357997038,-11.8419967471232,-3.76441735533867));
#42819=CARTESIAN_POINT('Ctrl Pts',(372.089930473792,-11.847851720547,-3.72898945278846));
#42820=CARTESIAN_POINT('Ctrl Pts',(372.198648120898,-11.8537066939708,-3.68877919110236));
#42821=CARTESIAN_POINT('Ctrl Pts',(372.307488985492,-11.859568303255,-3.64852335624944));
#42822=CARTESIAN_POINT('Ctrl Pts',(372.414470436844,-11.8654299125391,-3.60347448728542));
#42823=CARTESIAN_POINT('Ctrl Pts',(372.519153453294,-11.8712915218232,-3.5538455229139));
#42824=CARTESIAN_POINT('Ctrl Pts',(372.623907058272,-11.8771570836336,-3.50418309336718));
#42825=CARTESIAN_POINT('Ctrl Pts',(372.726358778034,-11.8830226454439,-3.44993461159245));
#42826=CARTESIAN_POINT('Ctrl Pts',(372.826095805739,-11.8888882072542,-3.39135807426401));
#42827=CARTESIAN_POINT('Ctrl Pts',(372.92597867344,-11.8947623459546,-3.33269588367121));
#42828=CARTESIAN_POINT('Ctrl Pts',(373.023138581555,-11.9006364846549,-3.2696932309884));
#42829=CARTESIAN_POINT('Ctrl Pts',(373.117193143708,-11.9065106233552,-3.20265037244101));
#42830=CARTESIAN_POINT('Ctrl Pts',(373.140978007027,-11.9079960971366,-3.18569632799576));
#42831=CARTESIAN_POINT('Ctrl Pts',(373.16456445696,-11.909481570918,-3.1684841053142));
#42832=CARTESIAN_POINT('Ctrl Pts',(373.187946672029,-11.9109670446994,-3.15101894365791));
#42833=CARTESIAN_POINT('Ctrl Pts',(373.28040193465,-11.91684073409,-3.08196021235674));
#42834=CARTESIAN_POINT('Ctrl Pts',(373.369969186994,-11.9227144234806,-3.00871386735199));
#42835=CARTESIAN_POINT('Ctrl Pts',(373.456245279269,-11.9285881128711,-2.93155002900421));
#42836=CARTESIAN_POINT('Ctrl Pts',(373.542409981003,-11.9344542187769,-2.85448581642098));
#42837=CARTESIAN_POINT('Ctrl Pts',(373.625291667792,-11.9403203246826,-2.77351444181067));
#42838=CARTESIAN_POINT('Ctrl Pts',(373.704517584294,-11.9461864305884,-2.68894821515114));
#42839=CARTESIAN_POINT('Ctrl Pts',(373.783662374467,-11.9520465296764,-2.60446858323037));
#42840=CARTESIAN_POINT('Ctrl Pts',(373.859158559626,-11.9579066287645,-2.51640172094925));
#42841=CARTESIAN_POINT('Ctrl Pts',(373.930668315433,-11.9637667278525,-2.42509851659249));
#42842=CARTESIAN_POINT('Ctrl Pts',(374.004757980089,-11.9698382459466,-2.33050130091862));
#42843=CARTESIAN_POINT('Ctrl Pts',(374.074567805351,-11.9759097640407,-2.23243011563941));
#42844=CARTESIAN_POINT('Ctrl Pts',(374.139765557656,-11.9819812821348,-2.13131519800962));
#42845=CARTESIAN_POINT('Ctrl Pts',(374.202620702615,-11.9878346457316,-2.03383342017918));
#42846=CARTESIAN_POINT('Ctrl Pts',(374.261189258605,-11.9936880093283,-1.93352325019779));
#42847=CARTESIAN_POINT('Ctrl Pts',(374.315216616381,-11.9995413729251,-1.83080113629325));
#42848=CARTESIAN_POINT('Ctrl Pts',(374.369235862131,-12.005393857659,-1.72809444576845));
#42849=CARTESIAN_POINT('Ctrl Pts',(374.418715073166,-12.0112463423929,-1.62297689695675));
#42850=CARTESIAN_POINT('Ctrl Pts',(374.463445425888,-12.0170988271268,-1.51588985791451));
#42851=CARTESIAN_POINT('Ctrl Pts',(374.508179879783,-12.022951848455,-1.40879300042859));
#42852=CARTESIAN_POINT('Ctrl Pts',(374.54816445057,-12.0288048697832,-1.29972667498969));
#42853=CARTESIAN_POINT('Ctrl Pts',(374.583238601092,-12.0346578911113,-1.18915189366549));
#42854=CARTESIAN_POINT('Ctrl Pts',(374.618324449519,-12.0405128645352,-1.07854023351634));
#42855=CARTESIAN_POINT('Ctrl Pts',(374.6484964963,-12.046367837959,-0.966419510687292));
#42856=CARTESIAN_POINT('Ctrl Pts',(374.673644368378,-12.0522228113828,-0.853264853394234));
#42857=CARTESIAN_POINT('Ctrl Pts',(374.698820742338,-12.058084420667,-0.739981949831268));
#42858=CARTESIAN_POINT('Ctrl Pts',(374.718961486519,-12.0639460299511,-0.6256631764289));
#42859=CARTESIAN_POINT('Ctrl Pts',(374.734007537168,-12.0698076392353,-0.510792882628788));
#42860=CARTESIAN_POINT('Ctrl Pts',(374.749063733479,-12.0756732010456,-0.395845130945944));
#42861=CARTESIAN_POINT('Ctrl Pts',(374.759018360247,-12.081538762856,-0.280345528941752));
#42862=CARTESIAN_POINT('Ctrl Pts',(374.763864427585,-12.0874043246663,-0.164780823896794));
#42863=CARTESIAN_POINT('Ctrl Pts',(374.768717581063,-12.0932784633667,-0.0490471349089849));
#42864=CARTESIAN_POINT('Ctrl Pts',(374.768447267897,-12.099152602067,0.0667514355525111));
#42865=CARTESIAN_POINT('Ctrl Pts',(374.763098500457,-12.1050267407673,0.182130793459123));
#42866=CARTESIAN_POINT('Ctrl Pts',(374.761745884491,-12.1065122145486,0.211308349490523));
#42867=CARTESIAN_POINT('Ctrl Pts',(374.760068757544,-12.1079976883298,0.240459138075285));
#42868=CARTESIAN_POINT('Ctrl Pts',(374.758068366329,-12.109483162111,0.269575427124148));
#42869=CARTESIAN_POINT('Ctrl Pts',(374.750158649708,-12.1153568515016,0.384703704876508));
#42870=CARTESIAN_POINT('Ctrl Pts',(374.737164430592,-12.1212305408922,0.499675310147675));
#42871=CARTESIAN_POINT('Ctrl Pts',(374.719094141903,-12.1271042302827,0.614005038186375));
#42872=CARTESIAN_POINT('Ctrl Pts',(374.701047183654,-12.1329703361885,0.728187155805334));
#42873=CARTESIAN_POINT('Ctrl Pts',(374.677937252867,-12.1388364420943,0.841728639899625));
#42874=CARTESIAN_POINT('Ctrl Pts',(374.64982471185,-12.144702548,0.954146955020592));
#42875=CARTESIAN_POINT('Ctrl Pts',(374.621740957718,-12.1505626470881,1.06645015521903));
#42876=CARTESIAN_POINT('Ctrl Pts',(374.588664882284,-12.1564227461761,1.1776320756891));
#42877=CARTESIAN_POINT('Ctrl Pts',(374.550708201941,-12.1622828452641,1.28721862011283));
#42878=CARTESIAN_POINT('Ctrl Pts',(374.511382131164,-12.1683543633583,1.40075879705231));
#42879=CARTESIAN_POINT('Ctrl Pts',(374.466816714825,-12.1744258814524,1.51258586332731));
#42880=CARTESIAN_POINT('Ctrl Pts',(374.417193377692,-12.1804973995465,1.62218740476106));
#42881=CARTESIAN_POINT('Ctrl Pts',(374.36935304672,-12.1863507631432,1.72785087521986));
#42882=CARTESIAN_POINT('Ctrl Pts',(374.316812194979,-12.19220412674,1.83144558961505));
#42883=CARTESIAN_POINT('Ctrl Pts',(374.259782741088,-12.1980574903367,1.93253183725646));
#42884=CARTESIAN_POINT('Ctrl Pts',(374.202761849978,-12.2039099750707,2.03360290713796));
#42885=CARTESIAN_POINT('Ctrl Pts',(374.141253899732,-12.2097624598046,2.13216589942927));
#42886=CARTESIAN_POINT('Ctrl Pts',(374.075516570133,-12.2156149445385,2.22780606820031));
#42887=CARTESIAN_POINT('Ctrl Pts',(374.009773213302,-12.2214679658667,2.32345500589072));
#42888=CARTESIAN_POINT('Ctrl Pts',(373.939799940288,-12.2273209871948,2.41618024684152));
#42889=CARTESIAN_POINT('Ctrl Pts',(373.865897114426,-12.233174008523,2.5055969713922));
#42890=CARTESIAN_POINT('Ctrl Pts',(373.791969640545,-12.2390289819469,2.59504351814734));
#42891=CARTESIAN_POINT('Ctrl Pts',(373.714110270844,-12.2448839553707,2.68117903605044));
#42892=CARTESIAN_POINT('Ctrl Pts',(373.632658425007,-12.2507389287945,2.76365320623102));
#42893=CARTESIAN_POINT('Ctrl Pts',(373.551114263966,-12.2566005380787,2.84622085029007));
#42894=CARTESIAN_POINT('Ctrl Pts',(373.465969790572,-12.2624621473628,2.92511857002222));
#42895=CARTESIAN_POINT('Ctrl Pts',(373.377599988441,-12.268323756647,3.0000341632531));
#42896=CARTESIAN_POINT('Ctrl Pts',(373.289170597903,-12.2741893184573,3.07500027261867));
#42897=CARTESIAN_POINT('Ctrl Pts',(373.19751187384,-12.2800548802677,3.14597865637191));
#42898=CARTESIAN_POINT('Ctrl Pts',(373.103029044526,-12.285920442078,3.21269957052663));
#42899=CARTESIAN_POINT('Ctrl Pts',(373.008408058142,-12.2917945807784,3.27951804702221));
#42900=CARTESIAN_POINT('Ctrl Pts',(372.91095507135,-12.2976687194787,3.34206640715571));
#42901=CARTESIAN_POINT('Ctrl Pts',(372.811101273794,-12.303542858179,3.40012004319834));
#42902=CARTESIAN_POINT('Ctrl Pts',(372.785849878519,-12.3050283319603,3.41480086002022));
#42903=CARTESIAN_POINT('Ctrl Pts',(372.76044505565,-12.3065138057415,3.42919447683105));
#42904=CARTESIAN_POINT('Ctrl Pts',(372.734893978377,-12.3079992795227,3.44329774961413));
#42905=CARTESIAN_POINT('Ctrl Pts',(372.633862850537,-12.3138729689133,3.49906328702403));
#42906=CARTESIAN_POINT('Ctrl Pts',(372.530207018652,-12.3197466583038,3.55047134344603));
#42907=CARTESIAN_POINT('Ctrl Pts',(372.424338775647,-12.3256203476944,3.59726597101978));
#42908=CARTESIAN_POINT('Ctrl Pts',(372.31860721849,-12.3314864536001,3.64400018233316));
#42909=CARTESIAN_POINT('Ctrl Pts',(372.210669305144,-12.3373525595059,3.68613264456589));
#42910=CARTESIAN_POINT('Ctrl Pts',(372.100963236915,-12.3432186654116,3.72345249358361));
#42911=CARTESIAN_POINT('Ctrl Pts',(371.991369506302,-12.3490787644997,3.76073412755138));
#42912=CARTESIAN_POINT('Ctrl Pts',(371.880011610985,-12.3549388635877,3.79321281834832));
#42913=CARTESIAN_POINT('Ctrl Pts',(371.767348500337,-12.3607989626757,3.82072543001294));
#42914=CARTESIAN_POINT('Ctrl Pts',(371.650620761683,-12.3668704807698,3.84923063394015));
#42915=CARTESIAN_POINT('Ctrl Pts',(371.532492264303,-12.3729419988639,3.87240448109277));
#42916=CARTESIAN_POINT('Ctrl Pts',(371.413491945943,-12.379013516958,3.89012163952794));
#42917=CARTESIAN_POINT('Ctrl Pts',(371.298767404124,-12.3848668805548,3.90720220630131));
#42918=CARTESIAN_POINT('Ctrl Pts',(371.183233057243,-12.3907202441515,3.91921139624767));
#42919=CARTESIAN_POINT('Ctrl Pts',(371.067373280744,-12.3965736077483,3.92608891490036));
#42920=CARTESIAN_POINT('Ctrl Pts',(370.951530900201,-12.4024260924821,3.93296540091676));
#42921=CARTESIAN_POINT('Ctrl Pts',(370.835363599504,-12.408278577216,3.93471172321431));
#42922=CARTESIAN_POINT('Ctrl Pts',(370.719359583573,-12.4141310619499,3.93131957442268));
#42923=CARTESIAN_POINT('Ctrl Pts',(370.603344931632,-12.4199840832781,3.92792711461654));
#42924=CARTESIAN_POINT('Ctrl Pts',(370.48749400721,-12.4258371046063,3.91939525923777));
#42925=CARTESIAN_POINT('Ctrl Pts',(370.372293007109,-12.4316901259344,3.90576779155804));
#42926=CARTESIAN_POINT('Ctrl Pts',(370.257053585249,-12.4375450993582,3.89213577885466));
#42927=CARTESIAN_POINT('Ctrl Pts',(370.142464928797,-12.443400072782,3.87340482300757));
#42928=CARTESIAN_POINT('Ctrl Pts',(370.029005416085,-12.4492550462058,3.84967022984951));
#42929=CARTESIAN_POINT('Ctrl Pts',(369.915417311589,-12.45511665549,3.8259087365787));
#42930=CARTESIAN_POINT('Ctrl Pts',(369.802961309736,-12.4609782647741,3.79713237170392));
#42931=CARTESIAN_POINT('Ctrl Pts',(369.692103038645,-12.4668398740583,3.76348698913067));
#42932=CARTESIAN_POINT('Ctrl Pts',(369.581170015007,-12.4727054358686,3.72981891922885));
#42933=CARTESIAN_POINT('Ctrl Pts',(369.471837256076,-12.4785709976789,3.69127543104224));
#42934=CARTESIAN_POINT('Ctrl Pts',(369.364551107941,-12.4844365594893,3.6480508102905));
#42935=CARTESIAN_POINT('Ctrl Pts',(369.257108081144,-12.4903106981896,3.60476298454168));
#42936=CARTESIAN_POINT('Ctrl Pts',(369.151718012278,-12.4961848368899,3.55678053593318));
#42937=CARTESIAN_POINT('Ctrl Pts',(369.048803392988,-12.5020589755902,3.50434403452155));
#42938=CARTESIAN_POINT('Ctrl Pts',(369.022777965861,-12.5035444493716,3.49108369934611));
#42939=CARTESIAN_POINT('Ctrl Pts',(368.9969107006,-12.505029923153,3.47753874390215));
#42940=CARTESIAN_POINT('Ctrl Pts',(368.971208127801,-12.5065153969343,3.46371349147624));
#42941=CARTESIAN_POINT('Ctrl Pts',(368.869577973802,-12.5123890863249,3.40904727015684));
#42942=CARTESIAN_POINT('Ctrl Pts',(368.770186568244,-12.5182627757155,3.34981325754346));
#42943=CARTESIAN_POINT('Ctrl Pts',(368.67347249404,-12.524136465106,3.28621915484853));
#42944=CARTESIAN_POINT('Ctrl Pts',(368.576883286792,-12.5300025710118,3.22270715811459));
#42945=CARTESIAN_POINT('Ctrl Pts',(368.482964878732,-12.5358686769175,3.1548464910175));
#42946=CARTESIAN_POINT('Ctrl Pts',(368.392132013744,-12.5417347828233,3.08289106610039));
#42947=CARTESIAN_POINT('Ctrl Pts',(368.301392160452,-12.5475948819113,3.01100932262175));
#42948=CARTESIAN_POINT('Ctrl Pts',(368.21373188753,-12.5534549809994,2.93504141652399));
#42949=CARTESIAN_POINT('Ctrl Pts',(368.12953708023,-12.5593150800874,2.85528456901245));
#42950=CARTESIAN_POINT('Ctrl Pts',(368.042304716361,-12.5653865981815,2.77265027639719));
#42951=CARTESIAN_POINT('Ctrl Pts',(367.958792968798,-12.5714581162756,2.68594873601823));
#42952=CARTESIAN_POINT('Ctrl Pts',(367.879393897138,-12.5775296343697,2.59555647477586));
#42953=CARTESIAN_POINT('Ctrl Pts',(367.802847697578,-12.5833829979665,2.50841207971957));
#42954=CARTESIAN_POINT('Ctrl Pts',(367.730124012735,-12.5892363615633,2.4178379575032));
#42955=CARTESIAN_POINT('Ctrl Pts',(367.661536093058,-12.59508972516,2.32420844640926));
#42956=CARTESIAN_POINT('Ctrl Pts',(367.592958471627,-12.6009422098939,2.23059299347138));
#42957=CARTESIAN_POINT('Ctrl Pts',(367.528515624721,-12.6067946946278,2.13392339703362));
#42958=CARTESIAN_POINT('Ctrl Pts',(367.468479193618,-12.6126471793617,2.03460539601712));
#42959=CARTESIAN_POINT('Ctrl Pts',(367.408437257981,-12.6185002006899,1.93527828887332));
#42960=CARTESIAN_POINT('Ctrl Pts',(367.352802755018,-12.6243532220181,1.83330264802757));
#42961=CARTESIAN_POINT('Ctrl Pts',(367.301802465215,-12.6302062433463,1.72911076379639));
#42962=CARTESIAN_POINT('Ctrl Pts',(367.250785165829,-12.6360612167701,1.62488412955972));
#42963=CARTESIAN_POINT('Ctrl Pts',(367.204405334497,-12.6419161901939,1.51844015302647));
#42964=CARTESIAN_POINT('Ctrl Pts',(367.162842218422,-12.6477711636177,1.41023248546389));
#42965=CARTESIAN_POINT('Ctrl Pts',(367.121231995895,-12.6536327729019,1.30190217840888));
#42966=CARTESIAN_POINT('Ctrl Pts',(367.084449532938,-12.6594943821861,1.19180457649475));
#42967=CARTESIAN_POINT('Ctrl Pts',(367.052624688804,-12.6653559914702,1.08041001947464));
#42968=CARTESIAN_POINT('Ctrl Pts',(367.020778384944,-12.6712215532806,0.968940348286627));
#42969=CARTESIAN_POINT('Ctrl Pts',(366.993896452045,-12.6770871150909,0.856172381466249));
#42970=CARTESIAN_POINT('Ctrl Pts',(366.972057598752,-12.6829526769013,0.74258651127268));
#42971=CARTESIAN_POINT('Ctrl Pts',(366.950186811699,-12.6888268156016,0.628834550678171));
#42972=CARTESIAN_POINT('Ctrl Pts',(366.933373881095,-12.6947009543019,0.514262707040079));
#42973=CARTESIAN_POINT('Ctrl Pts',(366.921645690772,-12.7005750930023,0.399356418718606));
#42974=CARTESIAN_POINT('Ctrl Pts',(366.918679822903,-12.7020605667835,0.370298494262007));
#42975=CARTESIAN_POINT('Ctrl Pts',(366.916038864731,-12.7035460405648,0.341219179107332));
#42976=CARTESIAN_POINT('Ctrl Pts',(366.913722723663,-12.705031514346,0.312126304660802));
#42977=CARTESIAN_POINT('Ctrl Pts',(366.905508391466,-12.7102998355524,0.208946693323902));
#42978=CARTESIAN_POINT('Ctrl Pts',(366.901366522409,-12.7155681567587,0.105438589692428));
#42979=CARTESIAN_POINT('Ctrl Pts',(366.901318279586,-12.720836477965,0.00183132919630113));
#42980=CARTESIAN_POINT('',(366.901318610208,-13.9708364779208,0.0024401713694973));
#42981=CARTESIAN_POINT('Ctrl Pts',(366.901318279586,-12.7208364780083,0.00183132834482709));
#42982=CARTESIAN_POINT('Ctrl Pts',(366.901265096517,-12.7266442978278,-0.112385758538794));
#42983=CARTESIAN_POINT('Ctrl Pts',(366.906191542405,-12.7324521176473,-0.226804680662638));
#42984=CARTESIAN_POINT('Ctrl Pts',(366.916124073898,-12.7382599374667,-0.340949420952398));
#42985=CARTESIAN_POINT('Ctrl Pts',(366.926044537002,-12.7440607005732,-0.454955471218333));
#42986=CARTESIAN_POINT('Ctrl Pts',(366.940958958238,-12.7498614636797,-0.568687584188307));
#42987=CARTESIAN_POINT('Ctrl Pts',(366.960841789125,-12.7556622267863,-0.681668673808639));
#42988=CARTESIAN_POINT('Ctrl Pts',(366.980706057939,-12.7614575744574,-0.794544287343653));
#42989=CARTESIAN_POINT('Ctrl Pts',(367.005529440934,-12.7672529221286,-0.906669857240528));
#42990=CARTESIAN_POINT('Ctrl Pts',(367.03523455997,-12.7730482697998,-1.01757315752793));
#42991=CARTESIAN_POINT('Ctrl Pts',(367.064921968539,-12.778840162231,-1.12841033624065));
#42992=CARTESIAN_POINT('Ctrl Pts',(367.09948521823,-12.7846320546623,-1.23802628648387));
#42993=CARTESIAN_POINT('Ctrl Pts',(367.138795941476,-12.7904239470935,-1.34595943467496));
#42994=CARTESIAN_POINT('Ctrl Pts',(367.178095158455,-12.7962141442351,-1.45386099078354));
#42995=CARTESIAN_POINT('Ctrl Pts',(367.22213894297,-12.8020043413767,-1.56008032651987));
#42996=CARTESIAN_POINT('Ctrl Pts',(367.270749445553,-12.8077945385184,-1.66417222782126));
#42997=CARTESIAN_POINT('Ctrl Pts',(367.319358096353,-12.8135845150864,-1.76826016381273));
#42998=CARTESIAN_POINT('Ctrl Pts',(367.372532939982,-12.8193744916544,-1.87022044337752));
#42999=CARTESIAN_POINT('Ctrl Pts',(367.43004883268,-12.8251644682224,-1.96962977124236));
#43000=CARTESIAN_POINT('Ctrl Pts',(367.487577179154,-12.83095569848,-2.06906062396677));
#43001=CARTESIAN_POINT('Ctrl Pts',(367.5494482303,-12.8367469287375,-2.16593906156535));
#43002=CARTESIAN_POINT('Ctrl Pts',(367.61539237484,-12.842538158995,-2.25986897067346));
#43003=CARTESIAN_POINT('Ctrl Pts',(367.681406160354,-12.8483355051392,-2.35389807540132));
#43004=CARTESIAN_POINT('Ctrl Pts',(367.751501382006,-12.8541328512834,-2.44497208956146));
#43005=CARTESIAN_POINT('Ctrl Pts',(367.825366830433,-12.8599301974275,-2.53272634574798));
#43006=CARTESIAN_POINT('Ctrl Pts',(367.899276057181,-12.8657309795229,-2.62053261182553));
#43007=CARTESIAN_POINT('Ctrl Pts',(367.976959672241,-12.8715317616182,-2.70501489314302));
#43008=CARTESIAN_POINT('Ctrl Pts',(368.058069457938,-12.8773325437136,-2.78584526628359));
#43009=CARTESIAN_POINT('Ctrl Pts',(368.139302682601,-12.8831421538749,-2.86679865315757));
#43010=CARTESIAN_POINT('Ctrl Pts',(368.223972174227,-12.8889517640361,-2.94408875383431));
#43011=CARTESIAN_POINT('Ctrl Pts',(368.311696438841,-12.8947613741974,-3.01742774556374));
#43012=CARTESIAN_POINT('Ctrl Pts',(368.355920173985,-12.8976901267175,-3.05439954760996));
#43013=CARTESIAN_POINT('Ctrl Pts',(368.400919777681,-12.9006188792376,-3.09036789966459));
#43014=CARTESIAN_POINT('Ctrl Pts',(368.44664376155,-12.9035476317577,-3.12530021469093));
#43015=CARTESIAN_POINT('Ctrl Pts',(368.53834440102,-12.9094213211482,-3.1953578814793));
#43016=CARTESIAN_POINT('Ctrl Pts',(368.633283764046,-12.9152950105388,-3.26149287295319));
#43017=CARTESIAN_POINT('Ctrl Pts',(368.731091819641,-12.9211686999294,-3.32339122759557));
#43018=CARTESIAN_POINT('Ctrl Pts',(368.828773595847,-12.9270348058351,-3.38520966564688));
#43019=CARTESIAN_POINT('Ctrl Pts',(368.929316353155,-12.9329009117408,-3.4428021257796));
#43020=CARTESIAN_POINT('Ctrl Pts',(369.032317785736,-12.9387670176466,-3.49589541559407));
#43021=CARTESIAN_POINT('Ctrl Pts',(369.135213746161,-12.9446271167346,-3.54893433855632));
#43022=CARTESIAN_POINT('Ctrl Pts',(369.240563008995,-12.9504872158226,-3.59748306692291));
#43023=CARTESIAN_POINT('Ctrl Pts',(369.347935707373,-12.9563473149107,-3.64131255407921));
#43024=CARTESIAN_POINT('Ctrl Pts',(369.459182167752,-12.9624188330048,-3.68672330914106));
#43025=CARTESIAN_POINT('Ctrl Pts',(369.572600440471,-12.9684903510989,-3.7270676333852));
#43026=CARTESIAN_POINT('Ctrl Pts',(369.687685859732,-12.974561869193,-3.7621435474341));
#43027=CARTESIAN_POINT('Ctrl Pts',(369.798636167905,-12.9804152327898,-3.79595915585919));
#43028=CARTESIAN_POINT('Ctrl Pts',(369.911135451532,-12.9862685963865,-3.8248783041136));
#43029=CARTESIAN_POINT('Ctrl Pts',(370.024713526672,-12.9921219599832,-3.84876991185864));
#43030=CARTESIAN_POINT('Ctrl Pts',(370.138274548446,-12.9979744447171,-3.87265793235914));
#43031=CARTESIAN_POINT('Ctrl Pts',(370.252913635475,-13.003826929451,-3.8915198282893));
#43032=CARTESIAN_POINT('Ctrl Pts',(370.368149148131,-13.0096794141849,-3.90527537292721));
#43033=CARTESIAN_POINT('Ctrl Pts',(370.483395226336,-13.0155324355131,-3.91903217876389));
#43034=CARTESIAN_POINT('Ctrl Pts',(370.599237428621,-13.0213854568412,-3.92768165363084));
#43035=CARTESIAN_POINT('Ctrl Pts',(370.715188418144,-13.0272384781694,-3.93119538788108));
#43036=CARTESIAN_POINT('Ctrl Pts',(370.83117807956,-13.0330934515932,-3.93471029402954));
#43037=CARTESIAN_POINT('Ctrl Pts',(370.947276187628,-13.038948425017,-3.9330860410911));
#43038=CARTESIAN_POINT('Ctrl Pts',(371.062995538878,-13.0448033984408,-3.92634633165287));
#43039=CARTESIAN_POINT('Ctrl Pts',(371.178846043149,-13.0506650077249,-3.91959898361965));
#43040=CARTESIAN_POINT('Ctrl Pts',(371.294316521124,-13.0565266170091,-3.90772463123588));
#43041=CARTESIAN_POINT('Ctrl Pts',(371.408924924247,-13.0623882262932,-3.89079885292595));
#43042=CARTESIAN_POINT('Ctrl Pts',(371.523610608658,-13.0682537881036,-3.87386166143937));
#43043=CARTESIAN_POINT('Ctrl Pts',(371.637432656077,-13.0741193499139,-3.85186633969296));
#43044=CARTESIAN_POINT('Ctrl Pts',(371.749920945379,-13.0799849117243,-3.82493921227999));
#43045=CARTESIAN_POINT('Ctrl Pts',(371.862573720149,-13.0858590504246,-3.7979727108025));
#43046=CARTESIAN_POINT('Ctrl Pts',(371.973888448911,-13.0917331891249,-3.76606012471782));
#43047=CARTESIAN_POINT('Ctrl Pts',(372.083411777131,-13.0976073278252,-3.72937707523109));
#43048=CARTESIAN_POINT('Ctrl Pts',(372.111108438858,-13.0990928016066,-3.72010053087057));
#43049=CARTESIAN_POINT('Ctrl Pts',(372.138690650169,-13.100578275388,-3.71051915052909));
#43050=CARTESIAN_POINT('Ctrl Pts',(372.166151314215,-13.1020637491693,-3.70063624694249));
#43051=CARTESIAN_POINT('Ctrl Pts',(372.274733110197,-13.1079374385599,-3.6615584074864));
#43052=CARTESIAN_POINT('Ctrl Pts',(372.381774394173,-13.1138111279505,-3.61763252361551));
#43053=CARTESIAN_POINT('Ctrl Pts',(372.4868107445,-13.119684817341,-3.56899933374663));
#43054=CARTESIAN_POINT('Ctrl Pts',(372.59171148303,-13.1255509232468,-3.52042893389471));
#43055=CARTESIAN_POINT('Ctrl Pts',(372.69461206422,-13.1314170291526,-3.46716348634923));
#43056=CARTESIAN_POINT('Ctrl Pts',(372.795064828534,-13.1372831350583,-3.40939295165738));
#43057=CARTESIAN_POINT('Ctrl Pts',(372.895414730498,-13.1431432341464,-3.35168157325728));
#43058=CARTESIAN_POINT('Ctrl Pts',(372.993321445276,-13.1490033332344,-3.28947448839614));
#43059=CARTESIAN_POINT('Ctrl Pts',(373.088359468285,-13.1548634323224,-3.22300874922352));
#43060=CARTESIAN_POINT('Ctrl Pts',(373.186826246349,-13.1609349504166,-3.15414507781414));
#43061=CARTESIAN_POINT('Ctrl Pts',(373.282213022964,-13.1670064685107,-3.08070985512041));
#43062=CARTESIAN_POINT('Ctrl Pts',(373.374076489147,-13.1730779866048,-3.00301766082958));
#43063=CARTESIAN_POINT('Ctrl Pts',(373.462639227575,-13.1789313502015,-2.92811700916959));
#43064=CARTESIAN_POINT('Ctrl Pts',(373.547927146423,-13.1847847137983,-2.84926032365174));
#43065=CARTESIAN_POINT('Ctrl Pts',(373.629575206669,-13.190638077395,-2.7667716436326));
#43066=CARTESIAN_POINT('Ctrl Pts',(373.711211007734,-13.196490562129,-2.68429534901106));
#43067=CARTESIAN_POINT('Ctrl Pts',(373.789207746309,-13.2023430468629,-2.59818843776364));
#43068=CARTESIAN_POINT('Ctrl Pts',(373.863236905828,-13.2081955315968,-2.50881214377893));
#43069=CARTESIAN_POINT('Ctrl Pts',(373.937272852827,-13.214048552925,-2.41942765518805));
#43070=CARTESIAN_POINT('Ctrl Pts',(374.007340234067,-13.2199015742532,-2.3267735061606));
#43071=CARTESIAN_POINT('Ctrl Pts',(374.073150986761,-13.2257545955814,-2.23124380852941));
#43072=CARTESIAN_POINT('Ctrl Pts',(374.138983688613,-13.2316095690052,-2.13568224989932));
#43073=CARTESIAN_POINT('Ctrl Pts',(374.200556704717,-13.237464542429,-2.03724357567743));
#43074=CARTESIAN_POINT('Ctrl Pts',(374.257625834908,-13.2433195158529,-1.93635003616015));
#43075=CARTESIAN_POINT('Ctrl Pts',(374.314759645629,-13.249181125137,-1.83534214677508));
#43076=CARTESIAN_POINT('Ctrl Pts',(374.367379178491,-13.2550427344212,-1.73187419864738));
#43077=CARTESIAN_POINT('Ctrl Pts',(374.415286619531,-13.2609043437053,-1.62639223274409));
#43078=CARTESIAN_POINT('Ctrl Pts',(374.463226364911,-13.2667699055157,-1.52083913957675));
#43079=CARTESIAN_POINT('Ctrl Pts',(374.506447537913,-13.272635467326,-1.41326970682986));
#43080=CARTESIAN_POINT('Ctrl Pts',(374.544801432953,-13.2785010291364,-1.30414746273616));
#43081=CARTESIAN_POINT('Ctrl Pts',(374.583211410794,-13.2843751678367,-1.19486565515765));
#43082=CARTESIAN_POINT('Ctrl Pts',(374.61673978746,-13.290249306537,-1.0840268986315));
#43083=CARTESIAN_POINT('Ctrl Pts',(374.645288371022,-13.2961234452374,-0.972107356456605));
#43084=CARTESIAN_POINT('Ctrl Pts',(374.652507841745,-13.2976089190186,-0.943804731341924));
#43085=CARTESIAN_POINT('Ctrl Pts',(374.659409111743,-13.2990943927998,-0.915433025324876));
#43086=CARTESIAN_POINT('Ctrl Pts',(374.665991117463,-13.300579866581,-0.886999997809702));
#43087=CARTESIAN_POINT('Ctrl Pts',(374.692016926641,-13.3064535559716,-0.774573394143596));
#43088=CARTESIAN_POINT('Ctrl Pts',(374.713133759842,-13.3123272453622,-0.660813123817876));
#43089=CARTESIAN_POINT('Ctrl Pts',(374.729208113275,-13.3182009347527,-0.546185739618226));
#43090=CARTESIAN_POINT('Ctrl Pts',(374.745261713206,-13.3240670406585,-0.431706350140542));
#43091=CARTESIAN_POINT('Ctrl Pts',(374.7562857234,-13.3299331465642,-0.316362478562879));
#43092=CARTESIAN_POINT('Ctrl Pts',(374.762197088704,-13.33579925247,-0.200633276123563));
#43093=CARTESIAN_POINT('Ctrl Pts',(374.768102400844,-13.341659351558,-0.0850225789127362));
#43094=CARTESIAN_POINT('Ctrl Pts',(374.768905460556,-13.3475194506461,0.0309722541648994));
#43095=CARTESIAN_POINT('Ctrl Pts',(374.76457479454,-13.3533795497341,0.146865160044948));
#43096=CARTESIAN_POINT('Ctrl Pts',(374.760087887974,-13.3594510678282,0.26693921757465));
#43097=CARTESIAN_POINT('Ctrl Pts',(374.750089772911,-13.3655225859223,0.386903407149259));
#43098=CARTESIAN_POINT('Ctrl Pts',(374.734604471114,-13.3715941040164,0.506214676110398));
#43099=CARTESIAN_POINT('Ctrl Pts',(374.719675568586,-13.3774474676132,0.621238995826725));
#43100=CARTESIAN_POINT('Ctrl Pts',(374.699647068922,-13.38330083121,0.735656062532786));
#43101=CARTESIAN_POINT('Ctrl Pts',(374.674593373812,-13.3891541948067,0.848983466255619));
#43102=CARTESIAN_POINT('Ctrl Pts',(374.649543440429,-13.3950066795406,0.962293854250114));
#43103=CARTESIAN_POINT('Ctrl Pts',(374.619469901018,-13.4008591642745,1.07451450128166));
#43104=CARTESIAN_POINT('Ctrl Pts',(374.584498211296,-13.4067116490084,1.18517352397492));
#43105=CARTESIAN_POINT('Ctrl Pts',(374.549523315139,-13.4125646703366,1.29584269261457));
#43106=CARTESIAN_POINT('Ctrl Pts',(374.509649500417,-13.4184176916647,1.40494955832535));
#43107=CARTESIAN_POINT('Ctrl Pts',(374.465051780819,-13.4242707129929,1.51203840791429));
#43108=CARTESIAN_POINT('Ctrl Pts',(374.420439187021,-13.4301256864167,1.6191629737025));
#43109=CARTESIAN_POINT('Ctrl Pts',(374.371099714255,-13.4359806598405,1.72426780385694));
#43110=CARTESIAN_POINT('Ctrl Pts',(374.317255799529,-13.4418356332643,1.8269187891613));
#43111=CARTESIAN_POINT('Ctrl Pts',(374.263350859641,-13.4476972425485,1.92968611617289));
#43112=CARTESIAN_POINT('Ctrl Pts',(374.204931480124,-13.4535588518326,2.02999368131795));
#43113=CARTESIAN_POINT('Ctrl Pts',(374.142265235874,-13.4594204611168,2.1274334569198));
#43114=CARTESIAN_POINT('Ctrl Pts',(374.079556735314,-13.4652860229271,2.22493893687804));
#43115=CARTESIAN_POINT('Ctrl Pts',(374.012595905819,-13.4711515847375,2.31957244030342));
#43116=CARTESIAN_POINT('Ctrl Pts',(373.941691639087,-13.4770171465478,2.41095772566206));
#43117=CARTESIAN_POINT('Ctrl Pts',(373.870683692927,-13.4828912852482,2.50247663872151));
#43118=CARTESIAN_POINT('Ctrl Pts',(373.795721067923,-13.4887654239485,2.59073754083909));
#43119=CARTESIAN_POINT('Ctrl Pts',(373.717150657053,-13.4946395626489,2.67539978791368));
#43120=CARTESIAN_POINT('Ctrl Pts',(373.697281482816,-13.4961250364301,2.6968094880769));
#43121=CARTESIAN_POINT('Ctrl Pts',(373.677181759714,-13.4976105102114,2.71798925108762));
#43122=CARTESIAN_POINT('Ctrl Pts',(373.656857431475,-13.4990959839926,2.73893397678799));
#43123=CARTESIAN_POINT('Ctrl Pts',(373.576493312867,-13.5049696733832,2.82175119960748));
#43124=CARTESIAN_POINT('Ctrl Pts',(373.492347301133,-13.5108433627738,2.90116636477356));
#43125=CARTESIAN_POINT('Ctrl Pts',(373.404739070565,-13.5167170521643,2.97681436529804));
#43126=CARTESIAN_POINT('Ctrl Pts',(373.317243950452,-13.5225831580701,3.05236469714692));
#43127=CARTESIAN_POINT('Ctrl Pts',(373.226295810814,-13.5284492639758,3.12415726923927));
#43128=CARTESIAN_POINT('Ctrl Pts',(373.132252261207,-13.5343153698816,3.19186253723524));
#43129=CARTESIAN_POINT('Ctrl Pts',(373.038305010998,-13.5401754689696,3.25949847589931));
#43130=CARTESIAN_POINT('Ctrl Pts',(372.941268988835,-13.5460355680577,3.32305519551618));
#43131=CARTESIAN_POINT('Ctrl Pts',(372.841535575353,-13.5518956671457,3.38224274941507));
#43132=CARTESIAN_POINT('Ctrl Pts',(372.738204007841,-13.5579671852398,3.44356565523023));
#43133=CARTESIAN_POINT('Ctrl Pts',(372.63197708469,-13.5640387033339,3.50019788883422));
#43134=CARTESIAN_POINT('Ctrl Pts',(372.523324159736,-13.570110221428,3.55186524189211));
#43135=CARTESIAN_POINT('Ctrl Pts',(372.41857522121,-13.5759635850248,3.60167614566312));
#43136=CARTESIAN_POINT('Ctrl Pts',(372.311572022044,-13.5818169486215,3.64687262031137));
#43137=CARTESIAN_POINT('Ctrl Pts',(372.202760268987,-13.5876703122183,3.68725566712433));
#43138=CARTESIAN_POINT('Ctrl Pts',(372.093964853649,-13.5935227969522,3.72763265055867));
#43139=CARTESIAN_POINT('Ctrl Pts',(371.983361811586,-13.5993752816861,3.76319749948606));
#43140=CARTESIAN_POINT('Ctrl Pts',(371.871415680838,-13.60522776642,3.79379982286338));
#43141=CARTESIAN_POINT('Ctrl Pts',(371.759459286133,-13.6110807877482,3.82440495206294));
#43142=CARTESIAN_POINT('Ctrl Pts',(371.646159956491,-13.6169338090764,3.85004654227227));
#43143=CARTESIAN_POINT('Ctrl Pts',(371.53199550787,-13.6227868304046,3.87062461241184));
#43144=CARTESIAN_POINT('Ctrl Pts',(371.4177929832,-13.6286418038284,3.89120954573506));
#43145=CARTESIAN_POINT('Ctrl Pts',(371.302725172188,-13.6344967772522,3.90672752767294));
#43146=CARTESIAN_POINT('Ctrl Pts',(371.187277445431,-13.6403517506759,3.91713013905194));
#43147=CARTESIAN_POINT('Ctrl Pts',(371.071698873503,-13.6462133599601,3.92754454045484));
#43148=CARTESIAN_POINT('Ctrl Pts',(370.955739938115,-13.6520749692443,3.93283196250979));
#43149=CARTESIAN_POINT('Ctrl Pts',(370.839888563019,-13.6579365785284,3.93299605481526));
#43150=CARTESIAN_POINT('Ctrl Pts',(370.723959068491,-13.6638021403388,3.93316025776937));
#43151=CARTESIAN_POINT('Ctrl Pts',(370.60813769042,-13.6696677021491,3.92819426955626));
#43152=CARTESIAN_POINT('Ctrl Pts',(370.492908040648,-13.6755332639594,3.91815369018076));
#43153=CARTESIAN_POINT('Ctrl Pts',(370.377509896867,-13.6814074026597,3.90809842901557));
#43154=CARTESIAN_POINT('Ctrl Pts',(370.262705616231,-13.6872815413601,3.89295382146564));
#43155=CARTESIAN_POINT('Ctrl Pts',(370.148969498636,-13.6931556800604,3.87282669801567));
#43156=CARTESIAN_POINT('Ctrl Pts',(370.120207491251,-13.6946411538417,3.86773687707284));
#43157=CARTESIAN_POINT('Ctrl Pts',(370.091513719128,-13.696126627623,3.86232867299299));
#43158=CARTESIAN_POINT('Ctrl Pts',(370.062895690121,-13.6976121014043,3.85660431549224));
#43159=CARTESIAN_POINT('Ctrl Pts',(369.949737574861,-13.7034857907949,3.83396972015764));
#43160=CARTESIAN_POINT('Ctrl Pts',(369.83738803511,-13.7093594801855,3.80631288254161));
#43161=CARTESIAN_POINT('Ctrl Pts',(369.72632717161,-13.715233169576,3.77370449948814));
#43162=CARTESIAN_POINT('Ctrl Pts',(369.615409698119,-13.7210992754818,3.7411382169206));
#43163=CARTESIAN_POINT('Ctrl Pts',(369.505777984912,-13.7269653813875,3.70363321764485));
#43164=CARTESIAN_POINT('Ctrl Pts',(369.397902814227,-13.7328314872933,3.66131135465738));
#43165=CARTESIAN_POINT('Ctrl Pts',(369.290138106343,-13.7386915863813,3.61903282871851));
#43166=CARTESIAN_POINT('Ctrl Pts',(369.184126745581,-13.7445516854694,3.57194740002689));
#43167=CARTESIAN_POINT('Ctrl Pts',(369.080324547569,-13.7504117845574,3.52022676595108));
#43168=CARTESIAN_POINT('Ctrl Pts',(368.972777403064,-13.7564833026515,3.46664016939145));
#43169=CARTESIAN_POINT('Ctrl Pts',(368.867602267396,-13.7625548207456,3.40807772474953));
#43170=CARTESIAN_POINT('Ctrl Pts',(368.765284001161,-13.7686263388397,3.34478518279095));
#43171=CARTESIAN_POINT('Ctrl Pts',(368.666642112003,-13.7744797024365,3.28376679244713));
#43172=CARTESIAN_POINT('Ctrl Pts',(368.570655707714,-13.7803330660332,3.21835260328292));
#43173=CARTESIAN_POINT('Ctrl Pts',(368.477733630341,-13.7861864296299,3.14880926708183));
#43174=CARTESIAN_POINT('Ctrl Pts',(368.384825504906,-13.7920389143638,3.0792763725786));
#43175=CARTESIAN_POINT('Ctrl Pts',(368.294981122219,-13.7978913990977,3.00561581126936));
#43176=CARTESIAN_POINT('Ctrl Pts',(368.208578687543,-13.8037438838316,2.92813640969977));
#43177=CARTESIAN_POINT('Ctrl Pts',(368.122168330924,-13.8095969051598,2.85064990430941));
#43178=CARTESIAN_POINT('Ctrl Pts',(368.039200857267,-13.815449926488,2.76934413845824));
#43179=CARTESIAN_POINT('Ctrl Pts',(367.960019310032,-13.8213029478161,2.68456642395093));
#43180=CARTESIAN_POINT('Ctrl Pts',(367.880811354222,-13.8271579212399,2.599760434439));
#43181=CARTESIAN_POINT('Ctrl Pts',(367.805392117466,-13.8330128946637,2.51148049548522));
#43182=CARTESIAN_POINT('Ctrl Pts',(367.734065410794,-13.8388678680875,2.42010821931692));
#43183=CARTESIAN_POINT('Ctrl Pts',(367.66265786446,-13.8447294773717,2.32863238440924));
#43184=CARTESIAN_POINT('Ctrl Pts',(367.595352360455,-13.8505910866558,2.23405754283356));
#43185=CARTESIAN_POINT('Ctrl Pts',(367.532410340101,-13.85645269594,2.13679567923062));
#43186=CARTESIAN_POINT('Ctrl Pts',(367.469425877479,-13.8623182577503,2.03946823123901));
#43187=CARTESIAN_POINT('Ctrl Pts',(367.410810965714,-13.8681838195607,1.93945050893014));
#43188=CARTESIAN_POINT('Ctrl Pts',(367.356781054262,-13.874049381371,1.83717903642075));
#43189=CARTESIAN_POINT('Ctrl Pts',(367.302672137828,-13.8799235200713,1.7347580179346));
#43190=CARTESIAN_POINT('Ctrl Pts',(367.253161777958,-13.8857976587717,1.63007704423034));
#43191=CARTESIAN_POINT('Ctrl Pts',(367.208417326641,-13.891671797472,1.52359258705272));
#43192=CARTESIAN_POINT('Ctrl Pts',(367.197102185361,-13.8931572712533,1.49666440620367));
#43193=CARTESIAN_POINT('Ctrl Pts',(367.186091574914,-13.8946427450346,1.46962096545369));
#43194=CARTESIAN_POINT('Ctrl Pts',(367.175387691731,-13.896128218816,1.44246978246126));
#43195=CARTESIAN_POINT('Ctrl Pts',(367.127536355304,-13.902768977543,1.32109136590888));
#43196=CARTESIAN_POINT('Ctrl Pts',(367.085685534993,-13.90940973627,1.19722064348745));
#43197=CARTESIAN_POINT('Ctrl Pts',(367.050069812319,-13.9160504949971,1.07142697600303));
#43198=CARTESIAN_POINT('Ctrl Pts',(367.014571606434,-13.9226693420351,0.946048374301991));
#43199=CARTESIAN_POINT('Ctrl Pts',(366.985267539514,-13.9292881890731,0.81875967944162));
#43200=CARTESIAN_POINT('Ctrl Pts',(366.962343410939,-13.9359070361111,0.690147026575956));
#43201=CARTESIAN_POINT('Ctrl Pts',(366.93956000388,-13.9424852528505,0.562323872313213));
#43202=CARTESIAN_POINT('Ctrl Pts',(366.923078544681,-13.9490634695899,0.433193162774451));
#43203=CARTESIAN_POINT('Ctrl Pts',(366.913033877604,-13.9556416863293,0.303349604497033));
#43204=CARTESIAN_POINT('Ctrl Pts',(366.905299936483,-13.9607066168598,0.203375914276909));
#43205=CARTESIAN_POINT('Ctrl Pts',(366.901380988686,-13.9657715473903,0.102980039154434));
#43206=CARTESIAN_POINT('Ctrl Pts',(366.901318610208,-13.9708364779208,0.00244017136950739));
#43207=CARTESIAN_POINT('',(366.901319086285,-15.2208364780051,-0.00311436343212247));
#43208=CARTESIAN_POINT('Ctrl Pts',(366.901318610208,-13.9708364779651,0.00244017049049901));
#43209=CARTESIAN_POINT('Ctrl Pts',(366.901245969927,-13.9767346357568,-0.114639422405236));
#43210=CARTESIAN_POINT('Ctrl Pts',(366.906405595384,-13.9826327935485,-0.231739061658494));
#43211=CARTESIAN_POINT('Ctrl Pts',(366.916776250793,-13.9885309513401,-0.348363019306832));
#43212=CARTESIAN_POINT('Ctrl Pts',(366.927148018102,-13.9944297415088,-0.46499948091072));
#43213=CARTESIAN_POINT('Ctrl Pts',(366.942731891741,-14.0003285316774,-0.581159756870668));
#43214=CARTESIAN_POINT('Ctrl Pts',(366.963454737144,-14.006227321846,-0.696353169425402));
#43215=CARTESIAN_POINT('Ctrl Pts',(366.984184520303,-14.0121280868579,-0.811585147335559));
#43216=CARTESIAN_POINT('Ctrl Pts',(367.010056627378,-14.0180288518699,-0.925849220139976));
#43217=CARTESIAN_POINT('Ctrl Pts',(367.040946903125,-14.0239296168818,-1.0386654104878));
#43218=CARTESIAN_POINT('Ctrl Pts',(367.071876808775,-14.029837952132,-1.15162633553298));
#43219=CARTESIAN_POINT('Ctrl Pts',(367.107837636474,-14.0357462873822,-1.26313527712464));
#43220=CARTESIAN_POINT('Ctrl Pts',(367.148655325033,-14.0416546226323,-1.37272747779266));
#43221=CARTESIAN_POINT('Ctrl Pts',(367.189499302339,-14.0475667631625,-1.48239026162705));
#43222=CARTESIAN_POINT('Ctrl Pts',(367.235206215648,-14.0534789036927,-1.5901334729216));
#43223=CARTESIAN_POINT('Ctrl Pts',(367.285554573887,-14.0593910442229,-1.69551413654578));
#43224=CARTESIAN_POINT('Ctrl Pts',(367.335995824196,-14.0653140925759,-1.80108922613311));
#43225=CARTESIAN_POINT('Ctrl Pts',(367.39109544319,-14.071237140929,-1.90429269979353));
#43226=CARTESIAN_POINT('Ctrl Pts',(367.450586467606,-14.0771601892821,-2.0047071880907));
#43227=CARTESIAN_POINT('Ctrl Pts',(367.509123319511,-14.0829882382639,-2.10351113521302));
#43228=CARTESIAN_POINT('Ctrl Pts',(367.571911478936,-14.0888162872458,-2.19961464379094));
#43229=CARTESIAN_POINT('Ctrl Pts',(367.638658335005,-14.0946443362276,-2.29265113866326));
#43230=CARTESIAN_POINT('Ctrl Pts',(367.705927896665,-14.1005180256182,-2.38641621760659));
#43231=CARTESIAN_POINT('Ctrl Pts',(367.777439788768,-14.1063917150087,-2.47737427957401));
#43232=CARTESIAN_POINT('Ctrl Pts',(367.852931686877,-14.1122654043993,-2.56511705914408));
#43233=CARTESIAN_POINT('Ctrl Pts',(367.928326117852,-14.118131510305,-2.65274655454247));
#43234=CARTESIAN_POINT('Ctrl Pts',(368.007690068925,-14.1239976162108,-2.73716871266057));
#43235=CARTESIAN_POINT('Ctrl Pts',(368.090718449835,-14.1298637221165,-2.81800484629188));
#43236=CARTESIAN_POINT('Ctrl Pts',(368.173661810741,-14.1357238212045,-2.89875820475225));
#43237=CARTESIAN_POINT('Ctrl Pts',(368.260261843529,-14.1415839202926,-2.97593255623396));
#43238=CARTESIAN_POINT('Ctrl Pts',(368.350174215594,-14.1474440193806,-3.04918339684968));
#43239=CARTESIAN_POINT('Ctrl Pts',(368.443330420921,-14.1535155374747,-3.12507696068299));
#43240=CARTESIAN_POINT('Ctrl Pts',(368.540042186724,-14.1595870555688,-3.19675822350987));
#43241=CARTESIAN_POINT('Ctrl Pts',(368.639885738655,-14.1656585736629,-3.26388674658754));
#43242=CARTESIAN_POINT('Ctrl Pts',(368.736141831973,-14.1715119372597,-3.32860328818311));
#43243=CARTESIAN_POINT('Ctrl Pts',(368.835308157173,-14.1773653008564,-3.38908837641716));
#43244=CARTESIAN_POINT('Ctrl Pts',(368.936973234927,-14.1832186644531,-3.44507944747595));
#43245=CARTESIAN_POINT('Ctrl Pts',(369.038623048013,-14.189071149187,-3.50106211166386));
#43246=CARTESIAN_POINT('Ctrl Pts',(369.142770505862,-14.1949236339209,-3.55255190110144));
#43247=CARTESIAN_POINT('Ctrl Pts',(369.248978334202,-14.2007761186548,-3.59933155036128));
#43248=CARTESIAN_POINT('Ctrl Pts',(369.355195900373,-14.206629139983,-3.64611548868689));
#43249=CARTESIAN_POINT('Ctrl Pts',(369.463473834451,-14.2124821613112,-3.68818826180188));
#43250=CARTESIAN_POINT('Ctrl Pts',(369.573354294008,-14.2183351826393,-3.72538050436855));
#43251=CARTESIAN_POINT('Ctrl Pts',(369.683271400821,-14.2241901560632,-3.76258515126637));
#43252=CARTESIAN_POINT('Ctrl Pts',(369.794791704764,-14.230045129487,-3.79490589851788));
#43253=CARTESIAN_POINT('Ctrl Pts',(369.907442286025,-14.2359001029108,-3.82222326440111));
#43254=CARTESIAN_POINT('Ctrl Pts',(370.020220542249,-14.2417617121949,-3.84957159100977));
#43255=CARTESIAN_POINT('Ctrl Pts',(370.134131230905,-14.2476233214791,-3.87190512047534));
#43256=CARTESIAN_POINT('Ctrl Pts',(370.248691226803,-14.2534849307632,-3.8891554937322));
#43257=CARTESIAN_POINT('Ctrl Pts',(370.363328471349,-14.2593504925736,-3.90641749904246));
#43258=CARTESIAN_POINT('Ctrl Pts',(370.478615485115,-14.2652160543839,-3.91858947974169));
#43259=CARTESIAN_POINT('Ctrl Pts',(370.594065744978,-14.2710816161943,-3.92565509494702));
#43260=CARTESIAN_POINT('Ctrl Pts',(370.709684821437,-14.2769557548946,-3.93273104181472));
#43261=CARTESIAN_POINT('Ctrl Pts',(370.825467208893,-14.2828298935949,-3.93468571446805));
#43262=CARTESIAN_POINT('Ctrl Pts',(370.940928037821,-14.2887040322952,-3.93155481566012));
#43263=CARTESIAN_POINT('Ctrl Pts',(370.970126196545,-14.2901895060766,-3.93076306246387));
#43264=CARTESIAN_POINT('Ctrl Pts',(370.999303827869,-14.2916749798579,-3.9296463438869));
#43265=CARTESIAN_POINT('Ctrl Pts',(371.028453177175,-14.2931604536392,-3.92820575784855));
#43266=CARTESIAN_POINT('Ctrl Pts',(371.143712177982,-14.2990341430298,-3.92250955840297));
#43267=CARTESIAN_POINT('Ctrl Pts',(371.258912228079,-14.3049078324204,-3.91172678479568));
#43268=CARTESIAN_POINT('Ctrl Pts',(371.373568050256,-14.3107815218109,-3.89585654574198));
#43269=CARTESIAN_POINT('Ctrl Pts',(371.488075840995,-14.3166476277167,-3.88000679665785));
#43270=CARTESIAN_POINT('Ctrl Pts',(371.602040395648,-14.3225137336225,-3.85908270064155));
#43271=CARTESIAN_POINT('Ctrl Pts',(371.714978108051,-14.3283798395282,-3.83313533749692));
#43272=CARTESIAN_POINT('Ctrl Pts',(371.827800173676,-14.3342399386162,-3.80721454412161));
#43273=CARTESIAN_POINT('Ctrl Pts',(371.939597088257,-14.3401000377043,-3.77628080694578));
#43274=CARTESIAN_POINT('Ctrl Pts',(372.049892696494,-14.3459601367923,-3.74043671252544));
#43275=CARTESIAN_POINT('Ctrl Pts',(372.164167518653,-14.3520316548864,-3.70329944495187));
#43276=CARTESIAN_POINT('Ctrl Pts',(372.276830214372,-14.3581031729805,-3.66089088357033));
#43277=CARTESIAN_POINT('Ctrl Pts',(372.3873649782,-14.3641746910746,-3.61338257420981));
#43278=CARTESIAN_POINT('Ctrl Pts',(372.493928139627,-14.3700280546714,-3.56758127637227));
#43279=CARTESIAN_POINT('Ctrl Pts',(372.598513241972,-14.3758814182681,-3.51704057673411));
#43280=CARTESIAN_POINT('Ctrl Pts',(372.700676583944,-14.3817347818649,-3.46196390626241));
#43281=CARTESIAN_POINT('Ctrl Pts',(372.802824586435,-14.3875872665988,-3.40689550536744));
#43282=CARTESIAN_POINT('Ctrl Pts',(372.902551187998,-14.3934397513327,-3.34729268384393));
#43283=CARTESIAN_POINT('Ctrl Pts',(372.999436768247,-14.3992922360666,-3.2834051050411));
#43284=CARTESIAN_POINT('Ctrl Pts',(373.096331231603,-14.4051452573948,-3.21951166860511));
#43285=CARTESIAN_POINT('Ctrl Pts',(373.190383810901,-14.410998278723,-3.15133292138041));
#43286=CARTESIAN_POINT('Ctrl Pts',(373.281203986385,-14.4168513000512,-3.07916177739099));
#43287=CARTESIAN_POINT('Ctrl Pts',(373.372054452151,-14.422706273475,-3.00696656293132));
#43288=CARTESIAN_POINT('Ctrl Pts',(373.459670047133,-14.4285612468988,-2.93077656089247));
#43289=CARTESIAN_POINT('Ctrl Pts',(373.543693995571,-14.4344162203226,-2.85092439732811));
#43290=CARTESIAN_POINT('Ctrl Pts',(373.627813174363,-14.4402778296068,-2.77098173159286));
#43291=CARTESIAN_POINT('Ctrl Pts',(373.708332282154,-14.446139438891,-2.68736890477264));
#43292=CARTESIAN_POINT('Ctrl Pts',(373.784931969527,-14.4520010481751,-2.60045483265399));
#43293=CARTESIAN_POINT('Ctrl Pts',(373.861583308632,-14.4578666099855,-2.5134821537382));
#43294=CARTESIAN_POINT('Ctrl Pts',(373.934309706187,-14.4637321717958,-2.42320411789462));
#43295=CARTESIAN_POINT('Ctrl Pts',(374.00283368201,-14.4695977336062,-2.3300206957733));
#43296=CARTESIAN_POINT('Ctrl Pts',(374.071457856692,-14.4754718723065,-2.23670101663432));
#43297=CARTESIAN_POINT('Ctrl Pts',(374.135867116908,-14.4813460110068,-2.14046781452352));
#43298=CARTESIAN_POINT('Ctrl Pts',(374.195828611582,-14.4872201497072,-2.04174788390892));
#43299=CARTESIAN_POINT('Ctrl Pts',(374.210991894706,-14.4887056234884,-2.01678322507182));
#43300=CARTESIAN_POINT('Ctrl Pts',(374.225870978771,-14.4901910972697,-1.99165964874743));
#43301=CARTESIAN_POINT('Ctrl Pts',(374.240462582516,-14.4916765710509,-1.96638426639299));
#43302=CARTESIAN_POINT('Ctrl Pts',(374.298159021989,-14.4975502604415,-1.8664432596576));
#43303=CARTESIAN_POINT('Ctrl Pts',(374.351549215539,-14.503423949832,-1.7637943094351));
#43304=CARTESIAN_POINT('Ctrl Pts',(374.40036934082,-14.5092976392226,-1.65884471479912));
#43305=CARTESIAN_POINT('Ctrl Pts',(374.449126434732,-14.5151637451284,-1.55403061994929));
#43306=CARTESIAN_POINT('Ctrl Pts',(374.493325021649,-14.5210298510341,-1.44692215891161));
#43307=CARTESIAN_POINT('Ctrl Pts',(374.53274585683,-14.5268959569399,-1.33795340058751));
#43308=CARTESIAN_POINT('Ctrl Pts',(374.572126325577,-14.5327560560279,-1.22909622488415));
#43309=CARTESIAN_POINT('Ctrl Pts',(374.606738634181,-14.5386161551159,-1.11838292713463));
#43310=CARTESIAN_POINT('Ctrl Pts',(374.636410858612,-14.5444762542039,-1.00626923752171));
#43311=CARTESIAN_POINT('Ctrl Pts',(374.667153589207,-14.550547772298,-0.890110741759438));
#43312=CARTESIAN_POINT('Ctrl Pts',(374.692592861174,-14.5566192903922,-0.772449309986367));
#43313=CARTESIAN_POINT('Ctrl Pts',(374.71259320278,-14.5626908084863,-0.653811374196177));
#43314=CARTESIAN_POINT('Ctrl Pts',(374.731874916127,-14.568544172083,-0.539436194252071));
#43315=CARTESIAN_POINT('Ctrl Pts',(374.746101748309,-14.5743975356797,-0.424153918084294));
#43316=CARTESIAN_POINT('Ctrl Pts',(374.755204109274,-14.5802508992765,-0.308447673230766));
#43317=CARTESIAN_POINT('Ctrl Pts',(374.764305103549,-14.5861033840104,-0.192758801280381));
#43318=CARTESIAN_POINT('Ctrl Pts',(374.768283124115,-14.5919558687443,-0.0766464989810674));
#43319=CARTESIAN_POINT('Ctrl Pts',(374.767120484841,-14.5978083534782,0.0394012784874696));
#43320=CARTESIAN_POINT('Ctrl Pts',(374.765957738968,-14.6036613748064,0.155459695978858));
#43321=CARTESIAN_POINT('Ctrl Pts',(374.759653400435,-14.6095143961346,0.271453163731976));
#43322=CARTESIAN_POINT('Ctrl Pts',(374.74824190272,-14.6153674174627,0.386894733452537));
#43323=CARTESIAN_POINT('Ctrl Pts',(374.736826599051,-14.6212223908865,0.50237480516592));
#43324=CARTESIAN_POINT('Ctrl Pts',(374.720300789811,-14.6270773643103,0.617302201915252));
#43325=CARTESIAN_POINT('Ctrl Pts',(374.698750571753,-14.6329323377342,0.731196802483956));
#43326=CARTESIAN_POINT('Ctrl Pts',(374.67717592929,-14.6387939470183,0.845220487953348));
#43327=CARTESIAN_POINT('Ctrl Pts',(374.650565588938,-14.6446555563025,0.958208634741834));
#43328=CARTESIAN_POINT('Ctrl Pts',(374.61905643117,-14.6505171655866,1.06969289827048));
#43329=CARTESIAN_POINT('Ctrl Pts',(374.587526026544,-14.6563827273969,1.18125233645673));
#43330=CARTESIAN_POINT('Ctrl Pts',(374.551090356411,-14.6622482892073,1.29130548088762));
#43331=CARTESIAN_POINT('Ctrl Pts',(374.509935094599,-14.6681138510176,1.39940233489322));
#43332=CARTESIAN_POINT('Ctrl Pts',(374.4687196537,-14.6739879897179,1.50765725301193));
#43333=CARTESIAN_POINT('Ctrl Pts',(374.422771011365,-14.6798621284183,1.61394979394341));
#43334=CARTESIAN_POINT('Ctrl Pts',(374.372321575551,-14.6857362671186,1.71785292176003));
#43335=CARTESIAN_POINT('Ctrl Pts',(374.359563736827,-14.6872217408999,1.74412832655396));
#43336=CARTESIAN_POINT('Ctrl Pts',(374.346518291478,-14.6887072146812,1.77025106732983));
#43337=CARTESIAN_POINT('Ctrl Pts',(374.333189436515,-14.6901926884625,1.79621453162981));
#43338=CARTESIAN_POINT('Ctrl Pts',(374.280486012888,-14.6960663778531,1.89887627276619));
#43339=CARTESIAN_POINT('Ctrl Pts',(374.223172626226,-14.7019400672436,1.99938744358015));
#43340=CARTESIAN_POINT('Ctrl Pts',(374.161448512536,-14.7078137566342,2.09730555138372));
#43341=CARTESIAN_POINT('Ctrl Pts',(374.099804090476,-14.71367986254,2.19509723771105));
#43342=CARTESIAN_POINT('Ctrl Pts',(374.033760484505,-14.7195459684457,2.29030217257058));
#43343=CARTESIAN_POINT('Ctrl Pts',(373.963563591468,-14.7254120743514,2.38250081000633));
#43344=CARTESIAN_POINT('Ctrl Pts',(373.893438579156,-14.7312721734395,2.47460503721192));
#43345=CARTESIAN_POINT('Ctrl Pts',(373.819168987959,-14.7371322725275,2.56370876344664));
#43346=CARTESIAN_POINT('Ctrl Pts',(373.741044569875,-14.7429923716155,2.64942046393343));
#43347=CARTESIAN_POINT('Ctrl Pts',(373.660101601016,-14.7490638897097,2.73822444703425));
#43348=CARTESIAN_POINT('Ctrl Pts',(373.575020647871,-14.7551354078038,2.8233866481389));
#43349=CARTESIAN_POINT('Ctrl Pts',(373.486170634858,-14.7612069258979,2.90450784549498));
#43350=CARTESIAN_POINT('Ctrl Pts',(373.400513073819,-14.7670602894946,2.98271429339955));
#43351=CARTESIAN_POINT('Ctrl Pts',(373.311352973549,-14.7729136530914,3.05716483048401));
#43352=CARTESIAN_POINT('Ctrl Pts',(373.21905858448,-14.7787670166881,3.12753907164879));
#43353=CARTESIAN_POINT('Ctrl Pts',(373.126778053102,-14.784619501422,3.19790274635807));
#43354=CARTESIAN_POINT('Ctrl Pts',(373.031364497107,-14.7904719861559,3.26419109167765));
#43355=CARTESIAN_POINT('Ctrl Pts',(372.933218361241,-14.7963244708898,3.32612472066898));
#43356=CARTESIAN_POINT('Ctrl Pts',(372.835063226692,-14.802177492218,3.38806402814259));
#43357=CARTESIAN_POINT('Ctrl Pts',(372.734175363635,-14.8080305135462,3.44564760508579));
#43358=CARTESIAN_POINT('Ctrl Pts',(372.630982625259,-14.8138835348744,3.49864040691914));
#43359=CARTESIAN_POINT('Ctrl Pts',(372.527755470112,-14.8197385082982,3.55165088287532));
#43360=CARTESIAN_POINT('Ctrl Pts',(372.422222278399,-14.825593481722,3.60006735054329));
#43361=CARTESIAN_POINT('Ctrl Pts',(372.314833173612,-14.8314484551459,3.64370187942084));
#43362=CARTESIAN_POINT('Ctrl Pts',(372.20732235707,-14.83731006443,3.68738586243212));
#43363=CARTESIAN_POINT('Ctrl Pts',(372.097951812086,-14.8431716737142,3.72627693362258));
#43364=CARTESIAN_POINT('Ctrl Pts',(371.987189296493,-14.8490332829983,3.76023622067742));
#43365=CARTESIAN_POINT('Ctrl Pts',(371.876352092922,-14.8548988448087,3.79421840672896));
#43366=CARTESIAN_POINT('Ctrl Pts',(371.764121448728,-14.860764406619,3.8232620835104));
#43367=CARTESIAN_POINT('Ctrl Pts',(371.650976155193,-14.8666299684294,3.84727932672243));
#43368=CARTESIAN_POINT('Ctrl Pts',(371.537665415487,-14.8725041071297,3.87133168903465));
#43369=CARTESIAN_POINT('Ctrl Pts',(371.423437763215,-14.87837824583,3.89034288170026));
#43370=CARTESIAN_POINT('Ctrl Pts',(371.308778030582,-14.8842523845304,3.90427669871148));
#43371=CARTESIAN_POINT('Ctrl Pts',(371.279782456033,-14.8857378583117,3.90780033356239));
#43372=CARTESIAN_POINT('Ctrl Pts',(371.25075925197,-14.887223332093,3.91099952969364));
#43373=CARTESIAN_POINT('Ctrl Pts',(371.221716250132,-14.8887088058742,3.9138742292099));
#43374=CARTESIAN_POINT('Ctrl Pts',(371.106877756236,-14.8945824952648,3.9252410350481));
#43375=CARTESIAN_POINT('Ctrl Pts',(370.991347298652,-14.9004561846554,3.93156820814741));
#43376=CARTESIAN_POINT('Ctrl Pts',(370.875604715191,-14.906329874046,3.93278328859206));
#43377=CARTESIAN_POINT('Ctrl Pts',(370.760011566279,-14.9121959799517,3.9339968002537));
#43378=CARTESIAN_POINT('Ctrl Pts',(370.644207245485,-14.9180620858574,3.93011134058085));
#43379=CARTESIAN_POINT('Ctrl Pts',(370.528677603588,-14.9239281917632,3.92110609876889));
#43380=CARTESIAN_POINT('Ctrl Pts',(370.413266262572,-14.9297882908512,3.91211007820978));
#43381=CARTESIAN_POINT('Ctrl Pts',(370.298129450435,-14.9356483899393,3.89800473537626));
#43382=CARTESIAN_POINT('Ctrl Pts',(370.183753245832,-14.9415084890274,3.87882130184023));
#43383=CARTESIAN_POINT('Ctrl Pts',(370.065250608702,-14.9475800071215,3.85894577378668));
#43384=CARTESIAN_POINT('Ctrl Pts',(369.947564948923,-14.9536515252156,3.83361882040805));
#43385=CARTESIAN_POINT('Ctrl Pts',(369.831231733103,-14.9597230433097,3.80293402988006));
#43386=CARTESIAN_POINT('Ctrl Pts',(369.719078462698,-14.9655764069064,3.77335176839843));
#43387=CARTESIAN_POINT('Ctrl Pts',(369.608182553798,-14.9714297705032,3.73879018073696));
#43388=CARTESIAN_POINT('Ctrl Pts',(369.499012860579,-14.9772831340999,3.69938502681424));
#43389=CARTESIAN_POINT('Ctrl Pts',(369.389859558822,-14.9831356188338,3.65998578944272));
#43390=CARTESIAN_POINT('Ctrl Pts',(369.282432345887,-14.9889881035677,3.61574457207696));
#43391=CARTESIAN_POINT('Ctrl Pts',(369.177183077718,-14.9948405883016,3.56684641326339));
#43392=CARTESIAN_POINT('Ctrl Pts',(369.071924159605,-15.0006936096298,3.51794377114532));
#43393=CARTESIAN_POINT('Ctrl Pts',(368.968843957921,-15.006546630958,3.46438351286968));
#43394=CARTESIAN_POINT('Ctrl Pts',(368.868371925755,-15.0123996522861,3.40639774692673));
#43395=CARTESIAN_POINT('Ctrl Pts',(368.767866384225,-15.0182546257099,3.34839264161094));
#43396=CARTESIAN_POINT('Ctrl Pts',(368.669971099555,-15.0241095991338,3.28595930008585));
#43397=CARTESIAN_POINT('Ctrl Pts',(368.575088007447,-15.0299645725576,3.21937408574269));
#43398=CARTESIAN_POINT('Ctrl Pts',(368.480097377542,-15.0358261818417,3.15271340561161));
#43399=CARTESIAN_POINT('Ctrl Pts',(368.388126092574,-15.0416877911259,3.08189169799442));
#43400=CARTESIAN_POINT('Ctrl Pts',(368.29954442401,-15.04754940041,3.00722673946475));
#43401=CARTESIAN_POINT('Ctrl Pts',(368.210903024176,-15.0534149622204,2.93251143380498));
#43402=CARTESIAN_POINT('Ctrl Pts',(368.125656095021,-15.0592805240307,2.85394799620949));
#43403=CARTESIAN_POINT('Ctrl Pts',(368.04413707733,-15.0651460858411,2.77189109415042));
#43404=CARTESIAN_POINT('Ctrl Pts',(367.962498858841,-15.0710202245414,2.68971420477493));
#43405=CARTESIAN_POINT('Ctrl Pts',(367.884599707743,-15.0768943632418,2.60403396056261));
#43406=CARTESIAN_POINT('Ctrl Pts',(367.810732880377,-15.0827685019421,2.51523814219873));
#43407=CARTESIAN_POINT('Ctrl Pts',(367.792053165621,-15.0842539757234,2.49278312933733));
#43408=CARTESIAN_POINT('Ctrl Pts',(367.773631101045,-15.0857394495046,2.47012901786266));
#43409=CARTESIAN_POINT('Ctrl Pts',(367.755470980959,-15.0872249232859,2.44728235746135));
#43410=CARTESIAN_POINT('Ctrl Pts',(367.683793739455,-15.093088026749,2.35710753552393));
#43411=CARTESIAN_POINT('Ctrl Pts',(367.615956575156,-15.098951130212,2.26362391034172));
#43412=CARTESIAN_POINT('Ctrl Pts',(367.552281197227,-15.1048142336751,2.1671927437798));
#43413=CARTESIAN_POINT('Ctrl Pts',(367.488685545306,-15.1106699961243,2.070882315755));
#43414=CARTESIAN_POINT('Ctrl Pts',(367.429241547768,-15.1165257585734,1.97163202414228));
#43415=CARTESIAN_POINT('Ctrl Pts',(367.374231072832,-15.1223815210226,1.86983648273214));
#43416=CARTESIAN_POINT('Ctrl Pts',(367.319276074643,-15.1282313780755,1.76814359968881));
#43417=CARTESIAN_POINT('Ctrl Pts',(367.26874590511,-15.1340812351284,1.66391093220002));
#43418=CARTESIAN_POINT('Ctrl Pts',(367.222879046891,-15.1399310921813,1.55756179592009));
#43419=CARTESIAN_POINT('Ctrl Pts',(367.177047273904,-15.1457764744652,1.45129400997268));
#43420=CARTESIAN_POINT('Ctrl Pts',(367.135871881179,-15.1516218567491,1.34291335396061));
#43421=CARTESIAN_POINT('Ctrl Pts',(367.099544979911,-15.157467239033,1.23286681550194));
#43422=CARTESIAN_POINT('Ctrl Pts',(367.063234004256,-15.1633100587175,1.122868521141));
#43423=CARTESIAN_POINT('Ctrl Pts',(367.031767424684,-15.169152878402,1.0112061886496));
#43424=CARTESIAN_POINT('Ctrl Pts',(367.005288628067,-15.1749956980865,0.898345252612361));
#43425=CARTESIAN_POINT('Ctrl Pts',(366.978816924361,-15.1808369526468,0.785514548789961));
#43426=CARTESIAN_POINT('Ctrl Pts',(366.957330437256,-15.1866782072072,0.671486283929554));
#43427=CARTESIAN_POINT('Ctrl Pts',(366.940922026421,-15.1925194617675,0.556738660264014));
#43428=CARTESIAN_POINT('Ctrl Pts',(366.92450971715,-15.1983621041381,0.441963773973242));
#43429=CARTESIAN_POINT('Ctrl Pts',(366.913177954739,-15.2042047465087,0.326469597483944));
#43430=CARTESIAN_POINT('Ctrl Pts',(366.906967993488,-15.2100473888794,0.210741735856712));
#43431=CARTESIAN_POINT('Ctrl Pts',(366.903145532068,-15.2136437519079,0.139506945751349));
#43432=CARTESIAN_POINT('Ctrl Pts',(366.901262628572,-15.2172401149365,0.0681837294482758));
#43433=CARTESIAN_POINT('Ctrl Pts',(366.901319086285,-15.2208364779651,-0.00311436263953608));
#43434=CARTESIAN_POINT('',(366.901317920817,-16.47083647792,-0.000729168186946121));
#43435=CARTESIAN_POINT('Ctrl Pts',(366.901319086285,-15.2208364780051,-0.00311436343211994));
#43436=CARTESIAN_POINT('Ctrl Pts',(366.901426740083,-15.2276940359743,-0.139065822086587));
#43437=CARTESIAN_POINT('Ctrl Pts',(366.908587402639,-15.2345515939436,-0.274721646700906));
#43438=CARTESIAN_POINT('Ctrl Pts',(366.92268598836,-15.2414091519128,-0.409420509722039));
#43439=CARTESIAN_POINT('Ctrl Pts',(366.936878419049,-15.2483123561134,-0.545015974052312));
#43440=CARTESIAN_POINT('Ctrl Pts',(366.958101331657,-15.2552155603139,-0.679641608731294));
#43441=CARTESIAN_POINT('Ctrl Pts',(366.98618838034,-15.2621187645144,-0.812642947378062));
#43442=CARTESIAN_POINT('Ctrl Pts',(367.014475827037,-15.2690712223202,-0.946593235997586));
#43443=CARTESIAN_POINT('Ctrl Pts',(367.04972563269,-15.2760236801261,-1.07889588617637));
#43444=CARTESIAN_POINT('Ctrl Pts',(367.091719796211,-15.2829761379319,-1.20890395964389));
#43445=CARTESIAN_POINT('Ctrl Pts',(367.097286641879,-15.2838977721871,-1.22613813744253));
#43446=CARTESIAN_POINT('Ctrl Pts',(367.102971936878,-15.2848194064424,-1.24333202509166));
#43447=CARTESIAN_POINT('Ctrl Pts',(367.108775111529,-15.2857410406976,-1.26048414500428));
#43448=CARTESIAN_POINT('Ctrl Pts',(367.145759463176,-15.2916147300882,-1.36979673205895));
#43449=CARTESIAN_POINT('Ctrl Pts',(367.187620563434,-15.2974884194787,-1.4776622410702));
#43450=CARTESIAN_POINT('Ctrl Pts',(367.234226623194,-15.3033621088693,-1.58361363200196));
#43451=CARTESIAN_POINT('Ctrl Pts',(367.280772510153,-15.3092282147751,-1.68942822973434));
#43452=CARTESIAN_POINT('Ctrl Pts',(367.332051008801,-15.3150943206809,-1.79333324928479));
#43453=CARTESIAN_POINT('Ctrl Pts',(367.387880794919,-15.3209604265866,-1.89487746388623));
#43454=CARTESIAN_POINT('Ctrl Pts',(367.443653412048,-15.3268205256747,-1.99631769850556));
#43455=CARTESIAN_POINT('Ctrl Pts',(367.50396784874,-15.3326806247627,-2.09540157677105));
#43456=CARTESIAN_POINT('Ctrl Pts',(367.568595272185,-15.3385407238508,-2.19169911796628));
#43457=CARTESIAN_POINT('Ctrl Pts',(367.63555430563,-15.3446122419449,-2.29147085475769));
#43458=CARTESIAN_POINT('Ctrl Pts',(367.70714322511,-15.350683760039,-2.38825099576136));
#43459=CARTESIAN_POINT('Ctrl Pts',(367.783056026683,-15.3567552781331,-2.48159026954379));
#43460=CARTESIAN_POINT('Ctrl Pts',(367.856241220628,-15.3626086417299,-2.57157578862457));
#43461=CARTESIAN_POINT('Ctrl Pts',(367.933444640014,-15.3684620053266,-2.65836310329369));
#43462=CARTESIAN_POINT('Ctrl Pts',(368.014349319108,-15.3743153689234,-2.74158101587276));
#43463=CARTESIAN_POINT('Ctrl Pts',(368.095241850636,-15.3801678536573,-2.82478643356228));
#43464=CARTESIAN_POINT('Ctrl Pts',(368.179834248955,-15.3860203383912,-2.9044232186531));
#43465=CARTESIAN_POINT('Ctrl Pts',(368.267771658926,-15.3918728231251,-2.98015597453164));
#43466=CARTESIAN_POINT('Ctrl Pts',(368.355717131578,-15.3977258444533,-3.05589567408727));
#43467=CARTESIAN_POINT('Ctrl Pts',(368.447007912489,-15.4035788657815,-3.12773036324572));
#43468=CARTESIAN_POINT('Ctrl Pts',(368.541255497375,-15.4094318871097,-3.19536445999363));
#43469=CARTESIAN_POINT('Ctrl Pts',(368.635534515651,-15.4152868605335,-3.26302111401864));
#43470=CARTESIAN_POINT('Ctrl Pts',(368.732771963341,-15.4211418339573,-3.32647414910308));
#43471=CARTESIAN_POINT('Ctrl Pts',(368.832550360121,-15.4269968073811,-3.38547129711021));
#43472=CARTESIAN_POINT('Ctrl Pts',(368.932441842899,-15.4328584166653,-3.44453531080686));
#43473=CARTESIAN_POINT('Ctrl Pts',(369.034879666925,-15.4387200259495,-3.49913314718487));
#43474=CARTESIAN_POINT('Ctrl Pts',(369.139421674341,-15.4445816352336,-3.54905845863487));
#43475=CARTESIAN_POINT('Ctrl Pts',(369.2440341752,-15.450447197044,-3.59901743508896));
#43476=CARTESIAN_POINT('Ctrl Pts',(369.35075330534,-15.4563127588543,-3.64429745186666));
#43477=CARTESIAN_POINT('Ctrl Pts',(369.459118479303,-15.4621783206647,-3.68474092467395));
#43478=CARTESIAN_POINT('Ctrl Pts',(369.567642109729,-15.468052459365,-3.72524353575792));
#43479=CARTESIAN_POINT('Ctrl Pts',(369.677816196019,-15.4739265980653,-3.76089536180227));
#43480=CARTESIAN_POINT('Ctrl Pts',(369.78916654942,-15.4798007367657,-3.7915890800767));
#43481=CARTESIAN_POINT('Ctrl Pts',(369.817325235985,-15.4812862105468,-3.79935102034902));
#43482=CARTESIAN_POINT('Ctrl Pts',(369.84555910456,-15.482771684328,-3.8067961459464));
#43483=CARTESIAN_POINT('Ctrl Pts',(369.873860417607,-15.4842571581092,-3.81392324442529));
#43484=CARTESIAN_POINT('Ctrl Pts',(369.985766211092,-15.4901308474997,-3.84210439662835));
#43485=CARTESIAN_POINT('Ctrl Pts',(370.099099745348,-15.4960045368903,-3.86540310393339));
#43486=CARTESIAN_POINT('Ctrl Pts',(370.213397118836,-15.5018782262808,-3.88367692291822));
#43487=CARTESIAN_POINT('Ctrl Pts',(370.327546923678,-15.5077443321866,-3.90192714868599));
#43488=CARTESIAN_POINT('Ctrl Pts',(370.442657688797,-15.5136104380923,-3.91516532321915));
#43489=CARTESIAN_POINT('Ctrl Pts',(370.558251947216,-15.519476543998,-3.92329920035934));
#43490=CARTESIAN_POINT('Ctrl Pts',(370.673727838588,-15.5253366430861,-3.93142474851296));
#43491=CARTESIAN_POINT('Ctrl Pts',(370.789685828807,-15.5311967421741,-3.93445636685652));
#43492=CARTESIAN_POINT('Ctrl Pts',(370.905640549261,-15.5370568412621,-3.93235324875957));
#43493=CARTESIAN_POINT('Ctrl Pts',(371.025778651495,-15.5431283593562,-3.93017425495966));
#43494=CARTESIAN_POINT('Ctrl Pts',(371.145912797567,-15.5491998774503,-3.9224829590621));
#43495=CARTESIAN_POINT('Ctrl Pts',(371.265499573519,-15.5552713955444,-3.90929294426539));
#43496=CARTESIAN_POINT('Ctrl Pts',(371.380789501039,-15.5611247591412,-3.89657685724157));
#43497=CARTESIAN_POINT('Ctrl Pts',(371.495570270525,-15.5669781227379,-3.87875044681748));
#43498=CARTESIAN_POINT('Ctrl Pts',(371.609358131515,-15.5728314863346,-3.85587883199502));
#43499=CARTESIAN_POINT('Ctrl Pts',(371.72312890764,-15.5786839710685,-3.83301065126854));
#43500=CARTESIAN_POINT('Ctrl Pts',(371.835906666765,-15.5845364558024,-3.80509885377174));
#43501=CARTESIAN_POINT('Ctrl Pts',(371.947217202139,-15.5903889405363,-3.77225980536663));
#43502=CARTESIAN_POINT('Ctrl Pts',(372.058537943194,-15.5962419618645,-3.73941774606172));
#43503=CARTESIAN_POINT('Ctrl Pts',(372.168390796794,-15.6020949831926,-3.7016476546982));
#43504=CARTESIAN_POINT('Ctrl Pts',(372.276316771186,-15.6079480045208,-3.65911575665432));
#43505=CARTESIAN_POINT('Ctrl Pts',(372.384278740974,-15.6138029779446,-3.61656967340109));
#43506=CARTESIAN_POINT('Ctrl Pts',(372.490312169504,-15.6196579513684,-3.56925877688727));
#43507=CARTESIAN_POINT('Ctrl Pts',(372.593978753825,-15.6255129247922,-3.51739712214837));
#43508=CARTESIAN_POINT('Ctrl Pts',(372.697762830903,-15.6313745340763,-3.46547668888518));
#43509=CARTESIAN_POINT('Ctrl Pts',(372.799174339944,-15.6372361433605,-3.40899538788675));
#43510=CARTESIAN_POINT('Ctrl Pts',(372.897800187449,-15.6430977526446,-3.34821290487047));
#43511=CARTESIAN_POINT('Ctrl Pts',(372.996492539088,-15.6489633144549,-3.28738943577955));
#43512=CARTESIAN_POINT('Ctrl Pts',(373.092395147963,-15.6548288762653,-3.22225924103046));
#43513=CARTESIAN_POINT('Ctrl Pts',(373.185125906998,-15.6606944380756,-3.15312392625312));
#43514=CARTESIAN_POINT('Ctrl Pts',(373.277992261147,-15.6665685767759,-3.08388751868903));
#43515=CARTESIAN_POINT('Ctrl Pts',(373.367677190384,-15.6724427154762,-3.01063456340494));
#43516=CARTESIAN_POINT('Ctrl Pts',(373.453833448343,-15.6783168541765,-2.93370534425832));
#43517=CARTESIAN_POINT('Ctrl Pts',(373.475620959471,-15.679802327958,-2.91425120061299));
#43518=CARTESIAN_POINT('Ctrl Pts',(373.497183005625,-15.6812878017394,-2.89456213268642));
#43519=CARTESIAN_POINT('Ctrl Pts',(373.518514373385,-15.6827732755208,-2.87464398511441));
#43520=CARTESIAN_POINT('Ctrl Pts',(373.602860411711,-15.6886469649114,-2.79588593934087));
#43521=CARTESIAN_POINT('Ctrl Pts',(373.683877685125,-15.694520654302,-2.71328133197832));
#43522=CARTESIAN_POINT('Ctrl Pts',(373.761195011868,-15.7003943436926,-2.62714276319492));
#43523=CARTESIAN_POINT('Ctrl Pts',(373.838412514679,-15.7062604495983,-2.5411154073962));
#43524=CARTESIAN_POINT('Ctrl Pts',(373.911939297212,-15.7121265555041,-2.45156346849149));
#43525=CARTESIAN_POINT('Ctrl Pts',(373.981439004909,-15.7179926614098,-2.35883815820824));
#43526=CARTESIAN_POINT('Ctrl Pts',(374.05086754579,-15.7238527604979,-2.26620779746146));
#43527=CARTESIAN_POINT('Ctrl Pts',(374.116276967849,-15.7297128595859,-2.1704108574716));
#43528=CARTESIAN_POINT('Ctrl Pts',(374.177369858013,-15.735572958674,-2.0718330756301));
#43529=CARTESIAN_POINT('Ctrl Pts',(374.240666840279,-15.7416444767681,-1.96969883231179));
#43530=CARTESIAN_POINT('Ctrl Pts',(374.299329647164,-15.7477159948622,-1.86457964199185));
#43531=CARTESIAN_POINT('Ctrl Pts',(374.35307510286,-15.7537875129563,-1.75693950326599));
#43532=CARTESIAN_POINT('Ctrl Pts',(374.40488944138,-15.759640876553,-1.65316696074828));
#43533=CARTESIAN_POINT('Ctrl Pts',(374.452133515632,-15.7654942401498,-1.54705191280296));
#43534=CARTESIAN_POINT('Ctrl Pts',(374.494599799898,-15.7713476037466,-1.43903616036896));
#43535=CARTESIAN_POINT('Ctrl Pts',(374.537059707995,-15.7772000884805,-1.3310366261367));
#43536=CARTESIAN_POINT('Ctrl Pts',(374.574743101381,-15.7830525732144,-1.22113733926093));
#43537=CARTESIAN_POINT('Ctrl Pts',(374.607490691213,-15.7889050579483,-1.10979986243639));
#43538=CARTESIAN_POINT('Ctrl Pts',(374.640241283559,-15.7947580792765,-0.998452177460075));
#43539=CARTESIAN_POINT('Ctrl Pts',(374.668055056145,-15.8006111006046,-0.88566643678181));
#43540=CARTESIAN_POINT('Ctrl Pts',(374.690822865664,-15.8064641219328,-0.77191844713202));
#43541=CARTESIAN_POINT('Ctrl Pts',(374.713598268688,-15.8123190953567,-0.658132520330992));
#43542=CARTESIAN_POINT('Ctrl Pts',(374.73132428118,-15.8181740687805,-0.543384111297028));
#43543=CARTESIAN_POINT('Ctrl Pts',(374.743943167067,-15.8240290422043,-0.428157570708126));
#43544=CARTESIAN_POINT('Ctrl Pts',(374.756576354842,-15.8298906514885,-0.312800435635769));
#43545=CARTESIAN_POINT('Ctrl Pts',(374.764090817968,-15.8357522607726,-0.196964498326556));
#43546=CARTESIAN_POINT('Ctrl Pts',(374.766480830481,-15.8416138700568,-0.0811376625844174));
#43547=CARTESIAN_POINT('Ctrl Pts',(374.768872454596,-15.8474794318671,0.0347672760436905));
#43548=CARTESIAN_POINT('Ctrl Pts',(374.76613275726,-15.8533449936775,0.150662688876631));
#43549=CARTESIAN_POINT('Ctrl Pts',(374.75830803617,-15.8592105554878,0.266063985059273));
#43550=CARTESIAN_POINT('Ctrl Pts',(374.750471873418,-15.8650846941882,0.381634026240967));
#43551=CARTESIAN_POINT('Ctrl Pts',(374.737535893395,-15.8709588328885,0.496708099823931));
#43552=CARTESIAN_POINT('Ctrl Pts',(374.719597793738,-15.8768329715888,0.610809940846733));
#43553=CARTESIAN_POINT('Ctrl Pts',(374.715061541177,-15.8783184453701,0.639664433713723));
#43554=CARTESIAN_POINT('Ctrl Pts',(374.710205653192,-15.8798039191513,0.668456821280135));
#43555=CARTESIAN_POINT('Ctrl Pts',(374.705032214831,-15.8812893929325,0.697179554237102));
#43556=CARTESIAN_POINT('Ctrl Pts',(374.684576000529,-15.8871630823231,0.810751677804809));
#43557=CARTESIAN_POINT('Ctrl Pts',(374.659082935221,-15.8930367717137,0.923611871718623));
#43558=CARTESIAN_POINT('Ctrl Pts',(374.628614478119,-15.8989104611042,1.03527876550775));
#43559=CARTESIAN_POINT('Ctrl Pts',(374.598185358657,-15.90477656701,1.14680148684628));
#43560=CARTESIAN_POINT('Ctrl Pts',(374.562793729788,-15.9106426729157,1.25713357699837));
#43561=CARTESIAN_POINT('Ctrl Pts',(374.522552376477,-15.9165087788215,1.36580199936999));
#43562=CARTESIAN_POINT('Ctrl Pts',(374.4823522298,-15.9223688779095,1.4743591466615));
#43563=CARTESIAN_POINT('Ctrl Pts',(374.437312379196,-15.9282289769976,1.58125562959299));
#43564=CARTESIAN_POINT('Ctrl Pts',(374.387595732367,-15.9340890760856,1.68603241771671));
#43565=CARTESIAN_POINT('Ctrl Pts',(374.336085422343,-15.9401605941797,1.79458931332171));
#43566=CARTESIAN_POINT('Ctrl Pts',(374.27955460738,-15.9462321122738,1.90087024314795));
#43567=CARTESIAN_POINT('Ctrl Pts',(374.218239676841,-15.9523036303679,2.00438571429028));
#43568=CARTESIAN_POINT('Ctrl Pts',(374.159127840757,-15.9581569939647,2.10418179182708));
#43569=CARTESIAN_POINT('Ctrl Pts',(374.095569995253,-15.9640103575614,2.20140733490737));
#43570=CARTESIAN_POINT('Ctrl Pts',(374.027824887459,-15.9698637211582,2.29564845355112));
#43571=CARTESIAN_POINT('Ctrl Pts',(373.960089951365,-15.9757162058921,2.38987542220805));
#43572=CARTESIAN_POINT('Ctrl Pts',(373.888169244162,-15.981568690626,2.48111852204783));
#43573=CARTESIAN_POINT('Ctrl Pts',(373.812364268609,-15.9874211753599,2.56899368387903));
#43574=CARTESIAN_POINT('Ctrl Pts',(373.736552342758,-15.9932741966881,2.65687690268273));
#43575=CARTESIAN_POINT('Ctrl Pts',(373.656855710469,-15.9991272180163,2.74139125677456));
#43576=CARTESIAN_POINT('Ctrl Pts',(373.573615028248,-16.0049802393445,2.82218709282486));
#43577=CARTESIAN_POINT('Ctrl Pts',(373.490346583652,-16.0108352127683,2.90300987584687));
#43578=CARTESIAN_POINT('Ctrl Pts',(373.40353203505,-16.0166901861921,2.98011138715356));
#43579=CARTESIAN_POINT('Ctrl Pts',(373.313547086845,-16.0225451596159,3.05318053956203));
#43580=CARTESIAN_POINT('Ctrl Pts',(373.223460152259,-16.0284067689001,3.12633250646928));
#43581=CARTESIAN_POINT('Ctrl Pts',(373.130195967081,-16.0342683781843,3.19544273213424));
#43582=CARTESIAN_POINT('Ctrl Pts',(373.034161416605,-16.0401299874684,3.2602419076892));
#43583=CARTESIAN_POINT('Ctrl Pts',(372.938062109325,-16.0459955492788,3.32508477780416));
#43584=CARTESIAN_POINT('Ctrl Pts',(372.839189068483,-16.0518611110891,3.3856105942126));
#43585=CARTESIAN_POINT('Ctrl Pts',(372.737974597999,-16.0577266728995,3.44159555992142));
#43586=CARTESIAN_POINT('Ctrl Pts',(372.636612127135,-16.0636008115998,3.49766238938128));
#43587=CARTESIAN_POINT('Ctrl Pts',(372.532901762289,-16.0694749503001,3.54917493361627));
#43588=CARTESIAN_POINT('Ctrl Pts',(372.427296675464,-16.0753490890005,3.59595710095316));
#43589=CARTESIAN_POINT('Ctrl Pts',(372.400590873023,-16.0768345627817,3.60778754734757));
#43590=CARTESIAN_POINT('Ctrl Pts',(372.37376398075,-16.0783200365629,3.61931573371256));
#43591=CARTESIAN_POINT('Ctrl Pts',(372.346823472713,-16.0798055103441,3.63053931957964));
#43592=CARTESIAN_POINT('Ctrl Pts',(372.240298417723,-16.0856791997347,3.67491833054902));
#43593=CARTESIAN_POINT('Ctrl Pts',(372.131641077973,-16.0915528891252,3.71467889225633));
#43594=CARTESIAN_POINT('Ctrl Pts',(372.021289270468,-16.0974265785158,3.74961169384864));
#43595=CARTESIAN_POINT('Ctrl Pts',(371.911079937514,-16.1032926844216,3.78449939391228));
#43596=CARTESIAN_POINT('Ctrl Pts',(371.799180877741,-16.1091587903273,3.8145716058894));
#43597=CARTESIAN_POINT('Ctrl Pts',(371.686050729313,-16.1150248962331,3.83966666623411));
#43598=CARTESIAN_POINT('Ctrl Pts',(371.573036424716,-16.1208849953211,3.86473602955671));
#43599=CARTESIAN_POINT('Ctrl Pts',(371.458793939884,-16.1267450944091,3.88483828974794));
#43600=CARTESIAN_POINT('Ctrl Pts',(371.343797315517,-16.1326051934971,3.8998614946561));
#43601=CARTESIAN_POINT('Ctrl Pts',(371.224651875293,-16.1386767115913,3.91542670252396));
#43602=CARTESIAN_POINT('Ctrl Pts',(371.104697283495,-16.1447482296854,3.92553931799939));
#43603=CARTESIAN_POINT('Ctrl Pts',(370.984473013775,-16.1508197477795,3.9301326221592));
#43604=CARTESIAN_POINT('Ctrl Pts',(370.868568498146,-16.1566731113762,3.93456088522967));
#43605=CARTESIAN_POINT('Ctrl Pts',(370.752413798801,-16.162526474973,3.93385962051803));
#43606=CARTESIAN_POINT('Ctrl Pts',(370.636496980016,-16.1683798385697,3.92802188157386));
#43607=CARTESIAN_POINT('Ctrl Pts',(370.520597565751,-16.1742323233036,3.92218501914655));
#43608=CARTESIAN_POINT('Ctrl Pts',(370.404936373539,-16.1800848080375,3.911213236745));
#43609=CARTESIAN_POINT('Ctrl Pts',(370.289999587249,-16.1859372927714,3.89515168194081));
#43610=CARTESIAN_POINT('Ctrl Pts',(370.175052262799,-16.1917903140996,3.8790886545077));
#43611=CARTESIAN_POINT('Ctrl Pts',(370.060829885495,-16.1976433354278,3.85793498416944));
#43612=CARTESIAN_POINT('Ctrl Pts',(369.947810944906,-16.2034963567559,3.83178737686533));
#43613=CARTESIAN_POINT('Ctrl Pts',(369.834754310318,-16.2093513301797,3.80563104882924));
#43614=CARTESIAN_POINT('Ctrl Pts',(369.722902312845,-16.2152063036035,3.77447756498039));
#43615=CARTESIAN_POINT('Ctrl Pts',(369.612720034418,-16.2210612770274,3.73847398935558));
#43616=CARTESIAN_POINT('Ctrl Pts',(369.502412878531,-16.2269228863115,3.70242960830225));
#43617=CARTESIAN_POINT('Ctrl Pts',(369.393779611761,-16.2327844955957,3.66152429227512));
#43618=CARTESIAN_POINT('Ctrl Pts',(369.287267112851,-16.2386461048798,3.61595395528093));
#43619=CARTESIAN_POINT('Ctrl Pts',(369.180682791781,-16.2445116666902,3.57035288987379));
#43620=CARTESIAN_POINT('Ctrl Pts',(369.076222457472,-16.2503772285005,3.52008071851414));
#43621=CARTESIAN_POINT('Ctrl Pts',(368.97430852436,-16.2562427903108,3.46537938710012));
#43622=CARTESIAN_POINT('Ctrl Pts',(368.872245568082,-16.2621169290112,3.4105980689233));
#43623=CARTESIAN_POINT('Ctrl Pts',(368.772736797759,-16.2679910677115,3.35137487567273));
#43624=CARTESIAN_POINT('Ctrl Pts',(368.676175853458,-16.2738652064118,3.28799515036809));
#43625=CARTESIAN_POINT('Ctrl Pts',(368.651757167012,-16.2753506801931,3.27196745251969));
#43626=CARTESIAN_POINT('Ctrl Pts',(368.627526828092,-16.2768361539745,3.25567414389832));
#43627=CARTESIAN_POINT('Ctrl Pts',(368.603490855174,-16.2783216277558,3.23912023623242));
#43628=CARTESIAN_POINT('Ctrl Pts',(368.508920869072,-16.2841662522001,3.17398857614697));
#43629=CARTESIAN_POINT('Ctrl Pts',(368.417040452205,-16.2900108766443,3.10459792704851));
#43630=CARTESIAN_POINT('Ctrl Pts',(368.328260515829,-16.2958555010885,3.03119871036011));
#43631=CARTESIAN_POINT('Ctrl Pts',(368.239595465043,-16.3016925623022,2.95789447585637));
#43632=CARTESIAN_POINT('Ctrl Pts',(368.154023236462,-16.3075296235159,2.88059225098274));
#43633=CARTESIAN_POINT('Ctrl Pts',(368.071926197233,-16.3133666847296,2.7995859227593));
#43634=CARTESIAN_POINT('Ctrl Pts',(367.989912890329,-16.319197792614,2.71866221442457));
#43635=CARTESIAN_POINT('Ctrl Pts',(367.911368019625,-16.3250289004984,2.63404220735748));
#43636=CARTESIAN_POINT('Ctrl Pts',(367.836640672554,-16.3308600083827,2.54605980300708));
#43637=CARTESIAN_POINT('Ctrl Pts',(367.761897370278,-16.3366923612801,2.458058613335));
#43638=CARTESIAN_POINT('Ctrl Pts',(367.690973526947,-16.3425247141775,2.36669387758273));
#43639=CARTESIAN_POINT('Ctrl Pts',(367.624181520526,-16.3483570670749,2.27233662239791));
#43640=CARTESIAN_POINT('Ctrl Pts',(367.557477847291,-16.3541817066194,2.17810415575409));
#43641=CARTESIAN_POINT('Ctrl Pts',(367.494895343439,-16.3600063461638,2.08088741183962));
#43642=CARTESIAN_POINT('Ctrl Pts',(367.436704138707,-16.3658309857083,1.98108809670978));
#43643=CARTESIAN_POINT('Ctrl Pts',(367.378520858579,-16.3716548320407,1.88130237246761));
#43644=CARTESIAN_POINT('Ctrl Pts',(367.324727898941,-16.3774786783731,1.77893513706548));
#43645=CARTESIAN_POINT('Ctrl Pts',(367.275550703742,-16.3833025247055,1.67441493536281));
#43646=CARTESIAN_POINT('Ctrl Pts',(367.226368005011,-16.3891270227978,1.56988303656711));
#43647=CARTESIAN_POINT('Ctrl Pts',(367.181802274987,-16.3949515208901,1.46319807070222));
#43648=CARTESIAN_POINT('Ctrl Pts',(367.142031525462,-16.4007760189823,1.35481019845036));
#43649=CARTESIAN_POINT('Ctrl Pts',(367.102166045212,-16.4066143905605,1.24616415500668));
#43650=CARTESIAN_POINT('Ctrl Pts',(367.06711855498,-16.4124527621386,1.13580748026041));
#43651=CARTESIAN_POINT('Ctrl Pts',(367.037018242879,-16.4182911337167,1.02420928978219));
#43652=CARTESIAN_POINT('Ctrl Pts',(367.006944774031,-16.4241242986751,0.912710621805926));
#43653=CARTESIAN_POINT('Ctrl Pts',(366.981809722171,-16.4299574636334,0.799973067514173));
#43654=CARTESIAN_POINT('Ctrl Pts',(366.961690530963,-16.4357906285918,0.686474051132961));
#43655=CARTESIAN_POINT('Ctrl Pts',(366.941537999637,-16.4416334598636,0.572786952110634));
#43656=CARTESIAN_POINT('Ctrl Pts',(366.926417992745,-16.4474762911354,0.458336284254925));
#43657=CARTESIAN_POINT('Ctrl Pts',(366.916356076746,-16.4533191224073,0.3436051775739));
#43658=CARTESIAN_POINT('Ctrl Pts',(366.906300554488,-16.4591582409115,0.228946975605304));
#43659=CARTESIAN_POINT('Ctrl Pts',(366.901296648633,-16.4649973594158,0.114009106601531));
#43660=CARTESIAN_POINT('Ctrl Pts',(366.901317920817,-16.47083647792,-0.0007291681869142));
#43661=CARTESIAN_POINT('',(366.901319463554,-17.7208364779321,0.00355905278372125));
#43662=CARTESIAN_POINT('Ctrl Pts',(366.901317920817,-16.4708364779651,-0.000729169072720509));
#43663=CARTESIAN_POINT('Ctrl Pts',(366.901325208459,-16.4728369003659,-0.0400373309035736));
#43664=CARTESIAN_POINT('Ctrl Pts',(366.901921774908,-16.4748373227667,-0.0793393664645878));
#43665=CARTESIAN_POINT('Ctrl Pts',(366.90310716762,-16.4768377451675,-0.118623544857057));
#43666=CARTESIAN_POINT('Ctrl Pts',(366.90658774682,-16.4827114345581,-0.233970714409067));
#43667=CARTESIAN_POINT('Ctrl Pts',(366.915155093854,-16.4885851239486,-0.34935667678678));
#43668=CARTESIAN_POINT('Ctrl Pts',(366.928819423885,-16.4944588133392,-0.464296261488943));
#43669=CARTESIAN_POINT('Ctrl Pts',(366.942466111982,-16.5003249192449,-0.579087448389017));
#43670=CARTESIAN_POINT('Ctrl Pts',(366.961196647927,-16.5061910251507,-0.693432997207112));
#43671=CARTESIAN_POINT('Ctrl Pts',(366.984969253279,-16.5120571310564,-0.806848409615581));
#43672=CARTESIAN_POINT('Ctrl Pts',(367.008717515785,-16.5179172301445,-0.920147686086775));
#43673=CARTESIAN_POINT('Ctrl Pts',(367.037497493783,-16.5237773292325,-1.03251831869163));
#43674=CARTESIAN_POINT('Ctrl Pts',(367.071215768427,-16.5296374283205,-1.14348226894757));
#43675=CARTESIAN_POINT('Ctrl Pts',(367.106150521497,-16.5357089464146,-1.25844954537938));
#43676=CARTESIAN_POINT('Ctrl Pts',(367.146386570428,-16.5417804645087,-1.37190627480334));
#43677=CARTESIAN_POINT('Ctrl Pts',(367.191762311665,-16.5478519826029,-1.48333345093234));
#43678=CARTESIAN_POINT('Ctrl Pts',(367.235507666256,-16.5537053461996,-1.59075695957264));
#43679=CARTESIAN_POINT('Ctrl Pts',(367.284029553862,-16.5595587097964,-1.69629383642354));
#43680=CARTESIAN_POINT('Ctrl Pts',(367.33713310628,-16.5654120733931,-1.79949655341228));
#43681=CARTESIAN_POINT('Ctrl Pts',(367.390228685378,-16.571264558127,-1.90268377486036));
#43682=CARTESIAN_POINT('Ctrl Pts',(367.447904372462,-16.5771170428609,-2.00353716603906));
#43683=CARTESIAN_POINT('Ctrl Pts',(367.509918612793,-16.5829695275948,-2.10163238703194));
#43684=CARTESIAN_POINT('Ctrl Pts',(367.571938538997,-16.588822548923,-2.19973660203955));
#43685=CARTESIAN_POINT('Ctrl Pts',(367.638297588432,-16.5946755702512,-2.29508179491208));
#43686=CARTESIAN_POINT('Ctrl Pts',(367.708710404532,-16.6005285915793,-2.38727188997903));
#43687=CARTESIAN_POINT('Ctrl Pts',(367.779146704667,-16.6063835650032,-2.47949273222297));
#43688=CARTESIAN_POINT('Ctrl Pts',(367.853639209241,-16.612238538427,-2.56855605608288));
#43689=CARTESIAN_POINT('Ctrl Pts',(367.931862208638,-16.6180935118508,-2.65409876063665));
#43690=CARTESIAN_POINT('Ctrl Pts',(368.010173863758,-16.623955121135,-2.73973841685849));
#43691=CARTESIAN_POINT('Ctrl Pts',(368.092224173651,-16.6298167304191,-2.82184918457442));
#43692=CARTESIAN_POINT('Ctrl Pts',(368.177650426563,-16.6356783397033,-2.90010468502771));
#43693=CARTESIAN_POINT('Ctrl Pts',(368.263134283025,-16.6415439015136,-2.9784129537397));
#43694=CARTESIAN_POINT('Ctrl Pts',(368.351998299459,-16.6474094633239,-3.05286051407843));
#43695=CARTESIAN_POINT('Ctrl Pts',(368.443847910513,-16.6532750251343,-3.12316225210861));
#43696=CARTESIAN_POINT('Ctrl Pts',(368.535831828226,-16.6591491638346,-3.19356678852246));
#43697=CARTESIAN_POINT('Ctrl Pts',(368.630809715783,-16.665023302535,-3.25981316853858));
#43698=CARTESIAN_POINT('Ctrl Pts',(368.72835933147,-16.6708974412353,-3.32166038370168));
#43699=CARTESIAN_POINT('Ctrl Pts',(368.753028036768,-16.6723829150166,-3.33730053475299));
#43700=CARTESIAN_POINT('Ctrl Pts',(368.777861090773,-16.6738683887979,-3.35265959262553));
#43701=CARTESIAN_POINT('Ctrl Pts',(368.802851446387,-16.6753538625791,-3.36773414002573));
#43702=CARTESIAN_POINT('Ctrl Pts',(368.901665433203,-16.6812275519697,-3.42734017969365));
#43703=CARTESIAN_POINT('Ctrl Pts',(369.003269603158,-16.6871012413603,-3.48269279839281));
#43704=CARTESIAN_POINT('Ctrl Pts',(369.107261801409,-16.6929749307509,-3.53352039669936));
#43705=CARTESIAN_POINT('Ctrl Pts',(369.211119735963,-16.6988410366566,-3.58428237180148));
#43706=CARTESIAN_POINT('Ctrl Pts',(369.31735919961,-16.7047071425624,-3.63053076502087));
#43707=CARTESIAN_POINT('Ctrl Pts',(369.425550416114,-16.7105732484682,-3.67203803195696));
#43708=CARTESIAN_POINT('Ctrl Pts',(369.53363084619,-16.7164333475562,-3.7135027959805));
#43709=CARTESIAN_POINT('Ctrl Pts',(369.643658670363,-16.7222934466443,-3.75023594332008));
#43710=CARTESIAN_POINT('Ctrl Pts',(369.7551815459,-16.7281535457323,-3.78205682535497));
#43711=CARTESIAN_POINT('Ctrl Pts',(369.870727912361,-16.7342250638264,-3.81502573221851));
#43712=CARTESIAN_POINT('Ctrl Pts',(369.987878837225,-16.7402965819205,-3.84272103667008));
#43713=CARTESIAN_POINT('Ctrl Pts',(370.106110588611,-16.7463681000146,-3.86499717720014));
#43714=CARTESIAN_POINT('Ctrl Pts',(370.220094178682,-16.7522214636114,-3.88647291819838));
#43715=CARTESIAN_POINT('Ctrl Pts',(370.335081821234,-16.7580748272082,-3.90291213998415));
#43716=CARTESIAN_POINT('Ctrl Pts',(370.450591815006,-16.7639281908049,-3.91423598261445));
#43717=CARTESIAN_POINT('Ctrl Pts',(370.566084465342,-16.7697806755389,-3.92555812500789));
#43718=CARTESIAN_POINT('Ctrl Pts',(370.682098899889,-16.7756331602728,-3.9317663751336));
#43719=CARTESIAN_POINT('Ctrl Pts',(370.798147593364,-16.7814856450067,-3.93283367462974));
#43720=CARTESIAN_POINT('Ctrl Pts',(370.914206926947,-16.7873386663349,-3.93390107198293));
#43721=CARTESIAN_POINT('Ctrl Pts',(371.030300112551,-16.7931916876631,-3.92982657789486));
#43722=CARTESIAN_POINT('Ctrl Pts',(371.145939630176,-16.7990447089913,-3.92063526333801));
#43723=CARTESIAN_POINT('Ctrl Pts',(371.261617715813,-16.8048996824151,-3.91144088330025));
#43724=CARTESIAN_POINT('Ctrl Pts',(371.376841420979,-16.8107546558389,-3.89712632209527));
#43725=CARTESIAN_POINT('Ctrl Pts',(371.49112905884,-16.8166096292628,-3.87776843560543));
#43726=CARTESIAN_POINT('Ctrl Pts',(371.605546227058,-16.822471238547,-3.85838860943768));
#43727=CARTESIAN_POINT('Ctrl Pts',(371.719024802884,-16.8283328478311,-3.8339541183041));
#43728=CARTESIAN_POINT('Ctrl Pts',(371.831093898196,-16.8341944571153,-3.80459281870881));
#43729=CARTESIAN_POINT('Ctrl Pts',(371.943238562521,-16.8400600189256,-3.77521172057359));
#43730=CARTESIAN_POINT('Ctrl Pts',(372.053971460174,-16.845925580736,-3.74089732076055));
#43731=CARTESIAN_POINT('Ctrl Pts',(372.162839110048,-16.8517911425463,-3.70182661265579));
#43732=CARTESIAN_POINT('Ctrl Pts',(372.271865951127,-16.8576652812467,-3.66269877359306));
#43733=CARTESIAN_POINT('Ctrl Pts',(372.379021720284,-16.863539419947,-3.61880090204385));
#43734=CARTESIAN_POINT('Ctrl Pts',(372.483874994972,-16.8694135586474,-3.57035715805946));
#43735=CARTESIAN_POINT('Ctrl Pts',(372.510390676396,-16.8708990324285,-3.55810652605699));
#43736=CARTESIAN_POINT('Ctrl Pts',(372.536759248013,-16.8723845062097,-3.54556540726016));
#43737=CARTESIAN_POINT('Ctrl Pts',(372.562974017947,-16.8738699799908,-3.53273787085405));
#43738=CARTESIAN_POINT('Ctrl Pts',(372.666629442893,-16.8797436693814,-3.48201670333702));
#43739=CARTESIAN_POINT('Ctrl Pts',(372.76822326964,-16.8856173587719,-3.42664510307133));
#43740=CARTESIAN_POINT('Ctrl Pts',(372.867309259094,-16.8914910481625,-3.36681376729656));
#43741=CARTESIAN_POINT('Ctrl Pts',(372.966267319227,-16.8973571540683,-3.30705967939723));
#43742=CARTESIAN_POINT('Ctrl Pts',(373.062723630657,-16.903223259974,-3.24285751824523));
#43743=CARTESIAN_POINT('Ctrl Pts',(373.156254000254,-16.9090893658797,-3.17444507420077));
#43744=CARTESIAN_POINT('Ctrl Pts',(373.249688595943,-16.9149494649678,-3.10610268362744));
#43745=CARTESIAN_POINT('Ctrl Pts',(373.340202877864,-16.9208095640558,-3.03355882810684));
#43746=CARTESIAN_POINT('Ctrl Pts',(373.427399826266,-16.9266696631438,-2.95709568345065));
#43747=CARTESIAN_POINT('Ctrl Pts',(373.517742641639,-16.9327411812379,-2.87787392297556));
#43748=CARTESIAN_POINT('Ctrl Pts',(373.604523853892,-16.9388126993321,-2.79444496945871));
#43749=CARTESIAN_POINT('Ctrl Pts',(373.687337226515,-16.9448842174262,-2.70717000862969));
#43750=CARTESIAN_POINT('Ctrl Pts',(373.767175048477,-16.9507375810229,-2.62303090689171));
#43751=CARTESIAN_POINT('Ctrl Pts',(373.843324950221,-16.9565909446197,-2.53531774700826));
#43752=CARTESIAN_POINT('Ctrl Pts',(373.915459530284,-16.9624443082164,-2.44439255560179));
#43753=CARTESIAN_POINT('Ctrl Pts',(373.987583279583,-16.9682967929503,-2.35348101630686));
#43754=CARTESIAN_POINT('Ctrl Pts',(374.055692649264,-16.9741492776842,-2.25935872800813));
#43755=CARTESIAN_POINT('Ctrl Pts',(374.119500609878,-16.9800017624181,-2.16242069343142));
#43756=CARTESIAN_POINT('Ctrl Pts',(374.183314420827,-16.9858547837463,-2.06547377093849));
#43757=CARTESIAN_POINT('Ctrl Pts',(374.24282581155,-16.9917078050744,-1.96571093407093));
#43758=CARTESIAN_POINT('Ctrl Pts',(374.297791560155,-16.9975608264026,-1.86355544092449));
#43759=CARTESIAN_POINT('Ctrl Pts',(374.352775640898,-17.0034157998264,-1.76136587694822));
#43760=CARTESIAN_POINT('Ctrl Pts',(374.403210869252,-17.0092707732502,-1.65678243353831));
#43761=CARTESIAN_POINT('Ctrl Pts',(374.448900700805,-17.015125746674,-1.55025154022651));
#43762=CARTESIAN_POINT('Ctrl Pts',(374.494642315913,-17.0209873559582,-1.44359990783055));
#43763=CARTESIAN_POINT('Ctrl Pts',(374.535627636522,-17.0268489652423,-1.33499680003465));
#43764=CARTESIAN_POINT('Ctrl Pts',(374.571708828526,-17.0327105745265,-1.22490722004938));
#43765=CARTESIAN_POINT('Ctrl Pts',(374.607814350344,-17.0385761363368,-1.11474340585184));
#43766=CARTESIAN_POINT('Ctrl Pts',(374.639009047908,-17.0444416981472,-1.00309152050713));
#43767=CARTESIAN_POINT('Ctrl Pts',(374.66519581373,-17.0503072599575,-0.890428577546521));
#43768=CARTESIAN_POINT('Ctrl Pts',(374.691420871026,-17.0561813986578,-0.777600893730893));
#43769=CARTESIAN_POINT('Ctrl Pts',(374.712623306707,-17.0620555373582,-0.663759606355524));
#43770=CARTESIAN_POINT('Ctrl Pts',(374.728757605958,-17.0679296760585,-0.549388762467288));
#43771=CARTESIAN_POINT('Ctrl Pts',(374.732837706844,-17.0694151498398,-0.520466243165366));
#43772=CARTESIAN_POINT('Ctrl Pts',(374.736593959772,-17.0709006236211,-0.49150986573407));
#43773=CARTESIAN_POINT('Ctrl Pts',(374.74002615638,-17.0723860974024,-0.462527459354832));
#43774=CARTESIAN_POINT('Ctrl Pts',(374.753597353027,-17.078259786793,-0.347928565046032));
#43775=CARTESIAN_POINT('Ctrl Pts',(374.762143142551,-17.0841334761836,-0.232541004059265));
#43776=CARTESIAN_POINT('Ctrl Pts',(374.765581858882,-17.0900071655741,-0.116843133392955));
#43777=CARTESIAN_POINT('Ctrl Pts',(374.769016135506,-17.0958732714799,-0.001294639547041));
#43778=CARTESIAN_POINT('Ctrl Pts',(374.767356439506,-17.1017393773857,0.114562958048043));
#43779=CARTESIAN_POINT('Ctrl Pts',(374.760572628855,-17.1076054832914,0.230244298159953));
#43780=CARTESIAN_POINT('Ctrl Pts',(374.75379576474,-17.1134655823795,0.345807182053286));
#43781=CARTESIAN_POINT('Ctrl Pts',(374.741905246791,-17.1193256814675,0.461193757478856));
#43782=CARTESIAN_POINT('Ctrl Pts',(374.724922961374,-17.1251857805555,0.575917435433359));
#43783=CARTESIAN_POINT('Ctrl Pts',(374.707327993842,-17.1312572986497,0.694780081961744));
#43784=CARTESIAN_POINT('Ctrl Pts',(374.684266910057,-17.1373288167438,0.812930644803329));
#43785=CARTESIAN_POINT('Ctrl Pts',(374.655822992546,-17.1434003348379,0.929831958010082));
#43786=CARTESIAN_POINT('Ctrl Pts',(374.628401087722,-17.1492536984346,1.04253291360825));
#43787=CARTESIAN_POINT('Ctrl Pts',(374.595976617167,-17.1551070620314,1.15407241182109));
#43788=CARTESIAN_POINT('Ctrl Pts',(374.558676307244,-17.1609604256281,1.26397907655505));
#43789=CARTESIAN_POINT('Ctrl Pts',(374.521381597838,-17.166812910362,1.37386923917312));
#43790=CARTESIAN_POINT('Ctrl Pts',(374.479212637476,-17.172665395096,1.48212666466833));
#43791=CARTESIAN_POINT('Ctrl Pts',(374.432345748655,-17.1785178798299,1.58829602520976));
#43792=CARTESIAN_POINT('Ctrl Pts',(374.385474562771,-17.184370901158,1.69447512005612));
#43793=CARTESIAN_POINT('Ctrl Pts',(374.333904759016,-17.1902239224862,1.7985653913906));
#43794=CARTESIAN_POINT('Ctrl Pts',(374.277860151588,-17.1960769438144,1.90013300570704));
#43795=CARTESIAN_POINT('Ctrl Pts',(374.221796852201,-17.2019319172382,2.00173449478428));
#43796=CARTESIAN_POINT('Ctrl Pts',(374.161255980997,-17.2077868906621,2.10081129231268));
#43797=CARTESIAN_POINT('Ctrl Pts',(374.096506127618,-17.2136418640859,2.19695622678428));
#43798=CARTESIAN_POINT('Ctrl Pts',(374.031682888597,-17.2195034733701,2.29321012918976));
#43799=CARTESIAN_POINT('Ctrl Pts',(373.962641376999,-17.2253650826542,2.38652519337903));
#43800=CARTESIAN_POINT('Ctrl Pts',(373.889692196396,-17.2312266919384,2.47652511053001));
#43801=CARTESIAN_POINT('Ctrl Pts',(373.816693825625,-17.2370922537487,2.56658571528611));
#43802=CARTESIAN_POINT('Ctrl Pts',(373.739782812457,-17.2429578155591,2.65332641340825));
#43803=CARTESIAN_POINT('Ctrl Pts',(373.659307352212,-17.2488233773694,2.73640701113821));
#43804=CARTESIAN_POINT('Ctrl Pts',(373.578714217107,-17.2546975160698,2.8196090930789));
#43805=CARTESIAN_POINT('Ctrl Pts',(373.494546532028,-17.2605716547701,2.89914011079338));
#43806=CARTESIAN_POINT('Ctrl Pts',(373.407186371495,-17.2664457934704,2.97469941131716));
#43807=CARTESIAN_POINT('Ctrl Pts',(373.385094413062,-17.2679312672517,2.99380712490413));
#43808=CARTESIAN_POINT('Ctrl Pts',(373.362798442319,-17.2694167410329,3.01266106132462));
#43809=CARTESIAN_POINT('Ctrl Pts',(373.340304925234,-17.2709022148141,3.03125680121626));
#43810=CARTESIAN_POINT('Ctrl Pts',(373.251363649844,-17.2767759042047,3.10478593481075));
#43811=CARTESIAN_POINT('Ctrl Pts',(373.159035330657,-17.2826495935952,3.17451972307088));
#43812=CARTESIAN_POINT('Ctrl Pts',(373.063677662859,-17.2885232829858,3.2401302194792));
#43813=CARTESIAN_POINT('Ctrl Pts',(372.96844311077,-17.2943893888915,3.30565600657279));
#43814=CARTESIAN_POINT('Ctrl Pts',(372.870187325365,-17.3002554947973,3.36706885657835));
#43815=CARTESIAN_POINT('Ctrl Pts',(372.76930181922,-17.306121600703,3.42408032197541));
#43816=CARTESIAN_POINT('Ctrl Pts',(372.668519618547,-17.3119816997911,3.48103340835827));
#43817=CARTESIAN_POINT('Ctrl Pts',(372.565113410884,-17.3178417988791,3.53359387279936));
#43818=CARTESIAN_POINT('Ctrl Pts',(372.459503945596,-17.3237018979671,3.5815163220571));
#43819=CARTESIAN_POINT('Ctrl Pts',(372.350084331733,-17.3297734160612,3.6311677039555));
#43820=CARTESIAN_POINT('Ctrl Pts',(372.238299853772,-17.3358449341553,3.67583983813364));
#43821=CARTESIAN_POINT('Ctrl Pts',(372.124647044722,-17.3419164522494,3.71531150478226));
#43822=CARTESIAN_POINT('Ctrl Pts',(372.015077871931,-17.3477698158462,3.75336492290316));
#43823=CARTESIAN_POINT('Ctrl Pts',(371.903772742432,-17.3536231794429,3.78658500868818));
#43824=CARTESIAN_POINT('Ctrl Pts',(371.791196456824,-17.3594765430397,3.81482271383259));
#43825=CARTESIAN_POINT('Ctrl Pts',(371.678637074166,-17.3653290277736,3.84305617918061));
#43826=CARTESIAN_POINT('Ctrl Pts',(371.564807315523,-17.3711815125075,3.86630865087828));
#43827=CARTESIAN_POINT('Ctrl Pts',(371.450185382546,-17.3770339972413,3.88448145655589));
#43828=CARTESIAN_POINT('Ctrl Pts',(371.335552940278,-17.3828870185695,3.90265592843578));
#43829=CARTESIAN_POINT('Ctrl Pts',(371.220128587361,-17.3887400398977,3.91574974375585));
#43830=CARTESIAN_POINT('Ctrl Pts',(371.104398209302,-17.3945930612258,3.92371579007204));
#43831=CARTESIAN_POINT('Ctrl Pts',(370.988629232927,-17.4004480346497,3.93168449321852));
#43832=CARTESIAN_POINT('Ctrl Pts',(370.872554440404,-17.4063030080735,3.93452199832939));
#43833=CARTESIAN_POINT('Ctrl Pts',(370.756661586145,-17.4121579814973,3.93223327184228));
#43834=CARTESIAN_POINT('Ctrl Pts',(370.640637382223,-17.4180195907814,3.92994195137766));
#43835=CARTESIAN_POINT('Ctrl Pts',(370.52479594143,-17.4238812000656,3.92251281121648));
#43836=CARTESIAN_POINT('Ctrl Pts',(370.409621860176,-17.4297428093497,3.91000285338626));
#43837=CARTESIAN_POINT('Ctrl Pts',(370.294370116192,-17.43560837116,3.8974844599996));
#43838=CARTESIAN_POINT('Ctrl Pts',(370.179787035149,-17.4414739329704,3.87987848954197));
#43839=CARTESIAN_POINT('Ctrl Pts',(370.066347244525,-17.4473394947807,3.85729311100074));
#43840=CARTESIAN_POINT('Ctrl Pts',(369.952741577103,-17.453213633481,3.83467470709667));
#43841=CARTESIAN_POINT('Ctrl Pts',(369.840282936222,-17.4590877721813,3.80706246196776));
#43842=CARTESIAN_POINT('Ctrl Pts',(369.729431089154,-17.4649619108817,3.77461444899779));
#43843=CARTESIAN_POINT('Ctrl Pts',(369.701398466699,-17.466447384663,3.76640887623504));
#43844=CARTESIAN_POINT('Ctrl Pts',(369.673468498175,-17.4679328584444,3.75789429531162));
#43845=CARTESIAN_POINT('Ctrl Pts',(369.645648402469,-17.4694183322257,3.74907374385222));
#43846=CARTESIAN_POINT('Ctrl Pts',(369.535645383201,-17.4752920216163,3.71419653485915));
#43847=CARTESIAN_POINT('Ctrl Pts',(369.426995473744,-17.4811657110069,3.67441567358145));
#43848=CARTESIAN_POINT('Ctrl Pts',(369.320168160092,-17.4870394003974,3.62985395116513));
#43849=CARTESIAN_POINT('Ctrl Pts',(369.213478770539,-17.4929055063032,3.58534976211886));
#43850=CARTESIAN_POINT('Ctrl Pts',(369.10860767498,-17.4987716122089,3.53607714469621));
#43851=CARTESIAN_POINT('Ctrl Pts',(369.006009500822,-17.5046377181147,3.48220871984097));
#43852=CARTESIAN_POINT('Ctrl Pts',(368.903516385887,-17.5104978172028,3.42839545556647));
#43853=CARTESIAN_POINT('Ctrl Pts',(368.803291926492,-17.5163579162908,3.36999593549393));
#43854=CARTESIAN_POINT('Ctrl Pts',(368.705770420738,-17.5222180153788,3.30723068860623));
#43855=CARTESIAN_POINT('Ctrl Pts',(368.604730561539,-17.528289533473,3.24220101480139));
#43856=CARTESIAN_POINT('Ctrl Pts',(368.506592787952,-17.5343610515671,3.17248482958971));
#43857=CARTESIAN_POINT('Ctrl Pts',(368.411812167986,-17.5404325696612,3.09837944819399));
#43858=CARTESIAN_POINT('Ctrl Pts',(368.320437091443,-17.5462859332579,3.02693673237529));
#43859=CARTESIAN_POINT('Ctrl Pts',(368.232182423347,-17.5521392968547,2.95141508308358));
#43860=CARTESIAN_POINT('Ctrl Pts',(368.147425382985,-17.5579926604514,2.87212427540527));
#43861=CARTESIAN_POINT('Ctrl Pts',(368.062681068607,-17.5638451451853,2.792845372975));
#43862=CARTESIAN_POINT('Ctrl Pts',(367.981433639376,-17.5696976299192,2.70979871960333));
#43863=CARTESIAN_POINT('Ctrl Pts',(367.904025248123,-17.5755501146531,2.62333266066097));
#43864=CARTESIAN_POINT('Ctrl Pts',(367.82660975956,-17.5814031359813,2.53685867394199));
#43865=CARTESIAN_POINT('Ctrl Pts',(367.753034284279,-17.5872561573095,2.44696496624837));
#43866=CARTESIAN_POINT('Ctrl Pts',(367.683601814389,-17.5931091786377,2.35403429087829));
#43867=CARTESIAN_POINT('Ctrl Pts',(367.614146187431,-17.5989641520615,2.26107262133322));
#43868=CARTESIAN_POINT('Ctrl Pts',(367.548836560604,-17.6048191254853,2.16507230082104));
#43869=CARTESIAN_POINT('Ctrl Pts',(367.48793317688,-17.6106740989091,2.06644588555582));
#43870=CARTESIAN_POINT('Ctrl Pts',(367.426960766993,-17.6165357081933,1.96770768991693));
#43871=CARTESIAN_POINT('Ctrl Pts',(367.370404784946,-17.6223973174774,1.86633781064752));
#43872=CARTESIAN_POINT('Ctrl Pts',(367.318480035809,-17.6282589267616,1.76277435925219));
#43873=CARTESIAN_POINT('Ctrl Pts',(367.266520273433,-17.634124488572,1.65914107426099));
#43874=CARTESIAN_POINT('Ctrl Pts',(367.219198130532,-17.6399900503823,1.55331164806737));
#43875=CARTESIAN_POINT('Ctrl Pts',(367.176680011928,-17.6458556121927,1.44574355330331));
#43876=CARTESIAN_POINT('Ctrl Pts',(367.134099721406,-17.651729750893,1.338018167602));
#43877=CARTESIAN_POINT('Ctrl Pts',(367.09633760885,-17.6576038895933,1.228549428478));
#43878=CARTESIAN_POINT('Ctrl Pts',(367.063510088167,-17.6634780282936,1.11780937506533));
#43879=CARTESIAN_POINT('Ctrl Pts',(367.055208544099,-17.6649635020749,1.08980502340273));
#43880=CARTESIAN_POINT('Ctrl Pts',(367.047222311687,-17.6664489758562,1.06171941638091));
#43881=CARTESIAN_POINT('Ctrl Pts',(367.039552751816,-17.6679344496374,1.0335602668127));
#43882=CARTESIAN_POINT('Ctrl Pts',(367.000890946421,-17.6754226366022,0.891611631032549));
#43883=CARTESIAN_POINT('Ctrl Pts',(366.970176145368,-17.682910823567,0.747412562252043));
#43884=CARTESIAN_POINT('Ctrl Pts',(366.947623622355,-17.6903990105317,0.60174492580523));
#43885=CARTESIAN_POINT('Ctrl Pts',(366.925476457884,-17.6977526049923,0.458695516182048));
#43886=CARTESIAN_POINT('Ctrl Pts',(366.911200774692,-17.7051061994529,0.314229690773424));
#43887=CARTESIAN_POINT('Ctrl Pts',(366.904955180256,-17.7124597939135,0.169109385555225));
#43888=CARTESIAN_POINT('Ctrl Pts',(366.902583670133,-17.7152520219197,0.114005859970163));
#43889=CARTESIAN_POINT('Ctrl Pts',(366.901369459675,-17.7180442499259,0.0588082087437617));
#43890=CARTESIAN_POINT('Ctrl Pts',(366.901319463554,-17.7208364779321,0.00355905278374745));
#43891=CARTESIAN_POINT('',(366.901318079705,-18.970836477995,-0.00133472881288598));
#43892=CARTESIAN_POINT('Ctrl Pts',(366.901319463554,-17.7208364779651,0.00355905213086757));
#43893=CARTESIAN_POINT('Ctrl Pts',(366.901210826618,-17.7269037316769,-0.116492263818606));
#43894=CARTESIAN_POINT('Ctrl Pts',(366.906603967799,-17.7329709853888,-0.236671020316424));
#43895=CARTESIAN_POINT('Ctrl Pts',(366.91750180444,-17.7390382391006,-0.356428169460981));
#43896=CARTESIAN_POINT('Ctrl Pts',(366.927912467658,-17.7448342642326,-0.470831733108454));
#43897=CARTESIAN_POINT('Ctrl Pts',(366.943346248658,-17.7506302893647,-0.584850100472219));
#43898=CARTESIAN_POINT('Ctrl Pts',(366.963752437188,-17.7564263144968,-0.698005988649075));
#43899=CARTESIAN_POINT('Ctrl Pts',(366.984153960437,-17.7622210145362,-0.811136007022495));
#43900=CARTESIAN_POINT('Ctrl Pts',(367.009525557066,-17.7680157145757,-0.923403522833011));
#43901=CARTESIAN_POINT('Ctrl Pts',(367.039765022357,-17.7738104146152,-1.03433931268109));
#43902=CARTESIAN_POINT('Ctrl Pts',(367.070005243591,-17.7796052595138,-1.14527787576476));
#43903=CARTESIAN_POINT('Ctrl Pts',(367.105113463762,-17.7854001044125,-1.25488423951657));
#43904=CARTESIAN_POINT('Ctrl Pts',(367.144937235379,-17.7911949493111,-1.36270306988447));
#43905=CARTESIAN_POINT('Ctrl Pts',(367.18477210334,-17.7969914088631,-1.4705519424782));
#43906=CARTESIAN_POINT('Ctrl Pts',(367.229324987372,-17.8027878684152,-1.57661189611944));
#43907=CARTESIAN_POINT('Ctrl Pts',(367.278395124978,-17.8085843279672,-1.6804471282203));
#43908=CARTESIAN_POINT('Ctrl Pts',(367.327519250044,-17.8143871648424,-1.78439660088862));
#43909=CARTESIAN_POINT('Ctrl Pts',(367.38117036646,-17.8201900017176,-1.88611608537424));
#43910=CARTESIAN_POINT('Ctrl Pts',(367.439101540829,-17.8259928385927,-1.98519399355422));
#43911=CARTESIAN_POINT('Ctrl Pts',(367.497070148194,-17.8317994250479,-2.08433592223832));
#43912=CARTESIAN_POINT('Ctrl Pts',(367.559324089116,-17.8376060115031,-2.18083252392297));
#43913=CARTESIAN_POINT('Ctrl Pts',(367.625573909863,-17.8434125979582,-2.27430237786089));
#43914=CARTESIAN_POINT('Ctrl Pts',(367.691922206198,-17.8492278154861,-2.36791116800698));
#43915=CARTESIAN_POINT('Ctrl Pts',(367.762277976017,-17.855043033014,-2.45848390128039));
#43916=CARTESIAN_POINT('Ctrl Pts',(367.836312460296,-17.8608582505418,-2.54567332232082));
#43917=CARTESIAN_POINT('Ctrl Pts',(367.860044691954,-17.8627223560442,-2.5736224538425));
#43918=CARTESIAN_POINT('Ctrl Pts',(367.884154662209,-17.8645864615467,-2.6012242220321));
#43919=CARTESIAN_POINT('Ctrl Pts',(367.908630796946,-17.8664505670491,-2.62846804217356));
#43920=CARTESIAN_POINT('Ctrl Pts',(367.985753691945,-17.8723242564397,-2.71431175494456));
#43921=CARTESIAN_POINT('Ctrl Pts',(368.066786396822,-17.8781979458302,-2.79690122454739));
#43922=CARTESIAN_POINT('Ctrl Pts',(368.151423500947,-17.8840716352208,-2.87585933149078));
#43923=CARTESIAN_POINT('Ctrl Pts',(368.23595133062,-17.8899377411266,-2.95471549610037));
#43924=CARTESIAN_POINT('Ctrl Pts',(368.324074005681,-17.8958038470324,-3.02994934254857));
#43925=CARTESIAN_POINT('Ctrl Pts',(368.415446841904,-17.9016699529381,-3.10121783023935));
#43926=CARTESIAN_POINT('Ctrl Pts',(368.506726113506,-17.9075300520262,-3.17241333990654));
#43927=CARTESIAN_POINT('Ctrl Pts',(368.601248602522,-17.9133901511142,-3.23965131485939));
#43928=CARTESIAN_POINT('Ctrl Pts',(368.698634357218,-17.9192502502022,-3.30262698542935));
#43929=CARTESIAN_POINT('Ctrl Pts',(368.79953356777,-17.9253217682963,-3.36787467452288));
#43930=CARTESIAN_POINT('Ctrl Pts',(368.903506214627,-17.9313932863905,-3.42854639603025));
#43931=CARTESIAN_POINT('Ctrl Pts',(369.010093825745,-17.9374648044846,-3.48435011122124));
#43932=CARTESIAN_POINT('Ctrl Pts',(369.112851658812,-17.9433181680813,-3.53814875432834));
#43933=CARTESIAN_POINT('Ctrl Pts',(369.218039377229,-17.9491715316781,-3.58742298539051));
#43934=CARTESIAN_POINT('Ctrl Pts',(369.32521924898,-17.9550248952748,-3.63195682830467));
#43935=CARTESIAN_POINT('Ctrl Pts',(369.432383028034,-17.9608773800087,-3.67648398461213));
#43936=CARTESIAN_POINT('Ctrl Pts',(369.54153798425,-17.9667298647427,-3.71627200952271));
#43937=CARTESIAN_POINT('Ctrl Pts',(369.652225700691,-17.9725823494766,-3.75115277520406));
#43938=CARTESIAN_POINT('Ctrl Pts',(369.76292356571,-17.9784353708047,-3.78603673898321));
#43939=CARTESIAN_POINT('Ctrl Pts',(369.875154076256,-17.9842883921329,-3.81601242493424));
#43940=CARTESIAN_POINT('Ctrl Pts',(369.988443610498,-17.9901414134611,-3.84096156782295));
#43941=CARTESIAN_POINT('Ctrl Pts',(370.101770928988,-17.9959963868849,-3.8659190317327));
#43942=CARTESIAN_POINT('Ctrl Pts',(370.216157570246,-18.0018513603087,-3.88584653022815));
#43943=CARTESIAN_POINT('Ctrl Pts',(370.33112038234,-18.0077063337326,-3.90067703165696));
#43944=CARTESIAN_POINT('Ctrl Pts',(370.446213490015,-18.0135679430167,-3.91552434155424));
#43945=CARTESIAN_POINT('Ctrl Pts',(370.561883661927,-18.0194295523009,-3.9252630713686));
#43946=CARTESIAN_POINT('Ctrl Pts',(370.677643194357,-18.0252911615851,-3.92987812168124));
#43947=CARTESIAN_POINT('Ctrl Pts',(370.79348078429,-18.0311567233954,-3.93449628395621));
#43948=CARTESIAN_POINT('Ctrl Pts',(370.909407442608,-18.0370222852058,-3.93398388900959));
#43949=CARTESIAN_POINT('Ctrl Pts',(371.024937778355,-18.0428878470161,-3.9283779151379));
#43950=CARTESIAN_POINT('Ctrl Pts',(371.140637047788,-18.0487619857165,-3.92276374395747));
#43951=CARTESIAN_POINT('Ctrl Pts',(371.255938428284,-18.0546361244168,-3.91204116750197));
#43952=CARTESIAN_POINT('Ctrl Pts',(371.370363865654,-18.0605102631172,-3.89629871449274));
#43953=CARTESIAN_POINT('Ctrl Pts',(371.399300190754,-18.0619957368983,-3.89231770512442));
#43954=CARTESIAN_POINT('Ctrl Pts',(371.428180563444,-18.0634812106795,-3.88801592605576));
#43955=CARTESIAN_POINT('Ctrl Pts',(371.456997395747,-18.0649666844607,-3.88339531690034));
#43956=CARTESIAN_POINT('Ctrl Pts',(371.570941596116,-18.0708403738513,-3.86512503618736));
#43957=CARTESIAN_POINT('Ctrl Pts',(371.684270775537,-18.0767140632418,-3.84180515537925));
#43958=CARTESIAN_POINT('Ctrl Pts',(371.796502471532,-18.0825877526324,-3.81348787336368));
#43959=CARTESIAN_POINT('Ctrl Pts',(371.908589265863,-18.0884538585381,-3.7852071516195));
#43960=CARTESIAN_POINT('Ctrl Pts',(372.019580997695,-18.0943199644439,-3.75194195995824));
#43961=CARTESIAN_POINT('Ctrl Pts',(372.129002550724,-18.1001860703496,-3.71379597367167));
#43962=CARTESIAN_POINT('Ctrl Pts',(372.238312057476,-18.1060461694377,-3.67568904838903));
#43963=CARTESIAN_POINT('Ctrl Pts',(372.346054195759,-18.1119062685257,-3.63271140485454));
#43964=CARTESIAN_POINT('Ctrl Pts',(372.451766889779,-18.1177663676138,-3.58501710095596));
#43965=CARTESIAN_POINT('Ctrl Pts',(372.56129345663,-18.1238378857079,-3.53560209538083));
#43966=CARTESIAN_POINT('Ctrl Pts',(372.668640941062,-18.129909403802,-3.4811237816107));
#43967=CARTESIAN_POINT('Ctrl Pts',(372.773315398583,-18.1359809218961,-3.42180910032845));
#43968=CARTESIAN_POINT('Ctrl Pts',(372.874228819192,-18.1418342854928,-3.36462564294782));
#43969=CARTESIAN_POINT('Ctrl Pts',(372.972657604813,-18.1476876490896,-3.30294760703959));
#43970=CARTESIAN_POINT('Ctrl Pts',(373.068182970345,-18.1535410126863,-3.23702573955043));
#43971=CARTESIAN_POINT('Ctrl Pts',(373.163693993064,-18.1593934974202,-3.17111377000791));
#43972=CARTESIAN_POINT('Ctrl Pts',(373.25630212256,-18.1652459821541,-3.10095947046653));
#43973=CARTESIAN_POINT('Ctrl Pts',(373.345617567513,-18.171098466888,-3.02685690857922));
#43974=CARTESIAN_POINT('Ctrl Pts',(373.434941201493,-18.1769514882162,-2.95274755248196));
#43975=CARTESIAN_POINT('Ctrl Pts',(373.520971232815,-18.1828045095444,-2.87468947822724));
#43976=CARTESIAN_POINT('Ctrl Pts',(373.603351527376,-18.1886575308725,-2.79301656124916));
#43977=CARTESIAN_POINT('Ctrl Pts',(373.685759297356,-18.1945125042964,-2.71131640477564));
#43978=CARTESIAN_POINT('Ctrl Pts',(373.764514616876,-18.2003674777202,-2.62599929897565));
#43979=CARTESIAN_POINT('Ctrl Pts',(373.839299237453,-18.206222451144,-2.53743490171398));
#43980=CARTESIAN_POINT('Ctrl Pts',(373.914168616792,-18.2120840604282,-2.44877012808402));
#43981=CARTESIAN_POINT('Ctrl Pts',(373.98505804821,-18.2179456697123,-2.35685103299713));
#43982=CARTESIAN_POINT('Ctrl Pts',(374.051690454723,-18.2238072789965,-2.26207925217577));
#43983=CARTESIAN_POINT('Ctrl Pts',(374.118367791957,-18.2296728408068,-2.16724356604643));
#43984=CARTESIAN_POINT('Ctrl Pts',(374.180782166516,-18.2355384026172,-2.06955171118823));
#43985=CARTESIAN_POINT('Ctrl Pts',(374.238701516499,-18.2414039644275,-1.96943161171589));
#43986=CARTESIAN_POINT('Ctrl Pts',(374.296705558777,-18.2472781031279,-1.86916511210221));
#43987=CARTESIAN_POINT('Ctrl Pts',(374.350201268639,-18.2531522418282,-1.76646364659903));
#43988=CARTESIAN_POINT('Ctrl Pts',(374.39900387974,-18.2590263805285,-1.66177692015447));
#43989=CARTESIAN_POINT('Ctrl Pts',(374.41134526338,-18.2605118543098,-1.63530335605997));
#43990=CARTESIAN_POINT('Ctrl Pts',(374.423386769389,-18.2619973280911,-1.60870291690914));
#43991=CARTESIAN_POINT('Ctrl Pts',(374.435125914126,-18.2634828018724,-1.58198303042164));
#43992=CARTESIAN_POINT('Ctrl Pts',(374.481543488617,-18.269356491263,-1.47633033176422));
#43993=CARTESIAN_POINT('Ctrl Pts',(374.523384435817,-18.2752301806536,-1.36845700379822));
#43994=CARTESIAN_POINT('Ctrl Pts',(374.560431071363,-18.2811038700441,-1.25879676104185));
#43995=CARTESIAN_POINT('Ctrl Pts',(374.597429876223,-18.2869699759499,-1.1492780999608));
#43996=CARTESIAN_POINT('Ctrl Pts',(374.6296465481,-18.2928360818556,-1.03797749994231));
#43997=CARTESIAN_POINT('Ctrl Pts',(374.65691064109,-18.2987021877614,-0.925350408305881));
#43998=CARTESIAN_POINT('Ctrl Pts',(374.684146815997,-18.3045622868495,-0.812838645376354));
#43999=CARTESIAN_POINT('Ctrl Pts',(374.70644040278,-18.3104223859375,-0.699003491781595));
#44000=CARTESIAN_POINT('Ctrl Pts',(374.723670361809,-18.3162824850256,-0.584316749682578));
#44001=CARTESIAN_POINT('Ctrl Pts',(374.741521938453,-18.3223540031197,-0.465492371571384));
#44002=CARTESIAN_POINT('Ctrl Pts',(374.753937476183,-18.3284255212138,-0.345754225987014));
#44003=CARTESIAN_POINT('Ctrl Pts',(374.760839903029,-18.3344970393079,-0.225640405064929));
#44004=CARTESIAN_POINT('Ctrl Pts',(374.767494320161,-18.3403504029046,-0.109842369720977));
#44005=CARTESIAN_POINT('Ctrl Pts',(374.76902496343,-18.3462037665014,0.0063043611136395));
#44006=CARTESIAN_POINT('Ctrl Pts',(374.765415510074,-18.3520571300981,0.122311946726538));
#44007=CARTESIAN_POINT('Ctrl Pts',(374.761806598665,-18.357909614832,0.238302114190843));
#44008=CARTESIAN_POINT('Ctrl Pts',(374.753059138041,-18.3637620995659,0.354152765140715));
#44009=CARTESIAN_POINT('Ctrl Pts',(374.739208925978,-18.3696145842998,0.46937693800074));
#44010=CARTESIAN_POINT('Ctrl Pts',(374.725357444036,-18.375467605628,0.584611675370635));
#44011=CARTESIAN_POINT('Ctrl Pts',(374.706402329915,-18.3813206269562,0.699219410251301));
#44012=CARTESIAN_POINT('Ctrl Pts',(374.682431078075,-18.3871736482844,0.812719883311904));
#44013=CARTESIAN_POINT('Ctrl Pts',(374.658451831359,-18.3930286217083,0.926258210972364));
#44014=CARTESIAN_POINT('Ctrl Pts',(374.629453205608,-18.3988835951321,1.03868813847992));
#44015=CARTESIAN_POINT('Ctrl Pts',(374.595573301698,-18.404738568556,1.1495418440936));
#44016=CARTESIAN_POINT('Ctrl Pts',(374.561654999269,-18.4106001778401,1.26052118814344));
#44017=CARTESIAN_POINT('Ctrl Pts',(374.522844497361,-18.4164617871243,1.36992034933774));
#44018=CARTESIAN_POINT('Ctrl Pts',(374.479329087555,-18.4223233964084,1.4772887671675));
#44019=CARTESIAN_POINT('Ctrl Pts',(374.435784334989,-18.4281889582188,1.58472958430979));
#44020=CARTESIAN_POINT('Ctrl Pts',(374.387528528816,-18.4340545200291,1.69013655669644));
#44021=CARTESIAN_POINT('Ctrl Pts',(374.334795454063,-18.4399200818394,1.79308269915879));
#44022=CARTESIAN_POINT('Ctrl Pts',(374.281985270622,-18.4457942205398,1.8961793741305));
#44023=CARTESIAN_POINT('Ctrl Pts',(374.224684956354,-18.4516683592401,1.99680768016255));
#44024=CARTESIAN_POINT('Ctrl Pts',(374.163172238265,-18.4575424979404,2.0945685673172));
#44025=CARTESIAN_POINT('Ctrl Pts',(374.147616676064,-18.4590279717216,2.119290699719));
#44026=CARTESIAN_POINT('Ctrl Pts',(374.131791933241,-18.4605134455028,2.14382962276991));
#44027=CARTESIAN_POINT('Ctrl Pts',(374.115702904964,-18.461998919284,2.1681792228086));
#44028=CARTESIAN_POINT('Ctrl Pts',(374.052085521813,-18.4678726086746,2.26445960770738));
#44029=CARTESIAN_POINT('Ctrl Pts',(373.984121093246,-18.4737462980651,2.35809804104824));
#44030=CARTESIAN_POINT('Ctrl Pts',(373.912056064212,-18.4796199874557,2.44867648018807));
#44031=CARTESIAN_POINT('Ctrl Pts',(373.8400840779,-18.4854860933614,2.53913797405344));
#44032=CARTESIAN_POINT('Ctrl Pts',(373.764022274544,-18.4913521992672,2.62654701009376));
#44033=CARTESIAN_POINT('Ctrl Pts',(373.684160969754,-18.4972183051729,2.71051345895347));
#44034=CARTESIAN_POINT('Ctrl Pts',(373.604381441921,-18.503078404261,2.79439392723967));
#44035=CARTESIAN_POINT('Ctrl Pts',(373.520810434497,-18.5089385033491,2.87483852260677));
#44036=CARTESIAN_POINT('Ctrl Pts',(373.433778789806,-18.5147986024371,2.95148976606502));
#44037=CARTESIAN_POINT('Ctrl Pts',(373.343607241924,-18.5208701205312,3.03090641151743));
#44038=CARTESIAN_POINT('Ctrl Pts',(373.249720919668,-18.5269416386254,3.10625047285099));
#44039=CARTESIAN_POINT('Ctrl Pts',(373.152530204631,-18.5330131567195,3.17716548101968));
#44040=CARTESIAN_POINT('Ctrl Pts',(373.058831629659,-18.5388665203162,3.24553245627108));
#44041=CARTESIAN_POINT('Ctrl Pts',(372.962062396585,-18.544719883913,3.30978291527873));
#44042=CARTESIAN_POINT('Ctrl Pts',(372.862623593065,-18.5505732475097,3.36963867880925));
#44043=CARTESIAN_POINT('Ctrl Pts',(372.763199719947,-18.5564257322436,3.42948545519824));
#44044=CARTESIAN_POINT('Ctrl Pts',(372.661107427249,-18.5622782169775,3.48493863512953));
#44045=CARTESIAN_POINT('Ctrl Pts',(372.556775318918,-18.5681307017114,3.535764313253));
#44046=CARTESIAN_POINT('Ctrl Pts',(372.452433644734,-18.5739837230396,3.58659465140874));
#44047=CARTESIAN_POINT('Ctrl Pts',(372.345852118116,-18.5798367443678,3.63279646338135));
#44048=CARTESIAN_POINT('Ctrl Pts',(372.237481736329,-18.585689765696,3.67418291830293));
#44049=CARTESIAN_POINT('Ctrl Pts',(372.129075210927,-18.5915447391198,3.71558317640636));
#44050=CARTESIAN_POINT('Ctrl Pts',(372.018879029757,-18.5973997125436,3.75216473665363));
#44051=CARTESIAN_POINT('Ctrl Pts',(371.907361172898,-18.6032546859674,3.78379003567901));
#44052=CARTESIAN_POINT('Ctrl Pts',(371.795716924871,-18.6091162952515,3.81545117791885));
#44053=CARTESIAN_POINT('Ctrl Pts',(371.68274840903,-18.6149779045357,3.84214473439152));
#44054=CARTESIAN_POINT('Ctrl Pts',(371.568935767455,-18.6208395138198,3.86378383454503));
#44055=CARTESIAN_POINT('Ctrl Pts',(371.455046381179,-18.6267050756302,3.88543752610263));
#44056=CARTESIAN_POINT('Ctrl Pts',(371.340312143645,-18.6325706374405,3.9020299157595));
#44057=CARTESIAN_POINT('Ctrl Pts',(371.225218590926,-18.6384361992508,3.91352598218839));
#44058=CARTESIAN_POINT('Ctrl Pts',(371.109956743205,-18.6443103379512,3.92503885868602));
#44059=CARTESIAN_POINT('Ctrl Pts',(370.994334942647,-18.6501844766515,3.93144051673639));
#44060=CARTESIAN_POINT('Ctrl Pts',(370.878839072497,-18.6560586153518,3.93274800375443));
#44061=CARTESIAN_POINT('Ctrl Pts',(370.84963205242,-18.6575440891331,3.93307864587641));
#44062=CARTESIAN_POINT('Ctrl Pts',(370.820433059223,-18.6590295629144,3.93308377387879));
#44063=CARTESIAN_POINT('Ctrl Pts',(370.791249883981,-18.6605150366957,3.93276418693331));
#44064=CARTESIAN_POINT('Ctrl Pts',(370.675857132547,-18.6663887260863,3.93150051303031));
#44065=CARTESIAN_POINT('Ctrl Pts',(370.560327859073,-18.6722624154769,3.92515175568437));
#44066=CARTESIAN_POINT('Ctrl Pts',(370.445146948226,-18.6781361048674,3.91369837962803));
#44067=CARTESIAN_POINT('Ctrl Pts',(370.330114746755,-18.6840022107732,3.90225979095617));
#44068=CARTESIAN_POINT('Ctrl Pts',(370.21543042083,-18.689868316679,3.88572973050901));
#44069=CARTESIAN_POINT('Ctrl Pts',(370.101579182062,-18.6957344225847,3.86414065993771));
#44070=CARTESIAN_POINT('Ctrl Pts',(369.987844525513,-18.7015945216727,3.84257369629974));
#44071=CARTESIAN_POINT('Ctrl Pts',(369.874941662792,-18.7074546207608,3.81595810322047));
#44072=CARTESIAN_POINT('Ctrl Pts',(369.763350339071,-18.7133147198488,3.78437809734019));
#44073=CARTESIAN_POINT('Ctrl Pts',(369.64773305497,-18.7193862379429,3.75165875689323));
#44074=CARTESIAN_POINT('Ctrl Pts',(369.533524180742,-18.725457756037,3.71361007580265));
#44075=CARTESIAN_POINT('Ctrl Pts',(369.42124573189,-18.7315292741311,3.67038365568348));
#44076=CARTESIAN_POINT('Ctrl Pts',(369.313001537436,-18.7373826377279,3.62871039538488));
#44077=CARTESIAN_POINT('Ctrl Pts',(369.206551850923,-18.7432360013246,3.58222523437972));
#44078=CARTESIAN_POINT('Ctrl Pts',(369.102347861977,-18.7490893649214,3.53111440616399));
#44079=CARTESIAN_POINT('Ctrl Pts',(368.998159518908,-18.7549418496553,3.48001125206714));
#44080=CARTESIAN_POINT('Ctrl Pts',(368.896216573787,-18.7607943343892,3.42428399363021));
#44081=CARTESIAN_POINT('Ctrl Pts',(368.796947929391,-18.7666468191231,3.36416598779867));
#44082=CARTESIAN_POINT('Ctrl Pts',(368.697670183393,-18.7724998404512,3.30404246995336));
#44083=CARTESIAN_POINT('Ctrl Pts',(368.601067578961,-18.7783528617794,3.23952761846563));
#44084=CARTESIAN_POINT('Ctrl Pts',(368.507541601444,-18.7842058831075,3.17089912708547));
#44085=CARTESIAN_POINT('Ctrl Pts',(368.413984431207,-18.7900608565313,3.10224774677808));
#44086=CARTESIAN_POINT('Ctrl Pts',(368.323506261179,-18.7959158299551,3.02948024274656));
#44087=CARTESIAN_POINT('Ctrl Pts',(368.236476383387,-18.8017708033789,2.95291528791404));
#44088=CARTESIAN_POINT('Ctrl Pts',(368.149347868407,-18.8076324126631,2.87626355653949));
#44089=CARTESIAN_POINT('Ctrl Pts',(368.065675756552,-18.8134940219472,2.79580605703821));
#44090=CARTESIAN_POINT('Ctrl Pts',(367.985793335415,-18.8193556312314,2.71189916321431));
#44091=CARTESIAN_POINT('Ctrl Pts',(367.905857048975,-18.8252211930417,2.62793569035545));
#44092=CARTESIAN_POINT('Ctrl Pts',(367.829715812337,-18.8310867548521,2.54051850245526));
#44093=CARTESIAN_POINT('Ctrl Pts',(367.75766226792,-18.8369523166624,2.45003661389321));
#44094=CARTESIAN_POINT('Ctrl Pts',(367.685503363549,-18.8428264553628,2.35942241861817));
#44095=CARTESIAN_POINT('Ctrl Pts',(367.617444322292,-18.8487005940631,2.26573491201658));
#44096=CARTESIAN_POINT('Ctrl Pts',(367.553734221,-18.8545747327634,2.16939162715773));
#44097=CARTESIAN_POINT('Ctrl Pts',(367.537622976458,-18.8560602065447,2.14502798323234));
#44098=CARTESIAN_POINT('Ctrl Pts',(367.521789615433,-18.857545680326,2.12049462005745));
#44099=CARTESIAN_POINT('Ctrl Pts',(367.506237689991,-18.8590311541073,2.0957985177716));
#44100=CARTESIAN_POINT('Ctrl Pts',(367.443144816677,-18.8650575981924,1.99560847644104));
#44101=CARTESIAN_POINT('Ctrl Pts',(367.384486334511,-18.8710840422775,1.89241860176349));
#44102=CARTESIAN_POINT('Ctrl Pts',(367.330551037451,-18.8771104863626,1.7866468875205));
#44103=CARTESIAN_POINT('Ctrl Pts',(367.276696694135,-18.8831278851054,1.68103393047141));
#44104=CARTESIAN_POINT('Ctrl Pts',(367.227551599139,-18.8891452838483,1.57284718607505));
#44105=CARTESIAN_POINT('Ctrl Pts',(367.183360883035,-18.8951626825911,1.4625328036765));
#44106=CARTESIAN_POINT('Ctrl Pts',(367.137049631408,-18.9014688322056,1.34692487577215));
#44107=CARTESIAN_POINT('Ctrl Pts',(367.096180300861,-18.9077749818201,1.22898037755567));
#44108=CARTESIAN_POINT('Ctrl Pts',(367.060981137706,-18.9140811314346,1.10924254846433));
#44109=CARTESIAN_POINT('Ctrl Pts',(367.02748605307,-18.9200819847541,0.995301523735869));
#44110=CARTESIAN_POINT('Ctrl Pts',(366.99912516879,-18.9260828380735,0.879737151549372));
#44111=CARTESIAN_POINT('Ctrl Pts',(366.976045925749,-18.932083691393,0.763037832388592));
#44112=CARTESIAN_POINT('Ctrl Pts',(366.952985535877,-18.938079642684,0.646433843567439));
#44113=CARTESIAN_POINT('Ctrl Pts',(366.935198273749,-18.944075593975,0.528697128891053));
#44114=CARTESIAN_POINT('Ctrl Pts',(366.922781205807,-18.9500715452659,0.41032920431667));
#44115=CARTESIAN_POINT('Ctrl Pts',(366.91037342804,-18.9560630105191,0.292049839999562));
#44116=CARTESIAN_POINT('Ctrl Pts',(366.903327879835,-18.9620544757722,0.17314058812312));
#44117=CARTESIAN_POINT('Ctrl Pts',(366.901690099519,-18.9680459410253,0.0541105422818254));
#44118=CARTESIAN_POINT('Ctrl Pts',(366.901435833031,-18.9689761200053,0.0356310482111091));
#44119=CARTESIAN_POINT('Ctrl Pts',(366.901311807065,-18.9699062989852,0.0171486531679969));
#44120=CARTESIAN_POINT('Ctrl Pts',(366.901318079705,-18.9708364779651,-0.00133472821883135));
#44121=CARTESIAN_POINT('',(366.901318910622,-20.2208364779229,-0.00288400549572383));
#44122=CARTESIAN_POINT('Ctrl Pts',(366.901318079705,-18.970836477995,-0.00133472881285637));
#44123=CARTESIAN_POINT('Ctrl Pts',(366.901360682557,-18.9771541147819,-0.126871096239978));
#44124=CARTESIAN_POINT('Ctrl Pts',(366.907417918414,-18.9834717515689,-0.252229964907151));
#44125=CARTESIAN_POINT('Ctrl Pts',(366.919413884164,-18.9897893883558,-0.376849987441945));
#44126=CARTESIAN_POINT('Ctrl Pts',(366.931459197123,-18.9961330136919,-0.501982653182976));
#44127=CARTESIAN_POINT('Ctrl Pts',(366.949492110904,-19.002476639028,-0.626370088264227));
#44128=CARTESIAN_POINT('Ctrl Pts',(366.973385122635,-19.008820264364,-0.749458104145278));
#44129=CARTESIAN_POINT('Ctrl Pts',(366.997328647286,-19.0151773009453,-0.872806344026037));
#44130=CARTESIAN_POINT('Ctrl Pts',(367.027156945381,-19.0215343375265,-0.994849386593892));
#44131=CARTESIAN_POINT('Ctrl Pts',(367.06269260094,-19.0278913741077,-1.11504796144853));
#44132=CARTESIAN_POINT('Ctrl Pts',(367.098341619796,-19.0342686904509,-1.23562998517139));
#44133=CARTESIAN_POINT('Ctrl Pts',(367.139734326602,-19.040646006794,-1.3543554840663));
#44134=CARTESIAN_POINT('Ctrl Pts',(367.186644262668,-19.0470233231372,-1.47070268129113));
#44135=CARTESIAN_POINT('Ctrl Pts',(367.212448102359,-19.0505313059311,-1.53470201016626));
#44136=CARTESIAN_POINT('Ctrl Pts',(367.239920520888,-19.0540392887251,-1.5979821369739));
#44137=CARTESIAN_POINT('Ctrl Pts',(367.269018002693,-19.057547271519,-1.66045956765047));
#44138=CARTESIAN_POINT('Ctrl Pts',(367.317738187542,-19.0634209609096,-1.76507040620682));
#44139=CARTESIAN_POINT('Ctrl Pts',(367.371147557887,-19.0692946503001,-1.86770937983961));
#44140=CARTESIAN_POINT('Ctrl Pts',(367.42906402566,-19.0751683396907,-1.96792666780601));
#44141=CARTESIAN_POINT('Ctrl Pts',(367.486905717833,-19.0810344455964,-2.06801456583865));
#44142=CARTESIAN_POINT('Ctrl Pts',(367.549242730345,-19.0869005515022,-2.16568664159388));
#44143=CARTESIAN_POINT('Ctrl Pts',(367.615845467115,-19.0927666574079,-2.26051421138093));
#44144=CARTESIAN_POINT('Ctrl Pts',(367.682380003531,-19.0986267564959,-2.35524467894446));
#44145=CARTESIAN_POINT('Ctrl Pts',(367.753171339751,-19.104486855584,-2.44713609813943));
#44146=CARTESIAN_POINT('Ctrl Pts',(367.82794498033,-19.110346954672,-2.53578610082354));
#44147=CARTESIAN_POINT('Ctrl Pts',(367.905416283276,-19.1164184727661,-2.62763439336167));
#44148=CARTESIAN_POINT('Ctrl Pts',(367.987162434697,-19.1224899908602,-2.71600257662339));
#44149=CARTESIAN_POINT('Ctrl Pts',(368.072830120906,-19.1285615089543,-2.80047754932223));
#44150=CARTESIAN_POINT('Ctrl Pts',(368.155419698686,-19.1344148725511,-2.88191726874117));
#44151=CARTESIAN_POINT('Ctrl Pts',(368.241653533961,-19.1402682361478,-2.95973842014678));
#44152=CARTESIAN_POINT('Ctrl Pts',(368.331175957581,-19.1461215997446,-3.03360670659181));
#44153=CARTESIAN_POINT('Ctrl Pts',(368.420684939711,-19.1519740844785,-3.1074639019622));
#44154=CARTESIAN_POINT('Ctrl Pts',(368.513481209804,-19.1578265692124,-3.17736914961774));
#44155=CARTESIAN_POINT('Ctrl Pts',(368.609175352991,-19.1636790539462,-3.24302788357669));
#44156=CARTESIAN_POINT('Ctrl Pts',(368.704878270046,-19.1695320752744,-3.30869263755996));
#44157=CARTESIAN_POINT('Ctrl Pts',(368.80347924769,-19.1753850966026,-3.37010987010404));
#44158=CARTESIAN_POINT('Ctrl Pts',(368.90455977919,-19.1812381179307,-3.42702827179763));
#44159=CARTESIAN_POINT('Ctrl Pts',(369.005674022999,-19.1870930913546,-3.48396565687741));
#44160=CARTESIAN_POINT('Ctrl Pts',(369.109269105275,-19.1929480647784,-3.53640102493135));
#44161=CARTESIAN_POINT('Ctrl Pts',(369.214902455271,-19.1988030382022,-3.58412929020052));
#44162=CARTESIAN_POINT('Ctrl Pts',(369.320655527102,-19.2046646474863,-3.63191164932791));
#44163=CARTESIAN_POINT('Ctrl Pts',(369.428451100795,-19.2105262567705,-3.67497608733073));
#44164=CARTESIAN_POINT('Ctrl Pts',(369.537827099443,-19.2163878660546,-3.71316586289387));
#44165=CARTESIAN_POINT('Ctrl Pts',(369.64727685113,-19.222253427865,-3.75138139010318));
#44166=CARTESIAN_POINT('Ctrl Pts',(369.758308755084,-19.2281189896753,-3.7847155911826));
#44167=CARTESIAN_POINT('Ctrl Pts',(369.870447751639,-19.2339845514857,-3.81306221130359));
#44168=CARTESIAN_POINT('Ctrl Pts',(369.982750722912,-19.239858690186,-3.84145028113563));
#44169=CARTESIAN_POINT('Ctrl Pts',(370.096163614508,-19.2457328288863,-3.86483613176681));
#44170=CARTESIAN_POINT('Ctrl Pts',(370.210203343254,-19.2516069675866,-3.88316495637836));
#44171=CARTESIAN_POINT('Ctrl Pts',(370.239042128942,-19.253092441368,-3.88780001690246));
#44172=CARTESIAN_POINT('Ctrl Pts',(370.267920988874,-19.2545779151493,-3.89211193979668));
#44173=CARTESIAN_POINT('Ctrl Pts',(370.296832099317,-19.2560633889306,-3.89610036630829));
#44174=CARTESIAN_POINT('Ctrl Pts',(370.411149083444,-19.2619370783212,-3.91187094319813));
#44175=CARTESIAN_POINT('Ctrl Pts',(370.526351146057,-19.2678107677117,-3.92263219398958));
#44176=CARTESIAN_POINT('Ctrl Pts',(370.641961587585,-19.2736844571023,-3.92829327661127));
#44177=CARTESIAN_POINT('Ctrl Pts',(370.757422765171,-19.279550563008,-3.93394705024346));
#44178=CARTESIAN_POINT('Ctrl Pts',(370.873290864252,-19.2854166689138,-3.93451373068495));
#44179=CARTESIAN_POINT('Ctrl Pts',(370.989081192337,-19.2912827748195,-3.92995385581899));
#44180=CARTESIAN_POINT('Ctrl Pts',(371.104752952602,-19.2971428739076,-3.9253986502068));
#44181=CARTESIAN_POINT('Ctrl Pts',(371.220346689904,-19.3030029729956,-3.9157273471927));
#44182=CARTESIAN_POINT('Ctrl Pts',(371.335375484545,-19.3088630720836,-3.90095247985606));
#44183=CARTESIAN_POINT('Ctrl Pts',(371.454554255674,-19.3149345901777,-3.88564456901275));
#44184=CARTESIAN_POINT('Ctrl Pts',(371.573126099686,-19.3210061082718,-3.8648578691115));
#44185=CARTESIAN_POINT('Ctrl Pts',(371.690552349617,-19.3270776263659,-3.83866532628028));
#44186=CARTESIAN_POINT('Ctrl Pts',(371.803759380543,-19.3329309899627,-3.81341390244562));
#44187=CARTESIAN_POINT('Ctrl Pts',(371.915901287021,-19.3387843535594,-3.78313852030409));
#44188=CARTESIAN_POINT('Ctrl Pts',(372.026504345074,-19.3446377171562,-3.74795682587877));
#44189=CARTESIAN_POINT('Ctrl Pts',(372.137090796449,-19.35049020189,-3.71278041386648));
#44190=CARTESIAN_POINT('Ctrl Pts',(372.246138465218,-19.3563426866239,-3.67269927954016));
#44191=CARTESIAN_POINT('Ctrl Pts',(372.35318871977,-19.3621951713578,-3.62788096424845));
#44192=CARTESIAN_POINT('Ctrl Pts',(372.460248789394,-19.368048192686,-3.58305853971897));
#44193=CARTESIAN_POINT('Ctrl Pts',(372.56531069963,-19.3739012140142,-3.53349823036469));
#44194=CARTESIAN_POINT('Ctrl Pts',(372.667936396727,-19.3797542353423,-3.47941547345534));
#44195=CARTESIAN_POINT('Ctrl Pts',(372.770596321477,-19.3856092087661,-3.42531467890212));
#44196=CARTESIAN_POINT('Ctrl Pts',(372.870818052119,-19.3914641821899,-3.36668863006954));
#44197=CARTESIAN_POINT('Ctrl Pts',(372.96818933167,-19.3973191556137,-3.30379804368741));
#44198=CARTESIAN_POINT('Ctrl Pts',(373.065670969061,-19.4031807648979,-3.24083617890363));
#44199=CARTESIAN_POINT('Ctrl Pts',(373.160295359994,-19.409042374182,-3.17360035386299));
#44200=CARTESIAN_POINT('Ctrl Pts',(373.251680297225,-19.4149039834662,-3.10239388445946));
#44201=CARTESIAN_POINT('Ctrl Pts',(373.343126855991,-19.4207695452765,-3.03113940001062));
#44202=CARTESIAN_POINT('Ctrl Pts',(373.431329297897,-19.4266351070868,-2.95590920727541));
#44203=CARTESIAN_POINT('Ctrl Pts',(373.515940801815,-19.4325006688972,-2.87704490086488));
#44204=CARTESIAN_POINT('Ctrl Pts',(373.600676028503,-19.4383748075975,-2.79806527549567));
#44205=CARTESIAN_POINT('Ctrl Pts',(373.681809549507,-19.4442489462978,-2.71544122476306));
#44206=CARTESIAN_POINT('Ctrl Pts',(373.759033426244,-19.4501230849981,-2.62954897595268));
#44207=CARTESIAN_POINT('Ctrl Pts',(373.778562083983,-19.4516085587795,-2.60782822842825));
#44208=CARTESIAN_POINT('Ctrl Pts',(373.797840931265,-19.4530940325609,-2.58589863021964));
#44209=CARTESIAN_POINT('Ctrl Pts',(373.816865425307,-19.4545795063423,-2.56376656118758));
#44210=CARTESIAN_POINT('Ctrl Pts',(373.892089889188,-19.4604531957329,-2.47625448208237));
#44211=CARTESIAN_POINT('Ctrl Pts',(373.963584786505,-19.4663268851236,-2.38528306125726));
#44212=CARTESIAN_POINT('Ctrl Pts',(374.03101535858,-19.4722005745142,-2.29120362675335));
#44213=CARTESIAN_POINT('Ctrl Pts',(374.098358871452,-19.47806668042,-2.19724565763779));
#44214=CARTESIAN_POINT('Ctrl Pts',(374.161648256009,-19.4839327863259,-2.10018798759542));
#44215=CARTESIAN_POINT('Ctrl Pts',(374.220587595515,-19.4897988922317,-2.00041651473943));
#44216=CARTESIAN_POINT('Ctrl Pts',(374.279466581889,-19.4956589913198,-1.90074720660059));
#44217=CARTESIAN_POINT('Ctrl Pts',(374.334004174478,-19.5015190904079,-1.79836997670861));
#44218=CARTESIAN_POINT('Ctrl Pts',(374.383946941129,-19.507379189496,-1.69370078180889));
#44219=CARTESIAN_POINT('Ctrl Pts',(374.435691528861,-19.5134507075901,-1.58525536114756));
#44220=CARTESIAN_POINT('Ctrl Pts',(374.482503226193,-19.5195222256841,-1.47434984244847));
#44221=CARTESIAN_POINT('Ctrl Pts',(374.524151313843,-19.5255937437782,-1.3614764165776));
#44222=CARTESIAN_POINT('Ctrl Pts',(374.56430295242,-19.531447107375,-1.25265862310272));
#44223=CARTESIAN_POINT('Ctrl Pts',(374.599655505314,-19.5373004709719,-1.142012326479));
#44224=CARTESIAN_POINT('Ctrl Pts',(374.630051021127,-19.5431538345687,-1.02999937770978));
#44225=CARTESIAN_POINT('Ctrl Pts',(374.660441973156,-19.5490063193026,-0.918003247307915));
#44226=CARTESIAN_POINT('Ctrl Pts',(374.685877259849,-19.5548588040366,-0.804641271390275));
#44227=CARTESIAN_POINT('Ctrl Pts',(374.706249038959,-19.5607112887706,-0.690389667455808));
#44228=CARTESIAN_POINT('Ctrl Pts',(374.726622685888,-19.5665643100988,-0.576127588183244));
#44229=CARTESIAN_POINT('Ctrl Pts',(374.741931829811,-19.5724173314271,-0.460976125498675));
#44230=CARTESIAN_POINT('Ctrl Pts',(374.752120031252,-19.5782703527553,-0.34542016999933));
#44231=CARTESIAN_POINT('Ctrl Pts',(374.762311630654,-19.5841253261792,-0.22982567435726));
#44232=CARTESIAN_POINT('Ctrl Pts',(374.767378855159,-19.5899802996031,-0.113826828971878));
#44233=CARTESIAN_POINT('Ctrl Pts',(374.76731729865,-19.595835273027,0.00208860636006148));
#44234=CARTESIAN_POINT('Ctrl Pts',(374.767255672375,-19.6016968823112,0.118135416949179));
#44235=CARTESIAN_POINT('Ctrl Pts',(374.762053663277,-19.6075584915954,0.234098215423539));
#44236=CARTESIAN_POINT('Ctrl Pts',(374.751758951901,-19.6134201008796,0.349491399606124));
#44237=CARTESIAN_POINT('Ctrl Pts',(374.741457298725,-19.61928566269,0.464962394260245));
#44238=CARTESIAN_POINT('Ctrl Pts',(374.726056160073,-19.6251512245004,0.579862601334531));
#44239=CARTESIAN_POINT('Ctrl Pts',(374.705654565544,-19.6310167863108,0.693715402625332));
#44240=CARTESIAN_POINT('Ctrl Pts',(374.685223138881,-19.6368909250112,0.807734684635805));
#44241=CARTESIAN_POINT('Ctrl Pts',(374.659776754079,-19.6427650637116,0.920703102748728));
#44242=CARTESIAN_POINT('Ctrl Pts',(374.629464621444,-19.648639202412,1.03215793736561));
#44243=CARTESIAN_POINT('Ctrl Pts',(374.621799177954,-19.6501246761927,1.0603430455137));
#44244=CARTESIAN_POINT('Ctrl Pts',(374.61382281097,-19.6516101499733,1.08843145591653));
#44245=CARTESIAN_POINT('Ctrl Pts',(374.605538418854,-19.6530956237539,1.11641589265502));
#44246=CARTESIAN_POINT('Ctrl Pts',(374.572781229388,-19.6589693131444,1.22706873036416));
#44247=CARTESIAN_POINT('Ctrl Pts',(374.535095294422,-19.6648430025348,1.33646292607124));
#44248=CARTESIAN_POINT('Ctrl Pts',(374.492594361804,-19.6707166919253,1.44412672115984));
#44249=CARTESIAN_POINT('Ctrl Pts',(374.450148301883,-19.676582797831,1.55165151217438));
#44250=CARTESIAN_POINT('Ctrl Pts',(374.402899757431,-19.6824489037366,1.65744996470563));
#44251=CARTESIAN_POINT('Ctrl Pts',(374.351012582384,-19.6883150096423,1.76106421856201));
#44252=CARTESIAN_POINT('Ctrl Pts',(374.299178539143,-19.6941751087302,1.86457237274251));
#44253=CARTESIAN_POINT('Ctrl Pts',(374.242715497142,-19.7000352078182,1.96590040979602));
#44254=CARTESIAN_POINT('Ctrl Pts',(374.181835600117,-19.7058953069061,2.06460987458625));
#44255=CARTESIAN_POINT('Ctrl Pts',(374.118759295294,-19.7119668250002,2.16688055167612));
#44256=CARTESIAN_POINT('Ctrl Pts',(374.050941583983,-19.7180383430944,2.26633972479668));
#44257=CARTESIAN_POINT('Ctrl Pts',(373.978670982913,-19.7241098611885,2.3625266973765));
#44258=CARTESIAN_POINT('Ctrl Pts',(373.908997122298,-19.7299632247852,2.45525759515865));
#44259=CARTESIAN_POINT('Ctrl Pts',(373.835185126145,-19.7358165883818,2.54494703252978));
#44260=CARTESIAN_POINT('Ctrl Pts',(373.757537464523,-19.7416699519785,2.63121190786983));
#44261=CARTESIAN_POINT('Ctrl Pts',(373.679901461436,-19.7475224367123,2.71746383082914));
#44262=CARTESIAN_POINT('Ctrl Pts',(373.598431214332,-19.7533749214461,2.80029190716383));
#44263=CARTESIAN_POINT('Ctrl Pts',(373.513468430205,-19.7592274061799,2.8793473541516));
#44264=CARTESIAN_POINT('Ctrl Pts',(373.428497856132,-19.765080427508,2.95841004946246));
#44265=CARTESIAN_POINT('Ctrl Pts',(373.34003441095,-19.7709334488361,3.03369914636178));
#44266=CARTESIAN_POINT('Ctrl Pts',(373.248454955657,-19.7767864701641,3.1049043545102));
#44267=CARTESIAN_POINT('Ctrl Pts',(373.156844956847,-19.7826414435879,3.17613331097065));
#44268=CARTESIAN_POINT('Ctrl Pts',(373.062117207405,-19.7884964170116,3.24327541683511));
#44269=CARTESIAN_POINT('Ctrl Pts',(372.964679187118,-19.7943513904353,3.3060625503836));
#44270=CARTESIAN_POINT('Ctrl Pts',(372.867130733351,-19.8002129997194,3.36892084508327));
#44271=CARTESIAN_POINT('Ctrl Pts',(372.766866225204,-19.8060746090034,3.42741409199333));
#44272=CARTESIAN_POINT('Ctrl Pts',(372.664319566075,-19.8119362182875,3.48131910789031));
#44273=CARTESIAN_POINT('Ctrl Pts',(372.561703758981,-19.8178017800978,3.53526047233538));
#44274=CARTESIAN_POINT('Ctrl Pts',(372.456803109591,-19.823667341908,3.58460726974267));
#44275=CARTESIAN_POINT('Ctrl Pts',(372.35007180881,-19.8295329037182,3.62918433620061));
#44276=CARTESIAN_POINT('Ctrl Pts',(372.243184440691,-19.8354070424185,3.67382658526298));
#44277=CARTESIAN_POINT('Ctrl Pts',(372.134461465246,-19.8412811811187,3.71368504233485));
#44278=CARTESIAN_POINT('Ctrl Pts',(372.024372597712,-19.847155319819,3.74863424531133));
#44279=CARTESIAN_POINT('Ctrl Pts',(371.996532920309,-19.8486407936012,3.75747232819979));
#44280=CARTESIAN_POINT('Ctrl Pts',(371.968605944197,-19.8501262673834,3.76599671886881));
#44281=CARTESIAN_POINT('Ctrl Pts',(371.940599354617,-19.8516117411656,3.77420590848924));
#44282=CARTESIAN_POINT('Ctrl Pts',(371.829858922811,-19.8574854305561,3.80666574087095));
#44283=CARTESIAN_POINT('Ctrl Pts',(371.717504217943,-19.8633591199467,3.83430158793234));
#44284=CARTESIAN_POINT('Ctrl Pts',(371.603993326271,-19.8692328093372,3.85695328804873));
#44285=CARTESIAN_POINT('Ctrl Pts',(371.490628987824,-19.8750989152429,3.87957574269224));
#44286=CARTESIAN_POINT('Ctrl Pts',(371.37611183261,-19.8809650211486,3.897226767387));
#44287=CARTESIAN_POINT('Ctrl Pts',(371.260915430919,-19.8868311270543,3.90979583951701));
#44288=CARTESIAN_POINT('Ctrl Pts',(371.145836988876,-19.8926912261422,3.92235204107728));
#44289=CARTESIAN_POINT('Ctrl Pts',(371.030081092109,-19.8985513252302,3.92983659642516));
#44290=CARTESIAN_POINT('Ctrl Pts',(370.914131183045,-19.9044114243182,3.93219008090693));
#44291=CARTESIAN_POINT('Ctrl Pts',(370.793998065785,-19.9104829424123,3.93462847373969));
#44292=CARTESIAN_POINT('Ctrl Pts',(370.673657115819,-19.9165544605065,3.93155848245061));
#44293=CARTESIAN_POINT('Ctrl Pts',(370.553651867755,-19.9226259786006,3.92297280191958));
#44294=CARTESIAN_POINT('Ctrl Pts',(370.437958504162,-19.9284793421973,3.91469561175165));
#44295=CARTESIAN_POINT('Ctrl Pts',(370.322577580986,-19.934332705794,3.90129230920255));
#44296=CARTESIAN_POINT('Ctrl Pts',(370.207994993426,-19.9401860693907,3.88280937921176));
#44297=CARTESIAN_POINT('Ctrl Pts',(370.093429610056,-19.9460385541245,3.86432922437072));
#44298=CARTESIAN_POINT('Ctrl Pts',(369.979662731724,-19.9518910388584,3.84077102437501));
#44299=CARTESIAN_POINT('Ctrl Pts',(369.867172685898,-19.9577435235922,3.81223283986149));
#44300=CARTESIAN_POINT('Ctrl Pts',(369.754672326246,-19.9635965449203,3.78369203877961));
#44301=CARTESIAN_POINT('Ctrl Pts',(369.643449432302,-19.9694495662484,3.75017044710643));
#44302=CARTESIAN_POINT('Ctrl Pts',(369.533969043405,-19.9753025875765,3.71181653275089));
#44303=CARTESIAN_POINT('Ctrl Pts',(369.424452140684,-19.9811575610003,3.67344982662421));
#44304=CARTESIAN_POINT('Ctrl Pts',(369.316679288319,-19.9870125344241,3.63024772959784));
#44305=CARTESIAN_POINT('Ctrl Pts',(369.211096689763,-19.9928675078478,3.58240729879948));
#44306=CARTESIAN_POINT('Ctrl Pts',(369.105394426893,-19.9987291171319,3.53451264701771));
#44307=CARTESIAN_POINT('Ctrl Pts',(369.001887749023,-20.004590726416,3.4819693395051));
#44308=CARTESIAN_POINT('Ctrl Pts',(368.900999421924,-20.0104523357001,3.42502099894235));
#44309=CARTESIAN_POINT('Ctrl Pts',(368.800043065086,-20.0163178975104,3.36803425769536));
#44310=CARTESIAN_POINT('Ctrl Pts',(368.701708924245,-20.0221834593206,3.30663678704779));
#44311=CARTESIAN_POINT('Ctrl Pts',(368.606390412219,-20.0280490211309,3.24111528915836));
#44312=CARTESIAN_POINT('Ctrl Pts',(368.51093252115,-20.0339231598312,3.17549798276875));
#44313=CARTESIAN_POINT('Ctrl Pts',(368.418499387841,-20.0397972985315,3.10574486200305));
#44314=CARTESIAN_POINT('Ctrl Pts',(368.32945107618,-20.0456714372317,3.0321826180591));
#44315=CARTESIAN_POINT('Ctrl Pts',(368.306932211876,-20.0471569110136,3.01357992747079));
#44316=CARTESIAN_POINT('Ctrl Pts',(368.284629620145,-20.0486423847955,2.9947338235567));
#44317=CARTESIAN_POINT('Ctrl Pts',(368.262548735111,-20.0501278585773,2.97564994633464));
#44318=CARTESIAN_POINT('Ctrl Pts',(368.176502957271,-20.0559165190782,2.90128304223486));
#44319=CARTESIAN_POINT('Ctrl Pts',(368.093522159799,-20.0617051795791,2.82303935525769));
#44320=CARTESIAN_POINT('Ctrl Pts',(368.013983734837,-20.0674938400799,2.74120492861447));
#44321=CARTESIAN_POINT('Ctrl Pts',(367.934548696519,-20.0732749762907,2.65947687303393));
#44322=CARTESIAN_POINT('Ctrl Pts',(367.858547431796,-20.0790561125014,2.574167656681));
#44323=CARTESIAN_POINT('Ctrl Pts',(367.78632452466,-20.0848372487121,2.48560368301691));
#44324=CARTESIAN_POINT('Ctrl Pts',(367.714182760477,-20.0906118897749,2.39713921161277));
#44325=CARTESIAN_POINT('Ctrl Pts',(367.645811177665,-20.0963865308376,2.30542758485855));
#44326=CARTESIAN_POINT('Ctrl Pts',(367.581517011793,-20.1021611719003,2.21083144676017));
#44327=CARTESIAN_POINT('Ctrl Pts',(367.517262887755,-20.1079322165679,2.11629422229607));
#44328=CARTESIAN_POINT('Ctrl Pts',(367.457081374441,-20.1137032612354,2.01887640667268));
#44329=CARTESIAN_POINT('Ctrl Pts',(367.401238614753,-20.119474305903,1.91897262679348));
#44330=CARTESIAN_POINT('Ctrl Pts',(367.3454162108,-20.1252432469165,1.81910526371693));
#44331=CARTESIAN_POINT('Ctrl Pts',(367.293929624938,-20.13101218793,1.71675410887057));
#44332=CARTESIAN_POINT('Ctrl Pts',(367.247000467295,-20.1367811289435,1.61234083636549));
#44333=CARTESIAN_POINT('Ctrl Pts',(367.200076297233,-20.1425494568401,1.50793866079034));
#44334=CARTESIAN_POINT('Ctrl Pts',(367.157708765978,-20.1483177847368,1.40147519241846));
#44335=CARTESIAN_POINT('Ctrl Pts',(367.120072119742,-20.1540861126335,1.29339384230438));
#44336=CARTESIAN_POINT('Ctrl Pts',(367.082410796346,-20.1598582226405,1.185241626664));
#44337=CARTESIAN_POINT('Ctrl Pts',(367.049486696699,-20.1656303326475,1.07546981267461));
#44338=CARTESIAN_POINT('Ctrl Pts',(367.021424697576,-20.1714024426545,0.964538637699085));
#44339=CARTESIAN_POINT('Ctrl Pts',(366.993353773675,-20.1771763884111,0.853572182409189));
#44340=CARTESIAN_POINT('Ctrl Pts',(366.970148118481,-20.1829503341676,0.741446048957956));
#44341=CARTESIAN_POINT('Ctrl Pts',(366.95188144196,-20.1887242799242,0.62863066461313));
#44342=CARTESIAN_POINT('Ctrl Pts',(366.933590720042,-20.1945058262322,0.515666775386035));
#44343=CARTESIAN_POINT('Ctrl Pts',(366.92025201549,-20.2002873725403,0.402012246335616));
#44344=CARTESIAN_POINT('Ctrl Pts',(366.911887134562,-20.2060689188483,0.288142772418037));
#44345=CARTESIAN_POINT('Ctrl Pts',(366.904765114104,-20.2109914385398,0.191192112895476));
#44346=CARTESIAN_POINT('Ctrl Pts',(366.901247804181,-20.2159139582314,0.0940858361474233));
#44347=CARTESIAN_POINT('Ctrl Pts',(366.901318910622,-20.2208364779229,-0.00288400549575217));
#44348=CARTESIAN_POINT('',(366.901319072764,-21.4708364780021,0.00309724080919957));
#44349=CARTESIAN_POINT('Ctrl Pts',(366.901318910622,-20.2208364779651,-0.00288400632674463));
#44350=CARTESIAN_POINT('Ctrl Pts',(366.901452804976,-20.230105643973,-0.185479428239274));
#44351=CARTESIAN_POINT('Ctrl Pts',(366.914303573141,-20.239374809981,-0.367615513842659));
#44352=CARTESIAN_POINT('Ctrl Pts',(366.939675353735,-20.248643975989,-0.547949633793549));
#44353=CARTESIAN_POINT('Ctrl Pts',(366.95575295536,-20.2545176653786,-0.662223842069158));
#44354=CARTESIAN_POINT('Ctrl Pts',(366.976891041824,-20.2603913547682,-0.775980165170206));
#44355=CARTESIAN_POINT('Ctrl Pts',(367.003046693838,-20.2662650441578,-0.88873522674322));
#44356=CARTESIAN_POINT('Ctrl Pts',(367.029168576447,-20.2721311500625,-1.00134471093884));
#44357=CARTESIAN_POINT('Ctrl Pts',(367.060295049186,-20.2779972559673,-1.11295510562502));
#44358=CARTESIAN_POINT('Ctrl Pts',(367.096331584714,-20.2838633618721,-1.22308939020565));
#44359=CARTESIAN_POINT('Ctrl Pts',(367.132331219289,-20.2897234609591,-1.33311089868209));
#44360=CARTESIAN_POINT('Ctrl Pts',(367.173230788142,-20.2955835600462,-1.44165891326165));
#44361=CARTESIAN_POINT('Ctrl Pts',(367.218885140078,-20.3014436591332,-1.54826848340756));
#44362=CARTESIAN_POINT('Ctrl Pts',(367.266186596888,-20.3075151772277,-1.65872428365451));
#44363=CARTESIAN_POINT('Ctrl Pts',(367.318592295747,-20.3135866953222,-1.76709868937213));
#44364=CARTESIAN_POINT('Ctrl Pts',(367.375884828439,-20.3196582134167,-1.87289348684829));
#44365=CARTESIAN_POINT('Ctrl Pts',(367.431118794632,-20.3255115770124,-1.97488699267859));
#44366=CARTESIAN_POINT('Ctrl Pts',(367.490894249033,-20.3313649406082,-2.07448268033402));
#44367=CARTESIAN_POINT('Ctrl Pts',(367.554968537456,-20.3372183042039,-2.17125702420816));
#44368=CARTESIAN_POINT('Ctrl Pts',(367.619033205341,-20.3430707889368,-2.26801683774035));
#44369=CARTESIAN_POINT('Ctrl Pts',(367.68739519582,-20.3489232736698,-2.36195580540828));
#44370=CARTESIAN_POINT('Ctrl Pts',(367.759767984918,-20.3547757584027,-2.45267855767936));
#44371=CARTESIAN_POINT('Ctrl Pts',(367.832147409629,-20.3606287797299,-2.54340962800885));
#44372=CARTESIAN_POINT('Ctrl Pts',(367.908538106326,-20.3664818010571,-2.63092357375398));
#44373=CARTESIAN_POINT('Ctrl Pts',(367.988613103915,-20.3723348223843,-2.71485791152273));
#44374=CARTESIAN_POINT('Ctrl Pts',(368.068714808062,-20.3781897958071,-2.79882024301425));
#44375=CARTESIAN_POINT('Ctrl Pts',(368.152502971456,-20.3840447692299,-2.87920029380748));
#44376=CARTESIAN_POINT('Ctrl Pts',(368.23961411925,-20.3898997426528,-2.95567277162098));
#44377=CARTESIAN_POINT('Ctrl Pts',(368.326823996341,-20.395761351936,-3.03223192116581));
#44378=CARTESIAN_POINT('Ctrl Pts',(368.417364064238,-20.4016229612192,-3.10487438553329));
#44379=CARTESIAN_POINT('Ctrl Pts',(368.510838085076,-20.4074845705024,-3.17331542192186));
#44380=CARTESIAN_POINT('Ctrl Pts',(368.604375136133,-20.4133501323118,-3.24180260860396));
#44381=CARTESIAN_POINT('Ctrl Pts',(368.700849736569,-20.4192156941212,-3.30608249755406));
#44382=CARTESIAN_POINT('Ctrl Pts',(368.799838500068,-20.4250812559306,-3.36591484764299));
#44383=CARTESIAN_POINT('Ctrl Pts',(368.898972009419,-20.43095539463,-3.42583468730284));
#44384=CARTESIAN_POINT('Ctrl Pts',(369.000626657562,-20.4368295333294,-3.48129381185933));
#44385=CARTESIAN_POINT('Ctrl Pts',(369.104356372638,-20.4427036720288,-3.53209884851597));
#44386=CARTESIAN_POINT('Ctrl Pts',(369.130587924348,-20.4441891458194,-3.54494661297028));
#44387=CARTESIAN_POINT('Ctrl Pts',(369.156952089498,-20.4456746196099,-3.55749699290705));
#44388=CARTESIAN_POINT('Ctrl Pts',(369.183441489458,-20.4471600934005,-3.56974736242766));
#44389=CARTESIAN_POINT('Ctrl Pts',(369.288182824173,-20.4530337827909,-3.61818636279223));
#44390=CARTESIAN_POINT('Ctrl Pts',(369.395232312874,-20.4589074721814,-3.66209224755502));
#44391=CARTESIAN_POINT('Ctrl Pts',(369.504160503663,-20.4647811615719,-3.701239039215));
#44392=CARTESIAN_POINT('Ctrl Pts',(369.612948057924,-20.4706472674776,-3.74033528868918));
#44393=CARTESIAN_POINT('Ctrl Pts',(369.723609105338,-20.4765133733832,-3.77468452587851));
#44394=CARTESIAN_POINT('Ctrl Pts',(369.835691557586,-20.4823794792889,-3.80410758544755));
#44395=CARTESIAN_POINT('Ctrl Pts',(369.947659238829,-20.4882395783768,-3.83350051617837));
#44396=CARTESIAN_POINT('Ctrl Pts',(370.061045032564,-20.4940996774647,-3.85797719862751));
#44397=CARTESIAN_POINT('Ctrl Pts',(370.175379549363,-20.4999597765527,-3.87740755037494));
#44398=CARTESIAN_POINT('Ctrl Pts',(370.293838994691,-20.5060312946468,-3.89753890488617));
#44399=CARTESIAN_POINT('Ctrl Pts',(370.413316486025,-20.512102812741,-3.91225278098042));
#44400=CARTESIAN_POINT('Ctrl Pts',(370.533275511409,-20.5181743308351,-3.92146178209539));
#44401=CARTESIAN_POINT('Ctrl Pts',(370.64892431314,-20.5240276944317,-3.93033989644041));
#44402=CARTESIAN_POINT('Ctrl Pts',(370.765020193394,-20.5298810580284,-3.93410188256667));
#44403=CARTESIAN_POINT('Ctrl Pts',(370.881075715139,-20.535734421625,-3.9327220474309));
#44404=CARTESIAN_POINT('Ctrl Pts',(370.997113811538,-20.5415869063588,-3.93134241947274));
#44405=CARTESIAN_POINT('Ctrl Pts',(371.113111148472,-20.5474393910926,-3.92482251024291));
#44406=CARTESIAN_POINT('Ctrl Pts',(371.228580166447,-20.5532918758263,-3.91318875450339));
#44407=CARTESIAN_POINT('Ctrl Pts',(371.344059771381,-20.5591448971544,-3.90155393210469));
#44408=CARTESIAN_POINT('Ctrl Pts',(371.459010549976,-20.5649979184824,-3.88480437254234));
#44409=CARTESIAN_POINT('Ctrl Pts',(371.572950650453,-20.5708509398104,-3.86301832649777));
#44410=CARTESIAN_POINT('Ctrl Pts',(371.686928752154,-20.5767059132341,-3.84122501438613));
#44411=CARTESIAN_POINT('Ctrl Pts',(371.799895099893,-20.5825608866578,-3.81439195320187));
#44412=CARTESIAN_POINT('Ctrl Pts',(371.911379304842,-20.5884158600815,-3.7826482296718));
#44413=CARTESIAN_POINT('Ctrl Pts',(372.022989862817,-20.5942774693655,-3.75086852870852));
#44414=CARTESIAN_POINT('Ctrl Pts',(372.133114527611,-20.6001390786495,-3.71416716999102));
#44415=CARTESIAN_POINT('Ctrl Pts',(372.241299223299,-20.6060006879335,-3.67272275352536));
#44416=CARTESIAN_POINT('Ctrl Pts',(372.349556868721,-20.6118662497437,-3.63125039078536));
#44417=CARTESIAN_POINT('Ctrl Pts',(372.455871562301,-20.6177318115538,-3.58502876613249));
#44418=CARTESIAN_POINT('Ctrl Pts',(372.559811905784,-20.623597373364,-3.53428341741013));
#44419=CARTESIAN_POINT('Ctrl Pts',(372.663904235542,-20.6294715120642,-3.48346386654189));
#44420=CARTESIAN_POINT('Ctrl Pts',(372.765614924711,-20.6353456507643,-3.42810758687781));
#44421=CARTESIAN_POINT('Ctrl Pts',(372.864539660816,-20.6412197894645,-3.36848458686931));
#44422=CARTESIAN_POINT('Ctrl Pts',(372.889556111642,-20.6427052632471,-3.35340690350608));
#44423=CARTESIAN_POINT('Ctrl Pts',(372.914394558932,-20.6441907370297,-3.33805656905684));
#44424=CARTESIAN_POINT('Ctrl Pts',(372.9390487961,-20.6456762108123,-3.32243836031613));
#44425=CARTESIAN_POINT('Ctrl Pts',(373.036533742045,-20.6515499002076,-3.26068263757789));
#44426=CARTESIAN_POINT('Ctrl Pts',(373.1314607476,-20.6574235896028,-3.19452990984376));
#44427=CARTESIAN_POINT('Ctrl Pts',(373.223407112138,-20.6632972789981,-3.12421854436298));
#44428=CARTESIAN_POINT('Ctrl Pts',(373.315234765282,-20.6691633849086,-3.05399795746024));
#44429=CARTESIAN_POINT('Ctrl Pts',(373.404089105203,-20.675029490819,-2.97962965904482));
#44430=CARTESIAN_POINT('Ctrl Pts',(373.489574496485,-20.6808955967295,-2.90139641524899));
#44431=CARTESIAN_POINT('Ctrl Pts',(373.574972351815,-20.6867556958223,-2.82324328129798));
#44432=CARTESIAN_POINT('Ctrl Pts',(373.657007817398,-20.692615794915,-2.74123335133565));
#44433=CARTESIAN_POINT('Ctrl Pts',(373.735317123481,-20.6984758940078,-2.65569053806536));
#44434=CARTESIAN_POINT('Ctrl Pts',(373.816451650586,-20.7045474121001,-2.56706153534387));
#44435=CARTESIAN_POINT('Ctrl Pts',(373.893585720489,-20.7106189301924,-2.47464019400463));
#44436=CARTESIAN_POINT('Ctrl Pts',(373.96635504494,-20.7166904482848,-2.37882997074371));
#44437=CARTESIAN_POINT('Ctrl Pts',(374.036509709485,-20.7225438118862,-2.28646228527293));
#44438=CARTESIAN_POINT('Ctrl Pts',(374.102607616852,-20.7283971754877,-2.19094541444005));
#44439=CARTESIAN_POINT('Ctrl Pts',(374.164362932726,-20.7342505390892,-2.092675026966));
#44440=CARTESIAN_POINT('Ctrl Pts',(374.226108976246,-20.7401030238278,-1.99441939446011));
#44441=CARTESIAN_POINT('Ctrl Pts',(374.283513504976,-20.7459555085664,-1.89341141708286));
#44442=CARTESIAN_POINT('Ctrl Pts',(374.336334421615,-20.751807993305,-1.79007512543936));
#44443=CARTESIAN_POINT('Ctrl Pts',(374.389160181222,-20.7576610146378,-1.68672935924563));
#44444=CARTESIAN_POINT('Ctrl Pts',(374.437401305259,-20.7635140359707,-1.58105522230921));
#44445=CARTESIAN_POINT('Ctrl Pts',(374.480862331955,-20.7693670573035,-1.47350003890016));
#44446=CARTESIAN_POINT('Ctrl Pts',(374.524337853742,-20.775222030732,-1.36590898376075));
#44447=CARTESIAN_POINT('Ctrl Pts',(374.563029953382,-20.7810770041605,-1.25643601750802));
#44448=CARTESIAN_POINT('Ctrl Pts',(374.596792101207,-20.786931977589,-1.14554639070893));
#44449=CARTESIAN_POINT('Ctrl Pts',(374.630592514089,-20.7927935868778,-1.03453108476222));
#44450=CARTESIAN_POINT('Ctrl Pts',(374.659451702506,-20.7986551961665,-0.922096309035752));
#44451=CARTESIAN_POINT('Ctrl Pts',(374.683273586565,-20.8045168054553,-0.808720447855802));
#44452=CARTESIAN_POINT('Ctrl Pts',(374.707111533896,-20.8103823672702,-0.695268136500583));
#44453=CARTESIAN_POINT('Ctrl Pts',(374.725905346492,-20.8162479290851,-0.580873882771531));
#44454=CARTESIAN_POINT('Ctrl Pts',(374.739610680474,-20.8221134909,-0.46602246021866));
#44455=CARTESIAN_POINT('Ctrl Pts',(374.753336055016,-20.8279876296049,-0.351003096718436));
#44456=CARTESIAN_POINT('Ctrl Pts',(374.761958070728,-20.8338617683097,-0.235525640664858));
#44457=CARTESIAN_POINT('Ctrl Pts',(374.765484436191,-20.8397359070146,-0.120076213154389));
#44458=CARTESIAN_POINT('Ctrl Pts',(374.76637619642,-20.841221380751,-0.0908809385667788));
#44459=CARTESIAN_POINT('Ctrl Pts',(374.766942348414,-20.8427068544874,-0.0616874349996441));
#44460=CARTESIAN_POINT('Ctrl Pts',(374.767183541498,-20.8441923282239,-0.0325035074423659));
#44461=CARTESIAN_POINT('Ctrl Pts',(374.76813723945,-20.8500660176043,0.0828922219920092));
#44462=CARTESIAN_POINT('Ctrl Pts',(374.76400941581,-20.8559397069847,0.198522152277014));
#44463=CARTESIAN_POINT('Ctrl Pts',(374.754771222418,-20.8618133963651,0.313901863608043));
#44464=CARTESIAN_POINT('Ctrl Pts',(374.745544956401,-20.8676795022607,0.429132608892232));
#44465=CARTESIAN_POINT('Ctrl Pts',(374.731221474499,-20.8735456081563,0.544113369609628));
#44466=CARTESIAN_POINT('Ctrl Pts',(374.711823909588,-20.8794117140519,0.65835840000756));
#44467=CARTESIAN_POINT('Ctrl Pts',(374.692446207536,-20.8852718131298,0.77248644495004));
#44468=CARTESIAN_POINT('Ctrl Pts',(374.668004826092,-20.8911319122077,0.885879853210644));
#44469=CARTESIAN_POINT('Ctrl Pts',(374.638574748598,-20.8969920112856,0.998057350056903));
#44470=CARTESIAN_POINT('Ctrl Pts',(374.608082900976,-20.9030635293835,1.11428195534522));
#44471=CARTESIAN_POINT('Ctrl Pts',(374.572235635544,-20.9091350474815,1.22920080788944));
#44472=CARTESIAN_POINT('Ctrl Pts',(374.531174496003,-20.9152065655794,1.34228907569993));
#44473=CARTESIAN_POINT('Ctrl Pts',(374.491588716113,-20.9210599291661,1.45131399141539));
#44474=CARTESIAN_POINT('Ctrl Pts',(374.447157444423,-20.9269132927529,1.55863718558821));
#44475=CARTESIAN_POINT('Ctrl Pts',(374.39805821096,-20.9327666563396,1.66380397362335));
#44476=CARTESIAN_POINT('Ctrl Pts',(374.348966349581,-20.9386191410636,1.76895497122027));
#44477=CARTESIAN_POINT('Ctrl Pts',(374.295208094768,-20.9444716257875,1.87194983221472));
#44478=CARTESIAN_POINT('Ctrl Pts',(374.237008519516,-20.9503241105115,1.9723552493226));
#44479=CARTESIAN_POINT('Ctrl Pts',(374.178803608143,-20.9561771318298,2.07276987226034));
#44480=CARTESIAN_POINT('Ctrl Pts',(374.116156774036,-20.9620301531481,2.17059422189032));
#44481=CARTESIAN_POINT('Ctrl Pts',(374.049337945602,-20.9678831744664,2.2654215514133));
#44482=CARTESIAN_POINT('Ctrl Pts',(373.982496831797,-20.9737381478804,2.36028050768339));
#44483=CARTESIAN_POINT('Ctrl Pts',(373.911481194693,-20.9795931212944,2.45214011871587));
#44484=CARTESIAN_POINT('Ctrl Pts',(373.836602552863,-20.9854480947085,2.54062503772484));
#44485=CARTESIAN_POINT('Ctrl Pts',(373.761639045708,-20.991309703983,2.62921024302679));
#44486=CARTESIAN_POINT('Ctrl Pts',(373.682804062196,-20.9971713132576,2.7144128067209));
#44487=CARTESIAN_POINT('Ctrl Pts',(373.600447506606,-21.0030329225321,2.79589265542889));
#44488=CARTESIAN_POINT('Ctrl Pts',(373.518035417384,-21.0088984843329,2.87742744659855));
#44489=CARTESIAN_POINT('Ctrl Pts',(373.432097333195,-21.0147640461337,2.9552342477066));
#44490=CARTESIAN_POINT('Ctrl Pts',(373.343016573817,-21.0206296079345,3.02901299589426));
#44491=CARTESIAN_POINT('Ctrl Pts',(373.253805556517,-21.0265037466255,3.10289962670991));
#44492=CARTESIAN_POINT('Ctrl Pts',(373.161443021103,-21.0323778853165,3.1727462014037));
#44493=CARTESIAN_POINT('Ctrl Pts',(373.066341637842,-21.0382520240075,3.23829566668944));
#44494=CARTESIAN_POINT('Ctrl Pts',(373.042292048985,-21.0397374978835,3.25487205744056));
#44495=CARTESIAN_POINT('Ctrl Pts',(373.018067432976,-21.0412229717596,3.27117387689709));
#44496=CARTESIAN_POINT('Ctrl Pts',(372.993674700417,-21.0427084456356,3.28719743953415));
#44497=CARTESIAN_POINT('Ctrl Pts',(372.897223771986,-21.0485821350287,3.35055596197067));
#44498=CARTESIAN_POINT('Ctrl Pts',(372.797821301549,-21.0544558244219,3.40977140443017));
#44499=CARTESIAN_POINT('Ctrl Pts',(372.695858712007,-21.0603295138151,3.46455691699246));
#44500=CARTESIAN_POINT('Ctrl Pts',(372.59402776575,-21.0661956197233,3.51927169631031));
#44501=CARTESIAN_POINT('Ctrl Pts',(372.489643634267,-21.0720617256316,3.56956772609213));
#44502=CARTESIAN_POINT('Ctrl Pts',(372.38312703408,-21.0779278315399,3.61520111768275));
#44503=CARTESIAN_POINT('Ctrl Pts',(372.276719505538,-21.0837879306303,3.660787781261));
#44504=CARTESIAN_POINT('Ctrl Pts',(372.168184229198,-21.0896480297208,3.70172114175997));
#44505=CARTESIAN_POINT('Ctrl Pts',(372.057966273182,-21.0955081288112,3.73780330466084));
#44506=CARTESIAN_POINT('Ctrl Pts',(371.943771904825,-21.1015796469044,3.77518722966137));
#44507=CARTESIAN_POINT('Ctrl Pts',(371.827771547821,-21.1076511649975,3.80736309407919));
#44508=CARTESIAN_POINT('Ctrl Pts',(371.710482954793,-21.1137226830907,3.83416532178671));
#44509=CARTESIAN_POINT('Ctrl Pts',(371.597408634589,-21.1195760466896,3.86000452404651));
#44510=CARTESIAN_POINT('Ctrl Pts',(371.483137497155,-21.1254294102886,3.88084950207157));
#44511=CARTESIAN_POINT('Ctrl Pts',(371.368147858245,-21.1312827738875,3.89660294689349));
#44512=CARTESIAN_POINT('Ctrl Pts',(371.253175484644,-21.1371352586235,3.91235402638843));
#44513=CARTESIAN_POINT('Ctrl Pts',(371.137485233285,-21.1429877433595,3.92301503668544));
#44514=CARTESIAN_POINT('Ctrl Pts',(371.021563229891,-21.1488402280955,3.92854020838743));
#44515=CARTESIAN_POINT('Ctrl Pts',(370.905630598008,-21.1546932494256,3.93406588667338));
#44516=CARTESIAN_POINT('Ctrl Pts',(370.789466584549,-21.1605462707558,3.93445477061387));
#44517=CARTESIAN_POINT('Ctrl Pts',(370.673559312802,-21.166399292086,3.92971318185962));
#44518=CARTESIAN_POINT('Ctrl Pts',(370.557613383742,-21.1722542655117,3.92497001169402));
#44519=CARTESIAN_POINT('Ctrl Pts',(370.441924779238,-21.1781092389374,3.91509298324243));
#44520=CARTESIAN_POINT('Ctrl Pts',(370.326977783324,-21.1839642123631,3.90014038894418));
#44521=CARTESIAN_POINT('Ctrl Pts',(370.211900509757,-21.189825821649,3.88517084780129));
#44522=CARTESIAN_POINT('Ctrl Pts',(370.097566932325,-21.1956874309349,3.86511431248825));
#44523=CARTESIAN_POINT('Ctrl Pts',(369.984452503796,-21.2015490402208,3.8400804533032));
#44524=CARTESIAN_POINT('Ctrl Pts',(369.871261801379,-21.2074146020328,3.81502971360342));
#44525=CARTESIAN_POINT('Ctrl Pts',(369.759292282861,-21.2132801638448,3.78499507377435));
#44526=CARTESIAN_POINT('Ctrl Pts',(369.649003894717,-21.2191457256568,3.75013597350411));
#44527=CARTESIAN_POINT('Ctrl Pts',(369.538554237903,-21.2250198643587,3.71522590068036));
#44528=CARTESIAN_POINT('Ctrl Pts',(369.429791004014,-21.2308940030605,3.67547742958702));
#44529=CARTESIAN_POINT('Ctrl Pts',(369.323153909422,-21.2367681417624,3.63109797925539));
#44530=CARTESIAN_POINT('Ctrl Pts',(369.296187129427,-21.238253615524,3.61987514091798));
#44531=CARTESIAN_POINT('Ctrl Pts',(369.269356189941,-21.2397390892856,3.60835637822619));
#44532=CARTESIAN_POINT('Ctrl Pts',(369.242667934241,-21.2412245630472,3.59654550025453));
#44533=CARTESIAN_POINT('Ctrl Pts',(369.137140304322,-21.2470982524757,3.54984428554753));
#44534=CARTESIAN_POINT('Ctrl Pts',(369.033494078067,-21.2529719419041,3.49841686381802));
#44535=CARTESIAN_POINT('Ctrl Pts',(368.932182491796,-21.2588456313325,3.44243664673818));
#44536=CARTESIAN_POINT('Ctrl Pts',(368.831001708298,-21.2647117372763,3.38652870537574));
#44537=CARTESIAN_POINT('Ctrl Pts',(368.73214992876,-21.2705778432201,3.3260798562357));
#44538=CARTESIAN_POINT('Ctrl Pts',(368.636060169164,-21.2764439491639,3.26131141635881));
#44539=CARTESIAN_POINT('Ctrl Pts',(368.540068804256,-21.28230404829,3.19660929853768));
#44540=CARTESIAN_POINT('Ctrl Pts',(368.446834174171,-21.2881641474162,3.12759661764776));
#44541=CARTESIAN_POINT('Ctrl Pts',(368.35676384689,-21.2940242465424,3.05454008742687));
#44542=CARTESIAN_POINT('Ctrl Pts',(368.26344398851,-21.3000957646222,2.97884784493437));
#44543=CARTESIAN_POINT('Ctrl Pts',(368.173521460681,-21.3061672827021,2.89881467686665));
#44544=CARTESIAN_POINT('Ctrl Pts',(368.087416076936,-21.3122388007819,2.81478589442049));
#44545=CARTESIAN_POINT('Ctrl Pts',(368.004404527708,-21.3180921644168,2.73377633256362));
#44546=CARTESIAN_POINT('Ctrl Pts',(367.924940858342,-21.3239455280518,2.64905365930629));
#44547=CARTESIAN_POINT('Ctrl Pts',(367.849366137848,-21.3297988916867,2.56096705501532));
#44548=CARTESIAN_POINT('Ctrl Pts',(367.773802764645,-21.3356513764586,2.4728936766323));
#44549=CARTESIAN_POINT('Ctrl Pts',(367.702127448222,-21.3415038612306,2.38145768498256));
#44550=CARTESIAN_POINT('Ctrl Pts',(367.634642182345,-21.3473563460026,2.28704276330556));
#44551=CARTESIAN_POINT('Ctrl Pts',(367.567150728977,-21.3532093673688,2.19261918504946));
#44552=CARTESIAN_POINT('Ctrl Pts',(367.503850330107,-21.359062388735,2.0952164699443));
#44553=CARTESIAN_POINT('Ctrl Pts',(367.445000289882,-21.3649154101012,1.9952482188496));
#44554=CARTESIAN_POINT('Ctrl Pts',(367.386130622034,-21.3707703835628,1.89524662641543));
#44555=CARTESIAN_POINT('Ctrl Pts',(367.331714473735,-21.3766253570245,1.79267815239974));
#44556=CARTESIAN_POINT('Ctrl Pts',(367.281965396373,-21.3824803304862,1.68798134536636));
#44557=CARTESIAN_POINT('Ctrl Pts',(367.232159934826,-21.3883419398078,1.58316587795775));
#44558=CARTESIAN_POINT('Ctrl Pts',(367.187032279204,-21.3942035491294,1.47621763630986));
#44559=CARTESIAN_POINT('Ctrl Pts',(367.146748020166,-21.400065158451,1.36759560043083));
#44560=CARTESIAN_POINT('Ctrl Pts',(367.106436597157,-21.4059307202986,1.25890031991917));
#44561=CARTESIAN_POINT('Ctrl Pts',(367.070975200002,-21.4117962821462,1.14852939014845));
#44562=CARTESIAN_POINT('Ctrl Pts',(367.040479191642,-21.4176618439938,1.03695574152691));
#44563=CARTESIAN_POINT('Ctrl Pts',(367.009938590641,-21.4235359827309,0.925218944877583));
#44564=CARTESIAN_POINT('Ctrl Pts',(366.984377959642,-21.4294101214679,0.812276320919939));
#44565=CARTESIAN_POINT('Ctrl Pts',(366.963861377235,-21.4352842602049,0.698609810606347));
#44566=CARTESIAN_POINT('Ctrl Pts',(366.958673069781,-21.4367697336229,0.669865412977412));
#44567=CARTESIAN_POINT('Ctrl Pts',(366.953807070168,-21.4382552070409,0.641074739808697));
#44568=CARTESIAN_POINT('Ctrl Pts',(366.949263887404,-21.4397406804589,0.612245606489808));
#44569=CARTESIAN_POINT('Ctrl Pts',(366.919679988603,-21.4494136558938,0.424518586249826));
#44570=CARTESIAN_POINT('Ctrl Pts',(366.903697510534,-21.4590866313286,0.234593952454445));
#44571=CARTESIAN_POINT('Ctrl Pts',(366.901564247857,-21.4687596067635,0.0440236239979143));
#44572=CARTESIAN_POINT('Ctrl Pts',(366.901411571228,-21.469451897164,0.0303845932875485));
#44573=CARTESIAN_POINT('Ctrl Pts',(366.901329818244,-21.4701441875646,0.0167422730070523));
#44574=CARTESIAN_POINT('Ctrl Pts',(366.901319072765,-21.4708364779651,0.00309724153850734));
#44575=CARTESIAN_POINT('',(366.901317979184,-22.7208364779192,0.000995388470130986));
#44576=CARTESIAN_POINT('Ctrl Pts',(366.901319072764,-21.4708364780021,0.00309724080919957));
#44577=CARTESIAN_POINT('Ctrl Pts',(366.901229367429,-21.4766158530609,-0.110814138701328));
#44578=CARTESIAN_POINT('Ctrl Pts',(366.906092658234,-21.4823952281197,-0.224907569796787));
#44579=CARTESIAN_POINT('Ctrl Pts',(366.91592978844,-21.4881746031785,-0.338709276167276));
#44580=CARTESIAN_POINT('Ctrl Pts',(366.925756862887,-21.4939480704164,-0.452394651602257));
#44581=CARTESIAN_POINT('Ctrl Pts',(366.94054763356,-21.4997215376542,-0.565788472930522));
#44582=CARTESIAN_POINT('Ctrl Pts',(366.960270897962,-21.5054950048921,-0.678416677585149));
#44583=CARTESIAN_POINT('Ctrl Pts',(366.979980182921,-21.5112643800155,-0.790965053693971));
#44584=CARTESIAN_POINT('Ctrl Pts',(367.004614938388,-21.517033755139,-0.902748473242205));
#44585=CARTESIAN_POINT('Ctrl Pts',(367.034092188521,-21.5228031302625,-1.01329852330451));
#44586=CARTESIAN_POINT('Ctrl Pts',(367.063558679286,-21.5285703995306,-1.12380822195673));
#44587=CARTESIAN_POINT('Ctrl Pts',(367.097864043444,-21.5343376687986,-1.23308503391867));
#44588=CARTESIAN_POINT('Ctrl Pts',(367.136874475267,-21.5401049380667,-1.34067202059475));
#44589=CARTESIAN_POINT('Ctrl Pts',(367.175880754778,-21.5458715934604,-1.44824755559515));
#44590=CARTESIAN_POINT('Ctrl Pts',(367.219590960946,-21.551638248854,-1.55413322193989));
#44591=CARTESIAN_POINT('Ctrl Pts',(367.267822107052,-21.5574049042477,-1.65788934870166));
#44592=CARTESIAN_POINT('Ctrl Pts',(367.316060590951,-21.563172436969,-1.76166126071782));
#44593=CARTESIAN_POINT('Ctrl Pts',(367.368821200754,-21.5689399696904,-1.86330260306287));
#44594=CARTESIAN_POINT('Ctrl Pts',(367.425874093819,-21.5747075024117,-1.96239652949444));
#44595=CARTESIAN_POINT('Ctrl Pts',(367.482984649202,-21.5804808642732,-2.0615906083499));
#44596=CARTESIAN_POINT('Ctrl Pts',(367.544395935419,-21.5862542261347,-2.15823176110984));
#44597=CARTESIAN_POINT('Ctrl Pts',(367.60983371631,-21.5920275879961,-2.25193051642203));
#44598=CARTESIAN_POINT('Ctrl Pts',(367.675306973377,-21.5978040798048,-2.34568006920018));
#44599=CARTESIAN_POINT('Ctrl Pts',(367.744810810353,-21.6035805716134,-2.43648371170479));
#44600=CARTESIAN_POINT('Ctrl Pts',(367.818030698075,-21.609357063422,-2.52398510250822));
#44601=CARTESIAN_POINT('Ctrl Pts',(367.891364596513,-21.6151425498083,-2.61162274176244));
#44602=CARTESIAN_POINT('Ctrl Pts',(367.968425810692,-21.6209280361947,-2.69594754916856));
#44603=CARTESIAN_POINT('Ctrl Pts',(368.048862868866,-21.626713522581,-2.7766399712806));
#44604=CARTESIAN_POINT('Ctrl Pts',(368.102359212646,-21.6305612810109,-2.83030615017597));
#44605=CARTESIAN_POINT('Ctrl Pts',(368.157348031264,-21.6344090394407,-2.88236645748791));
#44606=CARTESIAN_POINT('Ctrl Pts',(368.213718362491,-21.6382567978706,-2.93273717014811));
#44607=CARTESIAN_POINT('Ctrl Pts',(368.299768935969,-21.6441304873147,-3.00962919147517));
#44608=CARTESIAN_POINT('Ctrl Pts',(368.389349871925,-21.6500041767589,-3.08285880193323));
#44609=CARTESIAN_POINT('Ctrl Pts',(368.482116339173,-21.6558778662031,-3.15208455427479));
#44610=CARTESIAN_POINT('Ctrl Pts',(368.574763036186,-21.6617439721618,-3.22122092965851));
#44611=CARTESIAN_POINT('Ctrl Pts',(368.67058675735,-21.6676100781204,-3.28636348225071));
#44612=CARTESIAN_POINT('Ctrl Pts',(368.769207361484,-21.673476184079,-3.34720893535269));
#44613=CARTESIAN_POINT('Ctrl Pts',(368.867726979363,-21.6793362832191,-3.407992083478));
#44614=CARTESIAN_POINT('Ctrl Pts',(368.969037434012,-21.6851963823593,-3.4644866687855));
#44615=CARTESIAN_POINT('Ctrl Pts',(369.072727714875,-21.6910564814994,-3.51643131377137));
#44616=CARTESIAN_POINT('Ctrl Pts',(369.180158903211,-21.6971279995736,-3.57025000238972));
#44617=CARTESIAN_POINT('Ctrl Pts',(369.290144515212,-21.7031995176479,-3.61918397922799));
#44618=CARTESIAN_POINT('Ctrl Pts',(369.402196883889,-21.7092710357222,-3.6629931107211));
#44619=CARTESIAN_POINT('Ctrl Pts',(369.51022312268,-21.7151243993687,-3.70522814560526));
#44620=CARTESIAN_POINT('Ctrl Pts',(369.620169735998,-21.7209777630153,-3.74270011324703));
#44621=CARTESIAN_POINT('Ctrl Pts',(369.731577992946,-21.7268311266618,-3.77524221746824));
#44622=CARTESIAN_POINT('Ctrl Pts',(369.842969522302,-21.7326836114445,-3.8077794355969));
#44623=CARTESIAN_POINT('Ctrl Pts',(369.955821862452,-21.7385360962273,-3.8353881462999));
#44624=CARTESIAN_POINT('Ctrl Pts',(370.069660955866,-21.74438858101,-3.85795137726262));
#44625=CARTESIAN_POINT('Ctrl Pts',(370.183510486777,-21.750241602386,-3.88051667696689));
#44626=CARTESIAN_POINT('Ctrl Pts',(370.298346545519,-21.7560946237621,-3.8980354969932));
#44627=CARTESIAN_POINT('Ctrl Pts',(370.413685415421,-21.7619476451381,-3.91044209166534));
#44628=CARTESIAN_POINT('Ctrl Pts',(370.529062753043,-21.7678026186088,-3.92285282417418));
#44629=CARTESIAN_POINT('Ctrl Pts',(370.644942824728,-21.7736575920794,-3.93014789680097));
#44630=CARTESIAN_POINT('Ctrl Pts',(370.760838045376,-21.7795125655501,-3.9323135324944));
#44631=CARTESIAN_POINT('Ctrl Pts',(370.876864618334,-21.7853741748793,-3.93448162265705));
#44632=CARTESIAN_POINT('Ctrl Pts',(370.992905961218,-21.7912357842085,-3.93150866465491));
#44633=CARTESIAN_POINT('Ctrl Pts',(371.108475645362,-21.7970973935378,-3.92343299993893));
#44634=CARTESIAN_POINT('Ctrl Pts',(371.224123258974,-21.8029629553922,-3.91535188974429));
#44635=CARTESIAN_POINT('Ctrl Pts',(371.339298171105,-21.8088285172467,-3.90216126834873));
#44636=CARTESIAN_POINT('Ctrl Pts',(371.45352194879,-21.8146940791011,-3.88395098939656));
#44637=CARTESIAN_POINT('Ctrl Pts',(371.567912749618,-21.8205682178438,-3.86571408255577));
#44638=CARTESIAN_POINT('Ctrl Pts',(371.681349237169,-21.8264423565866,-3.84244295213261));
#44639=CARTESIAN_POINT('Ctrl Pts',(371.793365910351,-21.8323164953293,-3.81427789025932));
#44640=CARTESIAN_POINT('Ctrl Pts',(371.821693089267,-21.8338019686469,-3.8071554081841));
#44641=CARTESIAN_POINT('Ctrl Pts',(371.849929562381,-21.8352874419645,-3.79972020227114));
#44642=CARTESIAN_POINT('Ctrl Pts',(371.878067999437,-21.8367729152822,-3.7919750305456));
#44643=CARTESIAN_POINT('Ctrl Pts',(371.989329807703,-21.8426466049661,-3.76134995318875));
#44644=CARTESIAN_POINT('Ctrl Pts',(372.099427906212,-21.8485202946499,-3.72577285636308));
#44645=CARTESIAN_POINT('Ctrl Pts',(372.207888437869,-21.8543939843338,-3.68534840266124));
#44646=CARTESIAN_POINT('Ctrl Pts',(372.316208936825,-21.8602600905344,-3.64497614071385));
#44647=CARTESIAN_POINT('Ctrl Pts',(372.422895689887,-21.8661261967349,-3.59976911074903));
#44648=CARTESIAN_POINT('Ctrl Pts',(372.527487773092,-21.8719923029355,-3.54988233924066));
#44649=CARTESIAN_POINT('Ctrl Pts',(372.631972755362,-21.8778524023195,-3.50004665113853));
#44650=CARTESIAN_POINT('Ctrl Pts',(372.734366963505,-21.8837125017035,-3.44554092997041));
#44651=CARTESIAN_POINT('Ctrl Pts',(372.834227947198,-21.8895726010875,-3.38656885593958));
#44652=CARTESIAN_POINT('Ctrl Pts',(372.937691680256,-21.8956441190711,-3.32546920821231));
#44653=CARTESIAN_POINT('Ctrl Pts',(373.038435529005,-21.9017156370547,-3.25957500974351));
#44654=CARTESIAN_POINT('Ctrl Pts',(373.135993338471,-21.9077871550383,-3.18916587223289));
#44655=CARTESIAN_POINT('Ctrl Pts',(373.230045824359,-21.9136405189319,-3.12128658662391));
#44656=CARTESIAN_POINT('Ctrl Pts',(373.321136920447,-21.9194938828256,-3.04921149089762));
#44657=CARTESIAN_POINT('Ctrl Pts',(373.408877784197,-21.9253472467192,-2.97323563846321));
#44658=CARTESIAN_POINT('Ctrl Pts',(373.49660547395,-21.9311997317499,-2.89727119354882));
#44659=CARTESIAN_POINT('Ctrl Pts',(373.580983619329,-21.9370522167806,-2.81740742686313));
#44660=CARTESIAN_POINT('Ctrl Pts',(373.661656936468,-21.9429047018112,-2.73397928089499));
#44661=CARTESIAN_POINT('Ctrl Pts',(373.742337650259,-21.9487577234357,-2.6505434856929));
#44662=CARTESIAN_POINT('Ctrl Pts',(373.819312573345,-21.9546107450602,-2.56354295856598));
#44663=CARTESIAN_POINT('Ctrl Pts',(373.892264231691,-21.9604637666847,-2.47334852910365));
#44664=CARTESIAN_POINT('Ctrl Pts',(373.965240220813,-21.966318740404,-2.3831240180712));
#44665=CARTESIAN_POINT('Ctrl Pts',(374.034190017342,-21.9721737141233,-2.28970380759661));
#44666=CARTESIAN_POINT('Ctrl Pts',(374.098837719774,-21.9780286878426,-2.19349015062801));
#44667=CARTESIAN_POINT('Ctrl Pts',(374.16355869204,-21.9838902974196,-2.09716744788689));
#44668=CARTESIAN_POINT('Ctrl Pts',(374.223967607723,-21.9897519069966,-1.99804532259946));
#44669=CARTESIAN_POINT('Ctrl Pts',(374.279832987824,-21.9956135165736,-1.8965533098875));
#44670=CARTESIAN_POINT('Ctrl Pts',(374.335736038347,-22.0014790786755,-1.79499286038996));
#44671=CARTESIAN_POINT('Ctrl Pts',(374.387089270144,-22.0073446407775,-1.69105971091343));
#44672=CARTESIAN_POINT('Ctrl Pts',(374.43370882486,-22.0132102028795,-1.58520460297973));
#44673=CARTESIAN_POINT('Ctrl Pts',(374.480396548763,-22.0190843418675,-1.47919470899576));
#44674=CARTESIAN_POINT('Ctrl Pts',(374.522336632368,-22.0249584808554,-1.37125763137149));
#44675=CARTESIAN_POINT('Ctrl Pts',(374.559394611669,-22.0308326198434,-1.26186058805801));
#44676=CARTESIAN_POINT('Ctrl Pts',(374.568765951338,-22.0323180907935,-1.23419591580405));
#44677=CARTESIAN_POINT('Ctrl Pts',(374.577825335228,-22.0338035617437,-1.20643793408156));
#44678=CARTESIAN_POINT('Ctrl Pts',(374.586571107134,-22.0352890326939,-1.17859429767826));
#44679=CARTESIAN_POINT('Ctrl Pts',(374.621152692097,-22.0411627211946,-1.06849800333977));
#44680=CARTESIAN_POINT('Ctrl Pts',(374.650942200166,-22.0470364096953,-0.956695046797344));
#44681=CARTESIAN_POINT('Ctrl Pts',(374.675770697657,-22.052910098196,-0.843640352283101));
#44682=CARTESIAN_POINT('Ctrl Pts',(374.700567139219,-22.0587762032118,-0.730731622025469));
#44683=CARTESIAN_POINT('Ctrl Pts',(374.720415220098,-22.0646423082276,-0.616574767554941));
#44684=CARTESIAN_POINT('Ctrl Pts',(374.735195338943,-22.0705084132434,-0.501641148042162));
#44685=CARTESIAN_POINT('Ctrl Pts',(374.749960323135,-22.0763685114423,-0.386825219091741));
#44686=CARTESIAN_POINT('Ctrl Pts',(374.759667615314,-22.0822286096413,-0.271234514545874));
#44687=CARTESIAN_POINT('Ctrl Pts',(374.764248512977,-22.0880887078402,-0.155351245687263));
#44688=CARTESIAN_POINT('Ctrl Pts',(374.768994679957,-22.0941602262679,-0.0352871480472851));
#44689=CARTESIAN_POINT('Ctrl Pts',(374.768237472187,-22.1002317446957,0.0850905815487117));
#44690=CARTESIAN_POINT('Ctrl Pts',(374.761959142466,-22.1063032631234,0.205238648986715));
#44691=CARTESIAN_POINT('Ctrl Pts',(374.755906399394,-22.1121566258388,0.321069676536308));
#44692=CARTESIAN_POINT('Ctrl Pts',(374.744722488423,-22.1180099885542,0.436686813924215));
#44693=CARTESIAN_POINT('Ctrl Pts',(374.728444549976,-22.1238633512696,0.551603362611651));
#44694=CARTESIAN_POINT('Ctrl Pts',(374.712169055594,-22.1297158351265,0.666502657048842));
#44695=CARTESIAN_POINT('Ctrl Pts',(374.690801112468,-22.1355683189834,0.780701162992073));
#44696=CARTESIAN_POINT('Ctrl Pts',(374.664429572601,-22.1414208028403,0.893718757266345));
#44697=CARTESIAN_POINT('Ctrl Pts',(374.638055614794,-22.1472738232967,1.00674671383995));
#44698=CARTESIAN_POINT('Ctrl Pts',(374.606677242145,-22.1531268437532,1.11859314114516));
#44699=CARTESIAN_POINT('Ctrl Pts',(374.570433959941,-22.1589798642096,1.22879023316963));
#44700=CARTESIAN_POINT('Ctrl Pts',(374.534178589861,-22.164834836768,1.33902407817497));
#44701=CARTESIAN_POINT('Ctrl Pts',(374.493055212875,-22.1706898093263,1.44760710182469));
#44702=CARTESIAN_POINT('Ctrl Pts',(374.447252276424,-22.1765447818846,1.55408939693147));
#44703=CARTESIAN_POINT('Ctrl Pts',(374.401397428115,-22.1824063903167,1.66069237630617));
#44704=CARTESIAN_POINT('Ctrl Pts',(374.350852597835,-22.1882679987489,1.76518949524678));
#44705=CARTESIAN_POINT('Ctrl Pts',(374.295853240312,-22.1941296071811,1.86715338522054));
#44706=CARTESIAN_POINT('Ctrl Pts',(374.240816796248,-22.1999951681463,1.96918603032332));
#44707=CARTESIAN_POINT('Ctrl Pts',(374.181320055366,-22.2058607291115,2.06868169139114));
#44708=CARTESIAN_POINT('Ctrl Pts',(374.117642107897,-22.2117262900767,2.16524151970987));
#44709=CARTESIAN_POINT('Ctrl Pts',(374.053871047459,-22.2176004279483,2.26194254247199));
#44710=CARTESIAN_POINT('Ctrl Pts',(373.985906820052,-22.22347456582,2.35569883168704));
#44711=CARTESIAN_POINT('Ctrl Pts',(373.914069138321,-22.2293487036916,2.44614411307786));
#44712=CARTESIAN_POINT('Ctrl Pts',(373.895902456609,-22.2308341858296,2.46901638010719));
#44713=CARTESIAN_POINT('Ctrl Pts',(373.877488248296,-22.2323196679675,2.49167708902266));
#44714=CARTESIAN_POINT('Ctrl Pts',(373.858832048042,-22.2338051501055,2.51412069824459));
#44715=CARTESIAN_POINT('Ctrl Pts',(373.785064254748,-22.2396788402356,2.60286414564367));
#44716=CARTESIAN_POINT('Ctrl Pts',(373.707264507631,-22.2455525303657,2.688505969082));
#44717=CARTESIAN_POINT('Ctrl Pts',(373.625723502741,-22.2514262204958,2.77065759339582));
#44718=CARTESIAN_POINT('Ctrl Pts',(373.544287775022,-22.257292327135,2.85270315217211));
#44719=CARTESIAN_POINT('Ctrl Pts',(373.459120683839,-22.2631584337742,2.93126718258746));
#44720=CARTESIAN_POINT('Ctrl Pts',(373.37055347917,-22.2690245404133,3.00599365429825));
#44721=CARTESIAN_POINT('Ctrl Pts',(373.282076966284,-22.2748846402278,3.08064360697555));
#44722=CARTESIAN_POINT('Ctrl Pts',(373.190207579146,-22.2807447400424,3.15146355244152));
#44723=CARTESIAN_POINT('Ctrl Pts',(373.095313279593,-22.2866048398569,3.218134348025));
#44724=CARTESIAN_POINT('Ctrl Pts',(372.996995426842,-22.2926763576761,3.28721046212124));
#44725=CARTESIAN_POINT('Ctrl Pts',(372.895430596163,-22.2987478754953,3.35183207104542));
#44726=CARTESIAN_POINT('Ctrl Pts',(372.791065700638,-22.3048193933144,3.41168973701297));
#44727=CARTESIAN_POINT('Ctrl Pts',(372.690450702543,-22.3106727576161,3.46939667876823));
#44728=CARTESIAN_POINT('Ctrl Pts',(372.587233782069,-22.3165261219178,3.52267590579358));
#44729=CARTESIAN_POINT('Ctrl Pts',(372.481844050169,-22.3223794862195,3.57129478346174));
#44730=CARTESIAN_POINT('Ctrl Pts',(372.376470142345,-22.3282319716492,3.61990636109416));
#44731=CARTESIAN_POINT('Ctrl Pts',(372.268924446838,-22.334084457079,3.66385880770208));
#44732=CARTESIAN_POINT('Ctrl Pts',(372.159658582617,-22.3399369425087,3.70296650687138));
#44733=CARTESIAN_POINT('Ctrl Pts',(372.050382700368,-22.3457899645229,3.74207779162542));
#44734=CARTESIAN_POINT('Ctrl Pts',(371.939386724887,-22.351642986537,3.77634330670344));
#44735=CARTESIAN_POINT('Ctrl Pts',(371.827139384565,-22.3574960085512,3.80562667729063));
#44736=CARTESIAN_POINT('Ctrl Pts',(371.714854607794,-22.3633509826504,3.83491981439346));
#44737=CARTESIAN_POINT('Ctrl Pts',(371.601318035845,-22.3692059567497,3.85922739868854));
#44738=CARTESIAN_POINT('Ctrl Pts',(371.487009888607,-22.3750609308489,3.87846388496112));
#44739=CARTESIAN_POINT('Ctrl Pts',(371.372572188149,-22.3809225407896,3.89772217325554));
#44740=CARTESIAN_POINT('Ctrl Pts',(371.257361574639,-22.3867841507303,3.91189782341989));
#44741=CARTESIAN_POINT('Ctrl Pts',(371.141864811662,-22.3926457606711,3.92095700924605));
#44742=CARTESIAN_POINT('Ctrl Pts',(371.026290168578,-22.3985113231277,3.93002230373129));
#44743=CARTESIAN_POINT('Ctrl Pts',(370.910429403701,-22.4043768855844,3.93396425002952));
#44744=CARTESIAN_POINT('Ctrl Pts',(370.794768970429,-22.4102424480411,3.93280115005445));
#44745=CARTESIAN_POINT('Ctrl Pts',(370.678939413645,-22.4161165873679,3.93163634934608));
#44746=CARTESIAN_POINT('Ctrl Pts',(370.563311184037,-22.4219907266948,3.9253516268132));
#44747=CARTESIAN_POINT('Ctrl Pts',(370.448365384261,-22.4278648660216,3.91401707861642));
#44748=CARTESIAN_POINT('Ctrl Pts',(370.419297600566,-22.4293503331868,3.91115076948723));
#44749=CARTESIAN_POINT('Ctrl Pts',(370.390273403415,-22.430835800352,3.90796178063459));
#44750=CARTESIAN_POINT('Ctrl Pts',(370.361300449601,-22.4323212675171,3.90445175868131));
#44751=CARTESIAN_POINT('Ctrl Pts',(370.24673837912,-22.4381949590698,3.89057276708868));
#44752=CARTESIAN_POINT('Ctrl Pts',(370.132596868298,-22.4440686506226,3.87162427043359));
#44753=CARTESIAN_POINT('Ctrl Pts',(370.019360029201,-22.4499423421753,3.84763989285173));
#44754=CARTESIAN_POINT('Ctrl Pts',(369.90626938917,-22.4558084502576,3.82368648128416));
#44755=CARTESIAN_POINT('Ctrl Pts',(369.794081498555,-22.4616745583399,3.79471020352575));
#44756=CARTESIAN_POINT('Ctrl Pts',(369.683275106397,-22.4675406664223,3.76079640435063));
#44757=CARTESIAN_POINT('Ctrl Pts',(369.572582178309,-22.4734007676986,3.72691733239324));
#44758=CARTESIAN_POINT('Ctrl Pts',(369.463268327563,-22.4792608689749,3.68811091591094));
#44759=CARTESIAN_POINT('Ctrl Pts',(369.355801208018,-22.4851209702513,3.64451334609282));
#44760=CARTESIAN_POINT('Ctrl Pts',(369.244456976512,-22.4911924875295,3.59934289835524));
#44761=CARTESIAN_POINT('Ctrl Pts',(369.135095683615,-22.4972640048077,3.5490291612149));
#44762=CARTESIAN_POINT('Ctrl Pts',(369.028219627798,-22.503335522086,3.49377993012068));
#44763=CARTESIAN_POINT('Ctrl Pts',(368.925183661447,-22.5091888878862,3.4405158208454));
#44764=CARTESIAN_POINT('Ctrl Pts',(368.824457813454,-22.5150422536864,3.38266498754485));
#44765=CARTESIAN_POINT('Ctrl Pts',(368.726470193779,-22.5208956194866,3.32046190229214));
#44766=CARTESIAN_POINT('Ctrl Pts',(368.62849728658,-22.5267481064257,3.25826815660054));
#44767=CARTESIAN_POINT('Ctrl Pts',(368.533262138914,-22.5326005933649,3.19172367967013));
#44768=CARTESIAN_POINT('Ctrl Pts',(368.441165552764,-22.5384530803041,3.12110734624765));
#44769=CARTESIAN_POINT('Ctrl Pts',(368.349060522606,-22.5443061038369,3.05048453826534));
#44770=CARTESIAN_POINT('Ctrl Pts',(368.260094953887,-22.5501591273698,2.97578938304197));
#44771=CARTESIAN_POINT('Ctrl Pts',(368.17463754566,-22.5560121509026,2.89734182684032));
#44772=CARTESIAN_POINT('Ctrl Pts',(368.089151635793,-22.561867126528,2.81886810691423));
#44773=CARTESIAN_POINT('Ctrl Pts',(368.007176517172,-22.5677221021535,2.73663977670339));
#44774=CARTESIAN_POINT('Ctrl Pts',(367.929044405982,-22.5735770777789,2.65101399406912));
#44775=CARTESIAN_POINT('Ctrl Pts',(367.850823742321,-22.5794386892492,2.56529116587223));
#44776=CARTESIAN_POINT('Ctrl Pts',(367.776455058126,-22.5853003007194,2.47616350511215));
#44777=CARTESIAN_POINT('Ctrl Pts',(367.706230657093,-22.5911619121896,2.38402170573178));
#44778=CARTESIAN_POINT('Ctrl Pts',(367.635958903325,-22.5970274761796,2.29181777458389));
#44779=CARTESIAN_POINT('Ctrl Pts',(367.56983723228,-22.6028930401696,2.19659599626579));
#44780=CARTESIAN_POINT('Ctrl Pts',(367.508113975826,-22.6087586041595,2.09877506321652));
#44781=CARTESIAN_POINT('Ctrl Pts',(367.446300465141,-22.6146327450132,2.00081109246209));
#44782=CARTESIAN_POINT('Ctrl Pts',(367.388898408793,-22.620506885867,1.90024073939001));
#44783=CARTESIAN_POINT('Ctrl Pts',(367.336109714849,-22.6263810267207,1.79750627832298));
#44784=CARTESIAN_POINT('Ctrl Pts',(367.322760509952,-22.6278664794567,1.77152678786151));
#44785=CARTESIAN_POINT('Ctrl Pts',(367.309706078323,-22.6293519321928,1.74540899848703));
#44786=CARTESIAN_POINT('Ctrl Pts',(367.296949187031,-22.6308373849288,1.7191602366962));
#44787=CARTESIAN_POINT('Ctrl Pts',(367.242672211498,-22.6371575674847,1.6074791563363));
#44788=CARTESIAN_POINT('Ctrl Pts',(367.19362551988,-22.6434777500406,1.4930970559787));
#44789=CARTESIAN_POINT('Ctrl Pts',(367.150065578657,-22.6497979325966,1.37650796486861));
#44790=CARTESIAN_POINT('Ctrl Pts',(367.106647535126,-22.6560975269861,1.26029866589119));
#44791=CARTESIAN_POINT('Ctrl Pts',(367.068680713728,-22.6623971213756,1.14189700515019));
#44792=CARTESIAN_POINT('Ctrl Pts',(367.036373913979,-22.6686967157651,1.0218174173262));
#44793=CARTESIAN_POINT('Ctrl Pts',(367.004131677013,-22.6749837208745,0.901977799802725));
#44794=CARTESIAN_POINT('Ctrl Pts',(366.977527006976,-22.681270725984,0.780467237829525));
#44795=CARTESIAN_POINT('Ctrl Pts',(366.956720096784,-22.6875577310934,0.657818089785108));
#44796=CARTESIAN_POINT('Ctrl Pts',(366.935976328002,-22.6938256574271,0.535541137333476));
#44797=CARTESIAN_POINT('Ctrl Pts',(366.920995294742,-22.7000935837608,0.412132796286274));
#44798=CARTESIAN_POINT('Ctrl Pts',(366.911886720925,-22.7063615100944,0.288137141606198));
#44799=CARTESIAN_POINT('Ctrl Pts',(366.904875028599,-22.7111864993694,0.1926864818321));
#44800=CARTESIAN_POINT('Ctrl Pts',(366.901342248334,-22.7160114886443,0.0968881668734049));
#44801=CARTESIAN_POINT('Ctrl Pts',(366.901317979184,-22.7208364779192,0.000995388470100028));
#44802=CARTESIAN_POINT('',(366.901319515466,-23.9708364779953,-0.00361596385032392));
#44803=CARTESIAN_POINT('Ctrl Pts',(366.901317979183,-22.7208364779651,0.00099538755728252));
#44804=CARTESIAN_POINT('Ctrl Pts',(366.901287676336,-22.7268610418477,-0.118737970686335));
#44805=CARTESIAN_POINT('Ctrl Pts',(366.906729329308,-22.7328856057302,-0.238412572221518));
#44806=CARTESIAN_POINT('Ctrl Pts',(366.91760070142,-22.7389101696128,-0.357513290336023));
#44807=CARTESIAN_POINT('Ctrl Pts',(366.928480551288,-22.7449394315943,-0.476706886035791));
#44808=CARTESIAN_POINT('Ctrl Pts',(366.944798523797,-22.7509686935757,-0.595325330626995));
#44809=CARTESIAN_POINT('Ctrl Pts',(366.966460780102,-22.7569979555571,-0.712860899403337));
#44810=CARTESIAN_POINT('Ctrl Pts',(366.988162752378,-22.763038271696,-0.830611960007766));
#44811=CARTESIAN_POINT('Ctrl Pts',(367.015228520396,-22.7690785878349,-0.947275804961401));
#44812=CARTESIAN_POINT('Ctrl Pts',(367.047513327082,-22.7751189039738,-1.06235609886111));
#44813=CARTESIAN_POINT('Ctrl Pts',(367.079828053996,-22.781164818029,-1.17754304443784));
#44814=CARTESIAN_POINT('Ctrl Pts',(367.117371345748,-22.7872107320841,-1.29114315418572));
#44815=CARTESIAN_POINT('Ctrl Pts',(367.159949518888,-22.7932566461392,-1.40267827516699));
#44816=CARTESIAN_POINT('Ctrl Pts',(367.202620316752,-22.7993157124995,-1.51445603008713));
#44817=CARTESIAN_POINT('Ctrl Pts',(367.250347743227,-22.8053747788597,-1.6241594678244));
#44818=CARTESIAN_POINT('Ctrl Pts',(367.302890635125,-22.81143384522,-1.73133208924998));
#44819=CARTESIAN_POINT('Ctrl Pts',(367.354689077928,-22.8174070642601,-1.83698624532299));
#44820=CARTESIAN_POINT('Ctrl Pts',(367.41116717659,-22.8233802833003,-1.94018057508564));
#44821=CARTESIAN_POINT('Ctrl Pts',(367.472052951154,-22.8293535023405,-2.04050575306956));
#44822=CARTESIAN_POINT('Ctrl Pts',(367.531924296908,-22.8352272005068,-2.13915939526883));
#44823=CARTESIAN_POINT('Ctrl Pts',(367.596240994351,-22.8411008986732,-2.23534004410958));
#44824=CARTESIAN_POINT('Ctrl Pts',(367.664772841031,-22.8469745968396,-2.32862049627674));
#44825=CARTESIAN_POINT('Ctrl Pts',(367.733216206224,-22.8528407114727,-2.42178051402745));
#44826=CARTESIAN_POINT('Ctrl Pts',(367.805863655565,-22.8587068261058,-2.51204745167245));
#44827=CARTESIAN_POINT('Ctrl Pts',(367.88244007591,-22.8645729407389,-2.59902031307939));
#44828=CARTESIAN_POINT('Ctrl Pts',(367.958938082337,-22.8704330484964,-2.685904114658));
#44829=CARTESIAN_POINT('Ctrl Pts',(368.0393567858,-22.8762931562539,-2.76950024117513));
#44830=CARTESIAN_POINT('Ctrl Pts',(368.12337932194,-22.8821532640113,-2.84943876572168));
#44831=CARTESIAN_POINT('Ctrl Pts',(368.210433023802,-22.8882247788339,-2.93226112270937));
#44832=CARTESIAN_POINT('Ctrl Pts',(368.301355221014,-22.8942962936564,-3.01115663087208));
#44833=CARTESIAN_POINT('Ctrl Pts',(368.39574953221,-22.9003678084789,-3.08575331868064));
#44834=CARTESIAN_POINT('Ctrl Pts',(368.486752361127,-22.9062211805483,-3.15766983072856));
#44835=CARTESIAN_POINT('Ctrl Pts',(368.580981747322,-22.9120745526176,-3.22559083205616));
#44836=CARTESIAN_POINT('Ctrl Pts',(368.678047586308,-22.917927924687,-3.28922293802281));
#44837=CARTESIAN_POINT('Ctrl Pts',(368.775098849769,-22.9237804178067,-3.35284548891371));
#44838=CARTESIAN_POINT('Ctrl Pts',(368.874985373697,-22.9296329109265,-3.41218019856358));
#44839=CARTESIAN_POINT('Ctrl Pts',(368.977287856577,-22.9354854040462,-3.46697686631361));
#44840=CARTESIAN_POINT('Ctrl Pts',(369.079599717541,-22.9413384336649,-3.52177855728224));
#44841=CARTESIAN_POINT('Ctrl Pts',(369.184327613512,-22.9471914632835,-3.57204118429289));
#44842=CARTESIAN_POINT('Ctrl Pts',(369.291028057516,-22.9530444929022,-3.61756072602311));
#44843=CARTESIAN_POINT('Ctrl Pts',(369.397764086232,-22.9588994745124,-3.6630954485688));
#44844=CARTESIAN_POINT('Ctrl Pts',(369.506473591278,-22.9647544561226,-3.70388377841954));
#44845=CARTESIAN_POINT('Ctrl Pts',(369.616694222458,-22.9706094377329,-3.73977027286435));
#44846=CARTESIAN_POINT('Ctrl Pts',(369.727039770731,-22.976471055009,-3.77569743879262));
#44847=CARTESIAN_POINT('Ctrl Pts',(369.838899470347,-22.9823326722852,-3.80671155303308));
#44848=CARTESIAN_POINT('Ctrl Pts',(369.951796870379,-22.9881942895613,-3.8327073609706));
#44849=CARTESIAN_POINT('Ctrl Pts',(370.064770395858,-22.9940598592601,-3.85872069758919));
#44850=CARTESIAN_POINT('Ctrl Pts',(370.178782609719,-22.9999254289589,-3.87970891541977));
#44851=CARTESIAN_POINT('Ctrl Pts',(370.293349678834,-23.0057909986577,-3.8956183635332));
#44852=CARTESIAN_POINT('Ctrl Pts',(370.408084268749,-23.011665145035,-3.91155107455712));
#44853=CARTESIAN_POINT('Ctrl Pts',(370.523374923347,-23.0175392914124,-3.92239015648457));
#44854=CARTESIAN_POINT('Ctrl Pts',(370.638735461975,-23.0234134377898,-3.92813397534163));
#44855=CARTESIAN_POINT('Ctrl Pts',(370.667906653746,-23.0248988317772,-3.92958641344023));
#44856=CARTESIAN_POINT('Ctrl Pts',(370.697082330539,-23.0263842257647,-3.93071330423601));
#44857=CARTESIAN_POINT('Ctrl Pts',(370.726254677598,-23.0278696197521,-3.93151514687068));
#44858=CARTESIAN_POINT('Ctrl Pts',(370.84161110108,-23.0337433239663,-3.93468587901459));
#44859=CARTESIAN_POINT('Ctrl Pts',(370.957299310999,-23.0396170281805,-3.93278049909092));
#44860=CARTESIAN_POINT('Ctrl Pts',(371.072835528839,-23.0454907323946,-3.92576085853677));
#44861=CARTESIAN_POINT('Ctrl Pts',(371.188222581599,-23.051356853259,-3.91875028081384));
#44862=CARTESIAN_POINT('Ctrl Pts',(371.303457623906,-23.0572229741233,-3.90663859820559));
#44863=CARTESIAN_POINT('Ctrl Pts',(371.418054553035,-23.0630890949877,-3.88943960813041));
#44864=CARTESIAN_POINT('Ctrl Pts',(371.532534138928,-23.06894920915,-3.87225822921777));
#44865=CARTESIAN_POINT('Ctrl Pts',(371.646376505183,-23.0748093233124,-3.8499999653729));
#44866=CARTESIAN_POINT('Ctrl Pts',(371.759099023238,-23.0806694374747,-3.822730540803));
#44867=CARTESIAN_POINT('Ctrl Pts',(371.875887904304,-23.0867409499617,-3.79447739637549));
#44868=CARTESIAN_POINT('Ctrl Pts',(371.991474166008,-23.0928124624488,-3.76084474692569));
#44869=CARTESIAN_POINT('Ctrl Pts',(372.105330357215,-23.0988839749358,-3.72196402651858));
#44870=CARTESIAN_POINT('Ctrl Pts',(372.215095992104,-23.1047373537975,-3.68448018909865));
#44871=CARTESIAN_POINT('Ctrl Pts',(372.32325330665,-23.1105907326592,-3.64211903554325));
#44872=CARTESIAN_POINT('Ctrl Pts',(372.429344287467,-23.1164441115208,-3.59504932846093));
#44873=CARTESIAN_POINT('Ctrl Pts',(372.535419339916,-23.1222966115635,-3.54798668836569));
#44874=CARTESIAN_POINT('Ctrl Pts',(372.639428297962,-23.1281491116062,-3.49621706790352));
#44875=CARTESIAN_POINT('Ctrl Pts',(372.740933608191,-23.1340016116488,-3.4399571745752));
#44876=CARTESIAN_POINT('Ctrl Pts',(372.84244822554,-23.1398546483129,-3.38369212272267));
#44877=CARTESIAN_POINT('Ctrl Pts',(372.941458377355,-23.145707684977,-3.32293617983975));
#44878=CARTESIAN_POINT('Ctrl Pts',(373.037552204011,-23.151560721641,-3.25795141085801));
#44879=CARTESIAN_POINT('Ctrl Pts',(373.133678079901,-23.1574157104112,-3.19294496814228));
#44880=CARTESIAN_POINT('Ctrl Pts',(373.226885354509,-23.1632706991813,-3.12370712612603));
#44881=CARTESIAN_POINT('Ctrl Pts',(373.316792763345,-23.1691256879514,-3.05054213552566));
#44882=CARTESIAN_POINT('Ctrl Pts',(373.406802069448,-23.1749873125189,-2.97729422281013));
#44883=CARTESIAN_POINT('Ctrl Pts',(373.493503724484,-23.1808489370864,-2.90011053877019));
#44884=CARTESIAN_POINT('Ctrl Pts',(373.576550993332,-23.1867105616539,-2.81933439047121));
#44885=CARTESIAN_POINT('Ctrl Pts',(373.659654261159,-23.1925761387294,-2.73850377461465));
#44886=CARTESIAN_POINT('Ctrl Pts',(373.739097953685,-23.1984417158049,-2.65407617108448));
#44887=CARTESIAN_POINT('Ctrl Pts',(373.814574696856,-23.2043072928804,-2.56642906505969));
#44888=CARTESIAN_POINT('Ctrl Pts',(373.890161803387,-23.2101814467011,-2.47865379996664));
#44889=CARTESIAN_POINT('Ctrl Pts',(373.961770129644,-23.2160556005217,-2.38764996060215));
#44890=CARTESIAN_POINT('Ctrl Pts',(374.029134739244,-23.2219297543424,-2.29382520362811));
#44891=CARTESIAN_POINT('Ctrl Pts',(374.046168429106,-23.2234150819495,-2.27010085012677));
#44892=CARTESIAN_POINT('Ctrl Pts',(374.062931014547,-23.2249004095566,-2.24619626191627));
#44893=CARTESIAN_POINT('Ctrl Pts',(374.079418679064,-23.2263857371637,-2.2221182754591));
#44894=CARTESIAN_POINT('Ctrl Pts',(374.144617931055,-23.2322593555188,-2.12690365578005));
#44895=CARTESIAN_POINT('Ctrl Pts',(374.205731692429,-23.2381329738739,-2.02865848239646));
#44896=CARTESIAN_POINT('Ctrl Pts',(374.262465646344,-23.244006592229,-1.92776858272025));
#44897=CARTESIAN_POINT('Ctrl Pts',(374.31912634959,-23.2498726270041,-1.82700894459285));
#44898=CARTESIAN_POINT('Ctrl Pts',(374.371418290418,-23.2557386617792,-1.72361172766874));
#44899=CARTESIAN_POINT('Ctrl Pts',(374.419089542026,-23.2616046965543,-1.61799287364358));
#44900=CARTESIAN_POINT('Ctrl Pts',(374.466711978198,-23.2674647245005,-1.51248217349212));
#44901=CARTESIAN_POINT('Ctrl Pts',(374.509722967717,-23.2733247524468,-1.40475473565745));
#44902=CARTESIAN_POINT('Ctrl Pts',(374.547916101235,-23.279184780393,-1.29525173320391));
#44903=CARTESIAN_POINT('Ctrl Pts',(374.587487810059,-23.2852563251506,-1.18179623664475));
#44904=CARTESIAN_POINT('Ctrl Pts',(374.621887072299,-23.2913278699082,-1.06643497056012));
#44905=CARTESIAN_POINT('Ctrl Pts',(374.650938386052,-23.2973994146658,-0.949682425023584));
#44906=CARTESIAN_POINT('Ctrl Pts',(374.678945401484,-23.3032527075383,-0.837126746045857));
#44907=CARTESIAN_POINT('Ctrl Pts',(374.701982222204,-23.3091060004108,-0.723278524510714));
#44908=CARTESIAN_POINT('Ctrl Pts',(374.719942367608,-23.3149592932833,-0.608614108627111));
#44909=CARTESIAN_POINT('Ctrl Pts',(374.737899817165,-23.3208117075672,-0.49396690405588));
#44910=CARTESIAN_POINT('Ctrl Pts',(374.750782042665,-23.3266641218511,-0.378504156805758));
#44911=CARTESIAN_POINT('Ctrl Pts',(374.758533943495,-23.3325165361349,-0.26271101396801));
#44912=CARTESIAN_POINT('Ctrl Pts',(374.76628655554,-23.3383694873619,-0.146907247424043));
#44913=CARTESIAN_POINT('Ctrl Pts',(374.768907879622,-23.3442224385889,-0.0307734372891979));
#44914=CARTESIAN_POINT('Ctrl Pts',(374.766394858187,-23.3500753898159,0.0852022713527328));
#44915=CARTESIAN_POINT('Ctrl Pts',(374.763880998418,-23.3559302935623,0.20121666899282));
#44916=CARTESIAN_POINT('Ctrl Pts',(374.756229396263,-23.3617851973086,0.317072447428953));
#44917=CARTESIAN_POINT('Ctrl Pts',(374.743489029117,-23.367640101055,0.432284301783718));
#44918=CARTESIAN_POINT('Ctrl Pts',(374.730734220103,-23.3735016416387,0.547626754755979));
#44919=CARTESIAN_POINT('Ctrl Pts',(374.712879178201,-23.3793631822224,0.662323415885602));
#44920=CARTESIAN_POINT('Ctrl Pts',(374.690024418826,-23.3852247228061,0.775896823020315));
#44921=CARTESIAN_POINT('Ctrl Pts',(374.667154246245,-23.3910902164017,0.889546823848221));
#44922=CARTESIAN_POINT('Ctrl Pts',(374.6392777413,-23.3969557099974,1.00207166225154));
#44923=CARTESIAN_POINT('Ctrl Pts',(374.606545477403,-23.4028212035931,1.11300842376944));
#44924=CARTESIAN_POINT('Ctrl Pts',(374.573765343465,-23.4086952753128,1.22410742726817));
#44925=CARTESIAN_POINT('Ctrl Pts',(374.536115411754,-23.4145693470325,1.33361332951313));
#44926=CARTESIAN_POINT('Ctrl Pts',(374.493794614669,-23.4204434187523,1.44108252103892));
#44927=CARTESIAN_POINT('Ctrl Pts',(374.483087416051,-23.4219295640267,1.46827232033845));
#44928=CARTESIAN_POINT('Ctrl Pts',(374.472081468001,-23.4234157093011,1.49533187305735));
#44929=CARTESIAN_POINT('Ctrl Pts',(374.46078045256,-23.4249018545755,1.52225425458903));
#44930=CARTESIAN_POINT('Ctrl Pts',(374.416114739073,-23.4307756399335,1.62866127493066));
#44931=CARTESIAN_POINT('Ctrl Pts',(374.36668741188,-23.4366494252915,1.73327796734298));
#44932=CARTESIAN_POINT('Ctrl Pts',(374.31266315186,-23.4425232106496,1.83564783753799));
#44933=CARTESIAN_POINT('Ctrl Pts',(374.258708644464,-23.4483894121566,1.93788553439055));
#44934=CARTESIAN_POINT('Ctrl Pts',(374.200169198598,-23.4542556136636,2.0378818160345));
#44935=CARTESIAN_POINT('Ctrl Pts',(374.137257779935,-23.4601218151706,2.13519948495123));
#44936=CARTESIAN_POINT('Ctrl Pts',(374.074410785778,-23.4659820093878,2.23241749560526));
#44937=CARTESIAN_POINT('Ctrl Pts',(374.007200947151,-23.4718422036049,2.32696200477624));
#44938=CARTESIAN_POINT('Ctrl Pts',(373.935887106773,-23.477702397822,2.41842038641772));
#44939=CARTESIAN_POINT('Ctrl Pts',(373.862002061246,-23.4837738800789,2.51317628030224));
#44940=CARTESIAN_POINT('Ctrl Pts',(373.783711702946,-23.4898453623357,2.60461890883726));
#44941=CARTESIAN_POINT('Ctrl Pts',(373.701353200303,-23.4959168445926,2.6923219195701));
#44942=CARTESIAN_POINT('Ctrl Pts',(373.621952169263,-23.5017703015603,2.77687553885777));
#44943=CARTESIAN_POINT('Ctrl Pts',(373.538770447679,-23.507623758528,2.85795317135498));
#44944=CARTESIAN_POINT('Ctrl Pts',(373.452150606204,-23.5134772154956,2.93520709276592));
#44945=CARTESIAN_POINT('Ctrl Pts',(373.365543782114,-23.5193297927954,3.01244940431997));
#44946=CARTESIAN_POINT('Ctrl Pts',(373.27550017374,-23.5251823700951,3.08586887246897));
#44947=CARTESIAN_POINT('Ctrl Pts',(373.182397599193,-23.5310349473949,3.15515617784124));
#44948=CARTESIAN_POINT('Ctrl Pts',(373.089286502858,-23.5368880603879,3.22444982516199));
#44949=CARTESIAN_POINT('Ctrl Pts',(372.993116215198,-23.5427411733809,3.28961031117638));
#44950=CARTESIAN_POINT('Ctrl Pts',(372.894295286998,-23.5485942863739,3.35037042315363));
#44951=CARTESIAN_POINT('Ctrl Pts',(372.79544141747,-23.5544493504649,3.41115078912777));
#44952=CARTESIAN_POINT('Ctrl Pts',(372.693935502195,-23.5603044145559,3.46752764805658));
#44953=CARTESIAN_POINT('Ctrl Pts',(372.59021191469,-23.5661594786469,3.51927905186658));
#44954=CARTESIAN_POINT('Ctrl Pts',(372.486370805763,-23.5720211766722,3.57108909131369));
#44955=CARTESIAN_POINT('Ctrl Pts',(372.380307379329,-23.5778828746975,3.61826303085876));
#44956=CARTESIAN_POINT('Ctrl Pts',(372.272477358661,-23.5837445727229,3.66062648148104));
#44957=CARTESIAN_POINT('Ctrl Pts',(372.164574647179,-23.58961022226,3.70301849032574));
#44958=CARTESIAN_POINT('Ctrl Pts',(372.054903359969,-23.5954758717971,3.74059341940055));
#44959=CARTESIAN_POINT('Ctrl Pts',(371.94393413421,-23.6013415213343,3.77322682978001));
#44960=CARTESIAN_POINT('Ctrl Pts',(371.832802687362,-23.6072157456095,3.80590794552373));
#44961=CARTESIAN_POINT('Ctrl Pts',(371.720369914805,-23.6130899698848,3.83363302716284));
#44962=CARTESIAN_POINT('Ctrl Pts',(371.60711644896,-23.61896419416,3.85632873733921));
#44963=CARTESIAN_POINT('Ctrl Pts',(371.578493902312,-23.6204487867691,3.86206462381642));
#44964=CARTESIAN_POINT('Ctrl Pts',(371.549818958025,-23.6219333793781,3.86747953104869));
#44965=CARTESIAN_POINT('Ctrl Pts',(371.521099406255,-23.6234179719871,3.87257280091881));
#44966=CARTESIAN_POINT('Ctrl Pts',(371.407470725055,-23.6292917509944,3.8927242831904));
#44967=CARTESIAN_POINT('Ctrl Pts',(371.29276517905,-23.6351655300016,3.90790395531421));
#44968=CARTESIAN_POINT('Ctrl Pts',(371.177455643018,-23.6410393090088,3.91800273828579));
#44969=CARTESIAN_POINT('Ctrl Pts',(371.062294955964,-23.6469055057638,3.92808848509783));
#44970=CARTESIAN_POINT('Ctrl Pts',(370.946532237188,-23.6527717025188,3.93310635023573));
#44971=CARTESIAN_POINT('Ctrl Pts',(370.830650320756,-23.6586378992737,3.93299829000797));
#44972=CARTESIAN_POINT('Ctrl Pts',(370.714887042171,-23.6644980903206,3.93289034041034));
#44973=CARTESIAN_POINT('Ctrl Pts',(370.599005219337,-23.6703582813675,3.92766690421058));
#44974=CARTESIAN_POINT('Ctrl Pts',(370.48349190796,-23.6762184724144,3.91732180911012));
#44975=CARTESIAN_POINT('Ctrl Pts',(370.363813689121,-23.6822899564555,3.90660371488717));
#44976=CARTESIAN_POINT('Ctrl Pts',(370.244531506929,-23.6883614404965,3.8903876239092));
#44977=CARTESIAN_POINT('Ctrl Pts',(370.126186412439,-23.6944329245375,3.86872574145181));
#44978=CARTESIAN_POINT('Ctrl Pts',(370.012091077365,-23.7002863822498,3.84784173482723));
#44979=CARTESIAN_POINT('Ctrl Pts',(369.898867127292,-23.7061398399621,3.82189640608091));
#44980=CARTESIAN_POINT('Ctrl Pts',(369.786992468093,-23.7119932976744,3.79098912391743));
#44981=CARTESIAN_POINT('Ctrl Pts',(369.675134594174,-23.7178458771545,3.76008647897377));
#44982=CARTESIAN_POINT('Ctrl Pts',(369.564626006703,-23.7236984566347,3.72422347089168));
#44983=CARTESIAN_POINT('Ctrl Pts',(369.455931446481,-23.7295510361148,3.68354990650394));
#44984=CARTESIAN_POINT('Ctrl Pts',(369.34722691083,-23.7354041527146,3.64287260930569));
#44985=CARTESIAN_POINT('Ctrl Pts',(369.240337120329,-23.7412572693143,3.59738402295964));
#44986=CARTESIAN_POINT('Ctrl Pts',(369.135708092673,-23.7471103859141,3.54728260522892));
#44987=CARTESIAN_POINT('Ctrl Pts',(369.031044162269,-23.7529654550299,3.49716447438157));
#44988=CARTESIAN_POINT('Ctrl Pts',(368.928642866734,-23.7588205241456,3.44243063069062));
#44989=CARTESIAN_POINT('Ctrl Pts',(368.828926185299,-23.7646755932614,3.38332576885757));
#44990=CARTESIAN_POINT('Ctrl Pts',(368.729096487465,-23.7705372983664,3.32415391904925));
#44991=CARTESIAN_POINT('Ctrl Pts',(368.631957832316,-23.7763990034714,3.26060137397325));
#44992=CARTESIAN_POINT('Ctrl Pts',(368.537903807971,-23.7822607085764,3.19295655040372));
#44993=CARTESIAN_POINT('Ctrl Pts',(368.443786360278,-23.7881263663986,3.12526611197358));
#44994=CARTESIAN_POINT('Ctrl Pts',(368.352758008835,-23.7939920242208,3.05347815537743));
#44995=CARTESIAN_POINT('Ctrl Pts',(368.265178452428,-23.7998576820431,2.97792070735228));
#44996=CARTESIAN_POINT('Ctrl Pts',(368.177470842316,-23.8057319162871,2.90225278364609));
#44997=CARTESIAN_POINT('Ctrl Pts',(368.093222390468,-23.8116061505311,2.82280465122889));
#44998=CARTESIAN_POINT('Ctrl Pts',(368.012755272469,-23.8174803847751,2.73994043783507));
#44999=CARTESIAN_POINT('Ctrl Pts',(367.992419187765,-23.818964952983,2.71899854623452));
#45000=CARTESIAN_POINT('Ctrl Pts',(367.972324411649,-23.8204495211909,2.69783862802931));
#45001=CARTESIAN_POINT('Ctrl Pts',(367.952475719901,-23.8219340893987,2.67646687231542));
#45002=CARTESIAN_POINT('Ctrl Pts',(367.874845640598,-23.8277403737206,2.59287994820201));
#45003=CARTESIAN_POINT('Ctrl Pts',(367.800710733703,-23.8335466580424,2.50575695135316));
#45004=CARTESIAN_POINT('Ctrl Pts',(367.730415982015,-23.8393529423643,2.41542587837121));
#45005=CARTESIAN_POINT('Ctrl Pts',(367.660234682271,-23.8451498556559,2.32524059487712));
#45006=CARTESIAN_POINT('Ctrl Pts',(367.593881462807,-23.8509467689475,2.23185786899363));
#45007=CARTESIAN_POINT('Ctrl Pts',(367.531663925594,-23.8567436822391,2.13564183193501));
#45008=CARTESIAN_POINT('Ctrl Pts',(367.469503925471,-23.8625352347026,2.03951477285719));
#45009=CARTESIAN_POINT('Ctrl Pts',(367.411472236767,-23.8683267871661,1.94055996201908));
#45010=CARTESIAN_POINT('Ctrl Pts',(367.357835537159,-23.8741183396295,1.83917364761615));
#45011=CARTESIAN_POINT('Ctrl Pts',(367.304234736478,-23.8799060158194,1.73785519085511));
#45012=CARTESIAN_POINT('Ctrl Pts',(367.255023275686,-23.8856936920093,1.6341088381618));
#45013=CARTESIAN_POINT('Ctrl Pts',(367.210423457027,-23.8914813681991,1.52835807493371));
#45014=CARTESIAN_POINT('Ctrl Pts',(367.165842098073,-23.8972666488906,1.42265108156752));
#45015=CARTESIAN_POINT('Ctrl Pts',(367.125868749843,-23.903051929582,1.31494171714988));
#45016=CARTESIAN_POINT('Ctrl Pts',(367.090678486224,-23.9088372102735,1.20567544963205));
#45017=CARTESIAN_POINT('Ctrl Pts',(367.055483948564,-23.9146231936173,1.09639591115743));
#45018=CARTESIAN_POINT('Ctrl Pts',(367.025073795471,-23.9204091769612,0.985559492047928));
#45019=CARTESIAN_POINT('Ctrl Pts',(366.99957375711,-23.9261951603051,0.873628477854232));
#45020=CARTESIAN_POINT('Ctrl Pts',(366.974072376168,-23.931981448282,0.761691570472836));
#45021=CARTESIAN_POINT('Ctrl Pts',(366.953481710402,-23.937767736259,0.6486603683265));
#45022=CARTESIAN_POINT('Ctrl Pts',(366.937876438124,-23.9435540242359,0.535007755729943));
#45023=CARTESIAN_POINT('Ctrl Pts',(366.922259595966,-23.9493446022151,0.42127088013648));
#45024=CARTESIAN_POINT('Ctrl Pts',(366.911635576298,-23.9551351801943,0.306912095255886));
#45025=CARTESIAN_POINT('Ctrl Pts',(366.906027187634,-23.9609257581735,0.192409580431338));
#45026=CARTESIAN_POINT('Ctrl Pts',(366.902827554902,-23.9642293314374,0.127084936159333));
#45027=CARTESIAN_POINT('Ctrl Pts',(366.901259452096,-23.9675329047012,0.0617135537141975));
#45028=CARTESIAN_POINT('Ctrl Pts',(366.901319515466,-23.9708364779651,-0.00361596325308196));
#45029=CARTESIAN_POINT('',(369.0856199232,-24.9999241866122,3.52286027959241));
#45030=CARTESIAN_POINT('Ctrl Pts',(366.901319515466,-23.9708364779953,-0.0036159638503537));
#45031=CARTESIAN_POINT('Ctrl Pts',(366.901456107264,-23.9783492256021,-0.152183630750229));
#45032=CARTESIAN_POINT('Ctrl Pts',(366.910014340773,-23.9858619732089,-0.300376388370299));
#45033=CARTESIAN_POINT('Ctrl Pts',(366.926846153848,-23.9933747208157,-0.44738564860611));
#45034=CARTESIAN_POINT('Ctrl Pts',(366.944059171198,-24.0010576159569,-0.5977243516073));
#45035=CARTESIAN_POINT('Ctrl Pts',(366.969924781452,-24.0087405110982,-0.746825627686831));
#45036=CARTESIAN_POINT('Ctrl Pts',(367.004236650054,-24.0164234062394,-0.893849527115906));
#45037=CARTESIAN_POINT('Ctrl Pts',(367.010231224128,-24.0177656730964,-0.919535847671266));
#45038=CARTESIAN_POINT('Ctrl Pts',(367.016483487021,-24.0191079399534,-0.945158813959882));
#45039=CARTESIAN_POINT('Ctrl Pts',(367.022992190536,-24.0204502068104,-0.970714011920837));
#45040=CARTESIAN_POINT('Ctrl Pts',(367.051478761199,-24.0263248913126,-1.08256116409416));
#45041=CARTESIAN_POINT('Ctrl Pts',(367.084940277723,-24.0321995758149,-1.19333931436811));
#45042=CARTESIAN_POINT('Ctrl Pts',(367.123281110201,-24.0380742603171,-1.30257256685918));
#45043=CARTESIAN_POINT('Ctrl Pts',(367.161572432422,-24.0439413587258,-1.41166476434215));
#45044=CARTESIAN_POINT('Ctrl Pts',(367.204730404835,-24.0498084571345,-1.51921564525133));
#45045=CARTESIAN_POINT('Ctrl Pts',(367.252608796212,-24.0556755555432,-1.62476128428616));
#45046=CARTESIAN_POINT('Ctrl Pts',(367.300438138591,-24.0615366434055,-1.73019879713768));
#45047=CARTESIAN_POINT('Ctrl Pts',(367.352978111397,-24.0673977312678,-1.83363478038146));
#45048=CARTESIAN_POINT('Ctrl Pts',(367.410033485655,-24.0732588191302,-1.93462284955583));
#45049=CARTESIAN_POINT('Ctrl Pts',(367.469133693319,-24.0793299651757,-2.03923027589216));
#45050=CARTESIAN_POINT('Ctrl Pts',(367.533078883881,-24.0854011112212,-2.14121060684055));
#45051=CARTESIAN_POINT('Ctrl Pts',(367.601598550317,-24.0914722572667,-2.2400926116147));
#45052=CARTESIAN_POINT('Ctrl Pts',(367.667671284332,-24.0973265942577,-2.33544340271097));
#45053=CARTESIAN_POINT('Ctrl Pts',(367.737997104383,-24.1031809312487,-2.42791300605906));
#45054=CARTESIAN_POINT('Ctrl Pts',(367.812288408596,-24.1090352682398,-2.51710687810465));
#45055=CARTESIAN_POINT('Ctrl Pts',(367.886568467241,-24.1148887190525,-2.60628724876231));
#45056=CARTESIAN_POINT('Ctrl Pts',(367.964812552246,-24.1207421698653,-2.69219255682018));
#45057=CARTESIAN_POINT('Ctrl Pts',(368.046692534289,-24.126595620678,-2.7744610433796));
#45058=CARTESIAN_POINT('Ctrl Pts',(368.128579905949,-24.132449599761,-2.85673695461818));
#45059=CARTESIAN_POINT('Ctrl Pts',(368.214103535594,-24.138303578844,-2.93537509915258));
#45060=CARTESIAN_POINT('Ctrl Pts',(368.302898684382,-24.144157557927,-3.01005082874341));
#45061=CARTESIAN_POINT('Ctrl Pts',(368.391723301553,-24.150013479766,-3.08475134091618));
#45062=CARTESIAN_POINT('Ctrl Pts',(368.483821280868,-24.1558694016049,-3.15548655763097));
#45063=CARTESIAN_POINT('Ctrl Pts',(368.578795662652,-24.1617253234438,-3.22197278818994));
#45064=CARTESIAN_POINT('Ctrl Pts',(368.673877367559,-24.1675878626022,-3.2885341496399));
#45065=CARTESIAN_POINT('Ctrl Pts',(368.77184162403,-24.1734504017605,-3.35083670452901));
#45066=CARTESIAN_POINT('Ctrl Pts',(368.872263336832,-24.1793129409189,-3.40864064910112));
#45067=CARTESIAN_POINT('Ctrl Pts',(368.972752588234,-24.1851794229266,-3.46648346970289));
#45068=CARTESIAN_POINT('Ctrl Pts',(369.075702221223,-24.1910459049343,-3.51982146586649));
#45069=CARTESIAN_POINT('Ctrl Pts',(369.180665013877,-24.196912386942,-3.56846203383452));
#45070=CARTESIAN_POINT('Ctrl Pts',(369.285780885032,-24.2027874246699,-3.61717353956118));
#45071=CARTESIAN_POINT('Ctrl Pts',(369.392915394834,-24.2086624623977,-3.661173788335));
#45072=CARTESIAN_POINT('Ctrl Pts',(369.501603889699,-24.2145375001255,-3.70031924182562));
#45073=CARTESIAN_POINT('Ctrl Pts',(369.528915046232,-24.2160137748243,-3.71015567952021));
#45074=CARTESIAN_POINT('Ctrl Pts',(369.556324263869,-24.2174900495232,-3.71968582967798));
#45075=CARTESIAN_POINT('Ctrl Pts',(369.583824063438,-24.218966324222,-3.72890792078692));
#45076=CARTESIAN_POINT('Ctrl Pts',(369.693245676619,-24.2248404164544,-3.76560259136011));
#45077=CARTESIAN_POINT('Ctrl Pts',(369.804465679604,-24.2307145086869,-3.79753784266033));
#45078=CARTESIAN_POINT('Ctrl Pts',(369.91703237222,-24.2365886009193,-3.82453609557273));
#45079=CARTESIAN_POINT('Ctrl Pts',(370.029453951596,-24.2424551206759,-3.85149954419402));
#45080=CARTESIAN_POINT('Ctrl Pts',(370.143218370111,-24.2483216404325,-3.87353855580781));
#45081=CARTESIAN_POINT('Ctrl Pts',(370.257856559393,-24.2541881601892,-3.89052456318099));
#45082=CARTESIAN_POINT('Ctrl Pts',(370.372377571614,-24.2600486835013,-3.90749320836076));
#45083=CARTESIAN_POINT('Ctrl Pts',(370.487770171911,-24.2659092068134,-3.91941906260197));
#45084=CARTESIAN_POINT('Ctrl Pts',(370.603553474848,-24.2717697301256,-3.92622424240805));
#45085=CARTESIAN_POINT('Ctrl Pts',(370.723502227145,-24.2778410931051,-3.93327424708221));
#45086=CARTESIAN_POINT('Ctrl Pts',(370.843869884325,-24.2839124560846,-3.93482808927835));
#45087=CARTESIAN_POINT('Ctrl Pts',(370.964113675291,-24.2899838190641,-3.9308576728971));
#45088=CARTESIAN_POINT('Ctrl Pts',(371.080048827408,-24.2958376297676,-3.9270295265668));
#45089=CARTESIAN_POINT('Ctrl Pts',(371.195868389765,-24.3016914404711,-3.91806623889434));
#45090=CARTESIAN_POINT('Ctrl Pts',(371.311084975544,-24.3075452511746,-3.90399565971514));
#45091=CARTESIAN_POINT('Ctrl Pts',(371.426284413518,-24.3133981906493,-3.88992717467496));
#45092=CARTESIAN_POINT('Ctrl Pts',(371.540880643439,-24.319251130124,-3.87075295960273));
#45093=CARTESIAN_POINT('Ctrl Pts',(371.654391866833,-24.3251040695987,-3.84655269198321));
#45094=CARTESIAN_POINT('Ctrl Pts',(371.767913634676,-24.3309575527731,-3.82235017631749));
#45095=CARTESIAN_POINT('Ctrl Pts',(371.880349791616,-24.3368110359475,-3.79312076609747));
#45096=CARTESIAN_POINT('Ctrl Pts',(371.991229887442,-24.342664519122,-3.75899501796459));
#45097=CARTESIAN_POINT('Ctrl Pts',(372.102147085676,-24.3485199609737,-3.72485785076274));
#45098=CARTESIAN_POINT('Ctrl Pts',(372.21150679285,-24.3543754028254,-3.68582120918149));
#45099=CARTESIAN_POINT('Ctrl Pts',(372.318855519323,-24.3602308446771,-3.64206492500245));
#45100=CARTESIAN_POINT('Ctrl Pts',(372.426326035282,-24.3660929296561,-3.59825899835889));
#45101=CARTESIAN_POINT('Ctrl Pts',(372.53178063407,-24.3719550146351,-3.54972289777598));
#45102=CARTESIAN_POINT('Ctrl Pts',(372.634787461301,-24.377817099614,-3.49668388482455));
#45103=CARTESIAN_POINT('Ctrl Pts',(372.737863825642,-24.3836831419273,-3.44360906667695));
#45104=CARTESIAN_POINT('Ctrl Pts',(372.838488770445,-24.3895491842405,-3.38602548789292));
#45105=CARTESIAN_POINT('Ctrl Pts',(372.936258120726,-24.3954152265537,-3.32420458333332));
#45106=CARTESIAN_POINT('Ctrl Pts',(373.034170476087,-24.4012898489982,-3.26229325469496));
#45107=CARTESIAN_POINT('Ctrl Pts',(373.129218563327,-24.4071644714426,-3.19613246601103));
#45108=CARTESIAN_POINT('Ctrl Pts',(373.221029997727,-24.413039093887,-3.12603489092557));
#45109=CARTESIAN_POINT('Ctrl Pts',(373.244177591977,-24.4145202098026,-3.10836181745));
#45110=CARTESIAN_POINT('Ctrl Pts',(373.267119627545,-24.4160013257182,-3.09043868874957));
#45111=CARTESIAN_POINT('Ctrl Pts',(373.289850507784,-24.4174824416337,-3.07227088362816));
#45112=CARTESIAN_POINT('Ctrl Pts',(373.379915437798,-24.4233509605769,-3.00028589758434));
#45113=CARTESIAN_POINT('Ctrl Pts',(373.466963916202,-24.4292194795201,-2.92421591213455));
#45114=CARTESIAN_POINT('Ctrl Pts',(373.550602150184,-24.4350879984633,-2.84434326657155));
#45115=CARTESIAN_POINT('Ctrl Pts',(373.634132114576,-24.4409489206161,-2.76457401604811));
#45116=CARTESIAN_POINT('Ctrl Pts',(373.714260316684,-24.4468098427689,-2.68101217755409));
#45117=CARTESIAN_POINT('Ctrl Pts',(373.790624674593,-24.4526707649217,-2.59398129868439));
#45118=CARTESIAN_POINT('Ctrl Pts',(373.866910673734,-24.4585256730824,-2.50703972368229));
#45119=CARTESIAN_POINT('Ctrl Pts',(373.939440239106,-24.4643805812431,-2.41663649771471));
#45120=CARTESIAN_POINT('Ctrl Pts',(374.007887427826,-24.4702354894038,-2.32313261678282));
#45121=CARTESIAN_POINT('Ctrl Pts',(374.078889625628,-24.4763089506389,-2.22613840601473));
#45122=CARTESIAN_POINT('Ctrl Pts',(374.145498396162,-24.4823824118739,-2.12580785300024));
#45123=CARTESIAN_POINT('Ctrl Pts',(374.207394854622,-24.488455873109,-2.0225826417324));
#45124=CARTESIAN_POINT('Ctrl Pts',(374.266995477316,-24.4943040602351,-1.92318621385329));
#45125=CARTESIAN_POINT('Ctrl Pts',(374.32222691206,-24.5001522473612,-1.82110642942066));
#45126=CARTESIAN_POINT('Ctrl Pts',(374.372848546649,-24.5060004344873,-1.71676717457149));
#45127=CARTESIAN_POINT('Ctrl Pts',(374.423462695258,-24.5118477567775,-1.61244334952002));
#45128=CARTESIAN_POINT('Ctrl Pts',(374.469468218461,-24.5176950790676,-1.50586109073311));
#45129=CARTESIAN_POINT('Ctrl Pts',(374.510671076805,-24.5235424013577,-1.39746770104633));
#45130=CARTESIAN_POINT('Ctrl Pts',(374.55187785325,-24.5293902796868,-1.28906400391402));
#45131=CARTESIAN_POINT('Ctrl Pts',(374.588280909871,-24.535238158016,-1.17884922048234));
#45132=CARTESIAN_POINT('Ctrl Pts',(374.619735111485,-24.5410860363451,-1.06728870548844));
#45133=CARTESIAN_POINT('Ctrl Pts',(374.651199946746,-24.5469358916529,-0.955690475491368));
#45134=CARTESIAN_POINT('Ctrl Pts',(374.677712488063,-24.5527857469606,-0.842746007520911));
#45135=CARTESIAN_POINT('Ctrl Pts',(374.699178202527,-24.5586356022684,-0.728933111050087));
#45136=CARTESIAN_POINT('Ctrl Pts',(374.72066849635,-24.5644921559646,-0.614989892895866));
#45137=CARTESIAN_POINT('Ctrl Pts',(374.737100352414,-24.5703487096608,-0.500176668518449));
#45138=CARTESIAN_POINT('Ctrl Pts',(374.748430823958,-24.576205263357,-0.384978768675763));
#45139=CARTESIAN_POINT('Ctrl Pts',(374.759769000728,-24.5820657997706,-0.269702529128345));
#45140=CARTESIAN_POINT('Ctrl Pts',(374.765998863326,-24.5879263361843,-0.154041505544829));
#45141=CARTESIAN_POINT('Ctrl Pts',(374.767129590379,-24.5937868725979,-0.0384816851803687));
#45142=CARTESIAN_POINT('Ctrl Pts',(374.768261988245,-24.599656068801,0.0772488915170869));
#45143=CARTESIAN_POINT('Ctrl Pts',(374.764280227651,-24.605525265004,0.192877554481354));
#45144=CARTESIAN_POINT('Ctrl Pts',(374.755245371977,-24.6113944612071,0.307922705695058));
#45145=CARTESIAN_POINT('Ctrl Pts',(374.752882904271,-24.6129291604865,0.338005140249838));
#45146=CARTESIAN_POINT('Ctrl Pts',(374.750175209379,-24.6144638597659,0.368047730990852));
#45147=CARTESIAN_POINT('Ctrl Pts',(374.747123952468,-24.6159985590453,0.398041994923376));
#45148=CARTESIAN_POINT('Ctrl Pts',(374.735426283552,-24.6218821685148,0.513031646428155));
#45149=CARTESIAN_POINT('Ctrl Pts',(374.718636173904,-24.6277657779843,0.627693739462631));
#45150=CARTESIAN_POINT('Ctrl Pts',(374.696778725557,-24.6336493874539,0.741542318211561));
#45151=CARTESIAN_POINT('Ctrl Pts',(374.674949511691,-24.6395253967378,0.855243832419721));
#45152=CARTESIAN_POINT('Ctrl Pts',(374.648066054391,-24.6454014060217,0.968133521689445));
#45153=CARTESIAN_POINT('Ctrl Pts',(374.616205263135,-24.6512774153057,1.07972988231311));
#45154=CARTESIAN_POINT('Ctrl Pts',(374.584377195175,-24.6571473895104,1.19121162554159));
#45155=CARTESIAN_POINT('Ctrl Pts',(374.547582074684,-24.6630173637151,1.30140228899552));
#45156=CARTESIAN_POINT('Ctrl Pts',(374.505947848885,-24.6688873379198,1.40983054831438));
#45157=CARTESIAN_POINT('Ctrl Pts',(374.462910454372,-24.6749551436922,1.52191308817569));
#45158=CARTESIAN_POINT('Ctrl Pts',(374.414702094429,-24.6810229494646,1.6321118898979));
#45159=CARTESIAN_POINT('Ctrl Pts',(374.361520288645,-24.687090755237,1.73992298092849));
#45160=CARTESIAN_POINT('Ctrl Pts',(374.310132589878,-24.6929538614367,1.84409702669276));
#45161=CARTESIAN_POINT('Ctrl Pts',(374.254101795052,-24.6988169676364,1.94604146672834));
#45162=CARTESIAN_POINT('Ctrl Pts',(374.193654735131,-24.7046800738362,2.04532264297282));
#45163=CARTESIAN_POINT('Ctrl Pts',(374.13321741465,-24.7105422353519,2.14458782269084));
#45164=CARTESIAN_POINT('Ctrl Pts',(374.068365458107,-24.7164043968677,2.24119024048417));
#45165=CARTESIAN_POINT('Ctrl Pts',(373.999370619686,-24.7222665583835,2.33472267850232));
#45166=CARTESIAN_POINT('Ctrl Pts',(373.930370362768,-24.728129180283,2.42826246207226));
#45167=CARTESIAN_POINT('Ctrl Pts',(373.857226821597,-24.7339918021825,2.51873145534644));
#45168=CARTESIAN_POINT('Ctrl Pts',(373.78025344888,-24.739854424082,2.60575372325304));
#45169=CARTESIAN_POINT('Ctrl Pts',(373.703255583957,-24.7457189114129,2.69280368083081));
#45170=CARTESIAN_POINT('Ctrl Pts',(373.622425736794,-24.7515833987438,2.77640442399754));
#45171=CARTESIAN_POINT('Ctrl Pts',(373.538115300845,-24.7574478860747,2.85621574154327));
#45172=CARTESIAN_POINT('Ctrl Pts',(373.45371199277,-24.7633188334292,2.93611497521268));
#45173=CARTESIAN_POINT('Ctrl Pts',(373.365820742306,-24.7691897807837,3.01221616835958));
#45174=CARTESIAN_POINT('Ctrl Pts',(373.274827279402,-24.7750607281382,3.08421833545199));
#45175=CARTESIAN_POINT('Ctrl Pts',(373.183773975019,-24.7809355364972,3.15626785447475));
#45176=CARTESIAN_POINT('Ctrl Pts',(373.089614728311,-24.7868103448562,3.22421273865896));
#45177=CARTESIAN_POINT('Ctrl Pts',(372.992764187068,-24.7926851532151,3.28779537439818));
#45178=CARTESIAN_POINT('Ctrl Pts',(372.895775611393,-24.7985683345355,3.35146863010644));
#45179=CARTESIAN_POINT('Ctrl Pts',(372.796088438266,-24.8044515158558,3.41076701919639));
#45180=CARTESIAN_POINT('Ctrl Pts',(372.694141866626,-24.8103346971761,3.46547884702414));
#45181=CARTESIAN_POINT('Ctrl Pts',(372.669997641815,-24.8117280236031,3.47843636633704));
#45182=CARTESIAN_POINT('Ctrl Pts',(372.645726774633,-24.81312135003,3.49113684132792));
#45183=CARTESIAN_POINT('Ctrl Pts',(372.62133524988,-24.814514676457,3.50357786042328));
#45184=CARTESIAN_POINT('Ctrl Pts',(372.519529775596,-24.8203301496251,3.55550425134935));
#45185=CARTESIAN_POINT('Ctrl Pts',(372.415275008324,-24.8261456227933,3.60308336030811));
#45186=CARTESIAN_POINT('Ctrl Pts',(372.308982646098,-24.8319610959615,3.64607360713652));
#45187=CARTESIAN_POINT('Ctrl Pts',(372.202826302923,-24.8377691272484,3.6890088406751));
#45188=CARTESIAN_POINT('Ctrl Pts',(372.094637935516,-24.8435771585353,3.72736672841206));
#45189=CARTESIAN_POINT('Ctrl Pts',(371.984854025107,-24.8493851898223,3.760951411171));
#45190=CARTESIAN_POINT('Ctrl Pts',(371.875179831196,-24.8551874166443,3.79450252986967));
#45191=CARTESIAN_POINT('Ctrl Pts',(371.763913665966,-24.8609896434664,3.82328980564147));
#45192=CARTESIAN_POINT('Ctrl Pts',(371.651511457012,-24.8667918702884,3.8471656597979));
#45193=CARTESIAN_POINT('Ctrl Pts',(371.539187024154,-24.8725900822912,3.87102499318718));
#45194=CARTESIAN_POINT('Ctrl Pts',(371.425728522169,-24.878388294294,3.88997957516185));
#45195=CARTESIAN_POINT('Ctrl Pts',(371.311605765081,-24.8841865062969,3.90393202415144));
#45196=CARTESIAN_POINT('Ctrl Pts',(371.197523572533,-24.8899826573452,3.91787951379123));
#45197=CARTESIAN_POINT('Ctrl Pts',(371.082778012525,-24.8957788083936,3.92682835261829));
#45198=CARTESIAN_POINT('Ctrl Pts',(370.96784708384,-24.901574959442,3.93073262186212));
#45199=CARTESIAN_POINT('Ctrl Pts',(370.85292786991,-24.9073705196966,3.93463649314905));
#45200=CARTESIAN_POINT('Ctrl Pts',(370.737823746668,-24.9131660799511,3.93349680303252));
#45201=CARTESIAN_POINT('Ctrl Pts',(370.623014968402,-24.9189616402056,3.92731970825724));
#45202=CARTESIAN_POINT('Ctrl Pts',(370.508188785343,-24.924758079056,3.92114167704619));
#45203=CARTESIAN_POINT('Ctrl Pts',(370.393658457635,-24.9305545179064,3.90992474698988));
#45204=CARTESIAN_POINT('Ctrl Pts',(370.279900534571,-24.9363509567568,3.89372706244001));
#45205=CARTESIAN_POINT('Ctrl Pts',(370.166029974372,-24.9421531349372,3.87751333979161));
#45206=CARTESIAN_POINT('Ctrl Pts',(370.052933764254,-24.9479553131176,3.85630907571423));
#45207=CARTESIAN_POINT('Ctrl Pts',(369.941079656376,-24.9537574912981,3.83022382161817));
#45208=CARTESIAN_POINT('Ctrl Pts',(369.82916584053,-24.9595627666939,3.80412464315652));
#45209=CARTESIAN_POINT('Ctrl Pts',(369.718495852986,-24.9653680420897,3.7731394012963));
#45210=CARTESIAN_POINT('Ctrl Pts',(369.609521853363,-24.9711733174855,3.73742742521155));
#45211=CARTESIAN_POINT('Ctrl Pts',(369.500382321148,-24.9769874111524,3.70166120227943));
#45212=CARTESIAN_POINT('Ctrl Pts',(369.392944315382,-24.9828015048194,3.66115405719538));
#45213=CARTESIAN_POINT('Ctrl Pts',(369.287639788638,-24.9886155984863,3.61611337827333));
#45214=CARTESIAN_POINT('Ctrl Pts',(369.219366291571,-24.9923851278616,3.58691155043805));
#45215=CARTESIAN_POINT('Ctrl Pts',(369.151989131291,-24.9961546572369,3.5558050141533));
#45216=CARTESIAN_POINT('Ctrl Pts',(369.0856199232,-24.9999241866122,3.52286027959241));
#45217=CARTESIAN_POINT('',(372.583012328556,-25.,3.52286199445081));
#45218=CARTESIAN_POINT('Origin',(370.834317853224,-25.,0.));
#45219=CARTESIAN_POINT('',(366.902348364549,-24.1541640165523,-0.00373514424167985));
#45220=CARTESIAN_POINT('Ctrl Pts',(372.583012328555,-25.,3.52286199445091));
#45221=CARTESIAN_POINT('Ctrl Pts',(373.754775930706,-24.9338279608628,2.94121657640655));
#45222=CARTESIAN_POINT('Ctrl Pts',(375.451192048449,-24.8014838825885,0.524644555208875));
#45223=CARTESIAN_POINT('Ctrl Pts',(373.777719574704,-24.6029677651766,-3.60213327029863));
#45224=CARTESIAN_POINT('Ctrl Pts',(369.40332532051,-24.4044516477652,-4.42278112563621));
#45225=CARTESIAN_POINT('Ctrl Pts',(367.096283649816,-24.2548503982235,-1.99166067173424));
#45226=CARTESIAN_POINT('Ctrl Pts',(366.899312227999,-24.1714211878193,-0.345061147376345));
#45227=CARTESIAN_POINT('Ctrl Pts',(366.902348364549,-24.1541640165523,-0.00373514424167984));
#45228=CARTESIAN_POINT('',(366.901318041952,-22.9041635220074,0.00121841432566519));
#45229=CARTESIAN_POINT('Ctrl Pts',(366.901319618492,-24.154163522035,-0.00372633806003078));
#45230=CARTESIAN_POINT('Ctrl Pts',(366.901211040247,-24.1483709030749,0.110873582393982));
#45231=CARTESIAN_POINT('Ctrl Pts',(366.906115515684,-24.1425782841149,0.225595340395165));
#45232=CARTESIAN_POINT('Ctrl Pts',(366.916038151957,-24.1367856651548,0.33996056042058));
#45233=CARTESIAN_POINT('Ctrl Pts',(366.925955279232,-24.1309962622284,0.454262285436717));
#45234=CARTESIAN_POINT('Ctrl Pts',(366.940884993294,-24.125206859302,0.568207445362342));
#45235=CARTESIAN_POINT('Ctrl Pts',(366.960780336364,-24.1194174563756,0.681319385807697));
#45236=CARTESIAN_POINT('Ctrl Pts',(366.980670394066,-24.1136295914535,0.794401277099489));
#45237=CARTESIAN_POINT('Ctrl Pts',(367.005523386089,-24.1078417265315,0.906649972262003));
#45238=CARTESIAN_POINT('Ctrl Pts',(367.035240796864,-24.1020538616094,1.01759644252616));
#45239=CARTESIAN_POINT('Ctrl Pts',(367.064957886073,-24.0962660593168,1.12854171225819));
#45240=CARTESIAN_POINT('Ctrl Pts',(367.099539179392,-24.0904782570242,1.23818437640287));
#45241=CARTESIAN_POINT('Ctrl Pts',(367.138835807161,-24.0846904547317,1.34606888650933));
#45242=CARTESIAN_POINT('Ctrl Pts',(367.178142024708,-24.078901240009,1.45397972428082));
#45243=CARTESIAN_POINT('Ctrl Pts',(367.222165718138,-24.0731120252864,1.5601311580188));
#45244=CARTESIAN_POINT('Ctrl Pts',(367.270709548455,-24.0673228105638,1.66408679166055));
#45245=CARTESIAN_POINT('Ctrl Pts',(367.319305922783,-24.0615273295749,1.76815494724423));
#45246=CARTESIAN_POINT('Ctrl Pts',(367.372432019966,-24.055731848586,1.87002217515476));
#45247=CARTESIAN_POINT('Ctrl Pts',(367.429844131953,-24.0499363675972,1.96927592814549));
#45248=CARTESIAN_POINT('Ctrl Pts',(367.487291682565,-24.0441373092467,2.06859094724314));
#45249=CARTESIAN_POINT('Ctrl Pts',(367.549030285807,-24.0383382508963,2.16528892502502));
#45250=CARTESIAN_POINT('Ctrl Pts',(367.614773482489,-24.0325391925459,2.25898717235545));
#45251=CARTESIAN_POINT('Ctrl Pts',(367.680616649138,-24.0267313160712,2.35282789846979));
#45252=CARTESIAN_POINT('Ctrl Pts',(367.75047630523,-24.0209234395966,2.44365945622849));
#45253=CARTESIAN_POINT('Ctrl Pts',(367.824026372663,-24.015115563122,2.53113298782669));
#45254=CARTESIAN_POINT('Ctrl Pts',(367.856513999148,-24.0125501797286,2.56977071476638));
#45255=CARTESIAN_POINT('Ctrl Pts',(367.889721171392,-24.0099847963352,2.60775376482483));
#45256=CARTESIAN_POINT('Ctrl Pts',(367.923617651581,-24.0074194129418,2.64505450532738));
#45257=CARTESIAN_POINT('Ctrl Pts',(368.001233225964,-24.001545242394,2.73046509613132));
#45258=CARTESIAN_POINT('Ctrl Pts',(368.082740585547,-23.9956710718462,2.81259869280454));
#45259=CARTESIAN_POINT('Ctrl Pts',(368.167832125766,-23.9897969012984,2.89107987874132));
#45260=CARTESIAN_POINT('Ctrl Pts',(368.252813755781,-23.9839303182415,2.96945969287133));
#45261=CARTESIAN_POINT('Ctrl Pts',(368.341370058817,-23.9780637351846,3.04419620078266));
#45262=CARTESIAN_POINT('Ctrl Pts',(368.433154352334,-23.9721971521277,3.11494828881526));
#45263=CARTESIAN_POINT('Ctrl Pts',(368.524844595914,-23.9663365804671,3.18562787828477));
#45264=CARTESIAN_POINT('Ctrl Pts',(368.619755925512,-23.9604760088065,3.25233091819105));
#45265=CARTESIAN_POINT('Ctrl Pts',(368.71750660987,-23.9546154371459,3.31475476619477));
#45266=CARTESIAN_POINT('Ctrl Pts',(368.818772766051,-23.9485440979119,3.3794236038904));
#45267=CARTESIAN_POINT('Ctrl Pts',(368.923086016428,-23.9424727586779,3.43949935932853));
#45268=CARTESIAN_POINT('Ctrl Pts',(369.029986329454,-23.9364014194439,3.49469265491671));
#45269=CARTESIAN_POINT('Ctrl Pts',(369.133056728276,-23.9305475978926,3.54790854201389));
#45270=CARTESIAN_POINT('Ctrl Pts',(369.238531598795,-23.9246937763412,3.59658560823897));
#45271=CARTESIAN_POINT('Ctrl Pts',(369.345971937449,-23.9188399547899,3.64051032617621));
#45272=CARTESIAN_POINT('Ctrl Pts',(369.453396031117,-23.9129870183367,3.68442840269325));
#45273=CARTESIAN_POINT('Ctrl Pts',(369.562784619767,-23.9071340818835,3.72359540341856));
#45274=CARTESIAN_POINT('Ctrl Pts',(369.673678284574,-23.9012811454303,3.75784576475462));
#45275=CARTESIAN_POINT('Ctrl Pts',(369.784581987966,-23.8954276791435,3.79209922658462));
#45276=CARTESIAN_POINT('Ctrl Pts',(369.896990643664,-23.8895742128567,3.82143504235808));
#45277=CARTESIAN_POINT('Ctrl Pts',(370.010429907833,-23.8837207465699,3.84573759549974));
#45278=CARTESIAN_POINT('Ctrl Pts',(370.123906862006,-23.8778653354788,3.87004822312337));
#45279=CARTESIAN_POINT('Ctrl Pts',(370.238414701848,-23.8720099243878,3.88932217634726));
#45280=CARTESIAN_POINT('Ctrl Pts',(370.353469839863,-23.8661545132968,3.90349512463473));
#45281=CARTESIAN_POINT('Ctrl Pts',(370.468655110893,-23.8602924794481,3.917684103223));
#45282=CARTESIAN_POINT('Ctrl Pts',(370.584388505427,-23.8544304455994,3.92676051077787));
#45283=CARTESIAN_POINT('Ctrl Pts',(370.700182174666,-23.8485684117508,3.93071197364267));
#45284=CARTESIAN_POINT('Ctrl Pts',(370.816053777859,-23.8427024325097,3.93466609600625));
#45285=CARTESIAN_POINT('Ctrl Pts',(370.931985324504,-23.8368364532685,3.93348840949058));
#45286=CARTESIAN_POINT('Ctrl Pts',(371.047491567142,-23.8309704740274,3.92721860452079));
#45287=CARTESIAN_POINT('Ctrl Pts',(371.163166426168,-23.8250959316108,3.92093964686941));
#45288=CARTESIAN_POINT('Ctrl Pts',(371.278414332609,-23.8192213891941,3.90955377580453));
#45289=CARTESIAN_POINT('Ctrl Pts',(371.392757661741,-23.8133468467775,3.89315219073992));
#45290=CARTESIAN_POINT('Ctrl Pts',(371.421587733758,-23.8118656630284,3.88901676034632));
#45291=CARTESIAN_POINT('Ctrl Pts',(371.450360364779,-23.8103844792792,3.8845627185368));
#45292=CARTESIAN_POINT('Ctrl Pts',(371.479068043468,-23.80890329553,3.87979202950115));
#45293=CARTESIAN_POINT('Ctrl Pts',(371.592926779711,-23.8030287101393,3.86087079833835));
#45294=CARTESIAN_POINT('Ctrl Pts',(371.706140862762,-23.7971541247486,3.83690186711168));
#45295=CARTESIAN_POINT('Ctrl Pts',(371.818228011975,-23.7912795393579,3.80794036186305));
#45296=CARTESIAN_POINT('Ctrl Pts',(371.930170779619,-23.7854125211314,3.77901616247521));
#45297=CARTESIAN_POINT('Ctrl Pts',(372.040989104025,-23.7795455029048,3.74511228076714));
#45298=CARTESIAN_POINT('Ctrl Pts',(372.150208364254,-23.7736784846783,3.70633527395741));
#45299=CARTESIAN_POINT('Ctrl Pts',(372.259316084241,-23.767817458148,3.66759786819163));
#45300=CARTESIAN_POINT('Ctrl Pts',(372.366827601449,-23.7619564316177,3.62399737380741));
#45301=CARTESIAN_POINT('Ctrl Pts',(372.472281640284,-23.7560954050875,3.57569065108807));
#45302=CARTESIAN_POINT('Ctrl Pts',(372.581516778433,-23.7500242289637,3.52565187032618));
#45303=CARTESIAN_POINT('Ctrl Pts',(372.688543688626,-23.74395305284,3.4705631527276));
#45304=CARTESIAN_POINT('Ctrl Pts',(372.792869968271,-23.7378818767163,3.4106542792613));
#45305=CARTESIAN_POINT('Ctrl Pts',(372.893469871702,-23.7320275537803,3.35288525974034));
#45306=CARTESIAN_POINT('Ctrl Pts',(372.991558381076,-23.7261732308443,3.29063475531567));
#45307=CARTESIAN_POINT('Ctrl Pts',(373.086718083544,-23.7203189079082,3.22415604499136));
#45308=CARTESIAN_POINT('Ctrl Pts',(373.18186366578,-23.7144654536634,3.15768719908175));
#45309=CARTESIAN_POINT('Ctrl Pts',(373.274080966771,-23.7086119994185,3.08699163124631));
#45310=CARTESIAN_POINT('Ctrl Pts',(373.362981823317,-23.7027585451737,3.01236576901852));
#45311=CARTESIAN_POINT('Ctrl Pts',(373.451890968636,-23.6969045451753,2.93773294896269));
#45312=CARTESIAN_POINT('Ctrl Pts',(373.537482738475,-23.6910505451769,2.85916937158491));
#45313=CARTESIAN_POINT('Ctrl Pts',(373.619402860261,-23.6851965451785,2.77701107372275));
#45314=CARTESIAN_POINT('Ctrl Pts',(373.701350413512,-23.6793405849316,2.69482526464086));
#45315=CARTESIAN_POINT('Ctrl Pts',(373.779623582479,-23.6734846246847,2.60904263381188));
#45316=CARTESIAN_POINT('Ctrl Pts',(373.853906188467,-23.6676286644378,2.52003477866117));
#45317=CARTESIAN_POINT('Ctrl Pts',(373.928273060669,-23.6617660611877,2.43092595296979));
#45318=CARTESIAN_POINT('Ctrl Pts',(373.998640069694,-23.6559034579375,2.33858491766555));
#45319=CARTESIAN_POINT('Ctrl Pts',(374.064732393004,-23.6500408546873,2.24341500868123));
#45320=CARTESIAN_POINT('Ctrl Pts',(374.130869335962,-23.6441742935299,2.14818084945474));
#45321=CARTESIAN_POINT('Ctrl Pts',(374.192725626933,-23.6383077323724,2.05011436212437));
#45322=CARTESIAN_POINT('Ctrl Pts',(374.250071609165,-23.6324411712149,1.94964491094506));
#45323=CARTESIAN_POINT('Ctrl Pts',(374.307501433047,-23.6265660329584,1.84902857023195));
#45324=CARTESIAN_POINT('Ctrl Pts',(374.360407599833,-23.6206908947019,1.74600262014703));
#45325=CARTESIAN_POINT('Ctrl Pts',(374.408607872484,-23.6148157564454,1.641017933546));
#45326=CARTESIAN_POINT('Ctrl Pts',(374.420718718419,-23.6133395636698,1.61463938224214));
#45327=CARTESIAN_POINT('Ctrl Pts',(374.432532715833,-23.6118633708941,1.58813725214939));
#45328=CARTESIAN_POINT('Ctrl Pts',(374.444047468922,-23.6103871781184,1.56151884444309));
#45329=CARTESIAN_POINT('Ctrl Pts',(374.489859508578,-23.6045140689465,1.4556161351097));
#45330=CARTESIAN_POINT('Ctrl Pts',(374.531083565184,-23.5986409597746,1.34751893434641));
#45331=CARTESIAN_POINT('Ctrl Pts',(374.567504376343,-23.5927678506027,1.23766206357107));
#45332=CARTESIAN_POINT('Ctrl Pts',(374.603878113192,-23.5869023324907,1.12794718404289));
#45333=CARTESIAN_POINT('Ctrl Pts',(374.635460821849,-23.5810368143788,1.01647754615335));
#45334=CARTESIAN_POINT('Ctrl Pts',(374.662084596016,-23.5751712962669,0.903709445991489));
#45335=CARTESIAN_POINT('Ctrl Pts',(374.688681074097,-23.5693117917908,0.791056961582879));
#45336=CARTESIAN_POINT('Ctrl Pts',(374.71032863606,-23.5634522873148,0.677109062643));
#45337=CARTESIAN_POINT('Ctrl Pts',(374.726908870607,-23.5575927828387,0.562338129054325));
#45338=CARTESIAN_POINT('Ctrl Pts',(374.744089648872,-23.5515210444166,0.443410139483239));
#45339=CARTESIAN_POINT('Ctrl Pts',(374.7558289184,-23.5454493059944,0.323598792791398));
#45340=CARTESIAN_POINT('Ctrl Pts',(374.762052576321,-23.5393775675722,0.203442731438583));
#45341=CARTESIAN_POINT('Ctrl Pts',(374.768051772455,-23.5335248118243,0.0876202058567169));
#45342=CARTESIAN_POINT('Ctrl Pts',(374.768926310938,-23.5276720560764,-0.0285221508597304));
#45343=CARTESIAN_POINT('Ctrl Pts',(374.764662591531,-23.5218193003285,-0.144496498450968));
#45344=CARTESIAN_POINT('Ctrl Pts',(374.760399515183,-23.5159674273001,-0.260453354655197));
#45345=CARTESIAN_POINT('Ctrl Pts',(374.750999737023,-23.5101155542717,-0.376241839268233));
#45346=CARTESIAN_POINT('Ctrl Pts',(374.7365017716,-23.5042636812433,-0.491375281397875));
#45347=CARTESIAN_POINT('Ctrl Pts',(374.722002484717,-23.4984112748287,-0.606519217703132));
#45348=CARTESIAN_POINT('Ctrl Pts',(374.702404138451,-23.4925588684142,-0.721007582811191));
#45349=CARTESIAN_POINT('Ctrl Pts',(374.677796905732,-23.4867064619996,-0.834360697140713));
#45350=CARTESIAN_POINT('Ctrl Pts',(374.653181475933,-23.4808521060508,-0.947751571284607));
#45351=CARTESIAN_POINT('Ctrl Pts',(374.623553929497,-23.4749977501019,-1.06000603906158));
#45352=CARTESIAN_POINT('Ctrl Pts',(374.589054975105,-23.4691433941531,-1.17065714261912));
#45353=CARTESIAN_POINT('Ctrl Pts',(374.554516920495,-23.4632824030292,-1.28143365526499));
#45354=CARTESIAN_POINT('Ctrl Pts',(374.515096561176,-23.4574214119053,-1.39060278192006));
#45355=CARTESIAN_POINT('Ctrl Pts',(374.47098369848,-23.4515604207814,-1.49771510306407));
#45356=CARTESIAN_POINT('Ctrl Pts',(374.426841095714,-23.4456954782865,-1.60489963733956));
#45357=CARTESIAN_POINT('Ctrl Pts',(374.377999863869,-23.4398305357916,-1.71002423113383));
#45358=CARTESIAN_POINT('Ctrl Pts',(374.324696163445,-23.4339655932967,-1.81266330341204));
#45359=CARTESIAN_POINT('Ctrl Pts',(374.271314483747,-23.4280920708354,-1.91545252887505));
#45360=CARTESIAN_POINT('Ctrl Pts',(374.213457512432,-23.422218548374,-2.01574861945833));
#45361=CARTESIAN_POINT('Ctrl Pts',(374.151405192807,-23.4163450259127,-2.1131541783731));
#45362=CARTESIAN_POINT('Ctrl Pts',(374.135649745613,-23.4148537041774,-2.13788601997338));
#45363=CARTESIAN_POINT('Ctrl Pts',(374.119624035791,-23.4133623824421,-2.16243167915984));
#45364=CARTESIAN_POINT('Ctrl Pts',(374.103333052733,-23.4118710607068,-2.18678499752064));
#45365=CARTESIAN_POINT('Ctrl Pts',(374.039168680047,-23.4059972762164,-2.28270403382942));
#45366=CARTESIAN_POINT('Ctrl Pts',(373.970672218861,-23.400123491726,-2.37595634356408));
#45367=CARTESIAN_POINT('Ctrl Pts',(373.898092499842,-23.3942497072356,-2.46612528366739));
#45368=CARTESIAN_POINT('Ctrl Pts',(373.82560648435,-23.3883835060527,-2.55617781180404));
#45369=CARTESIAN_POINT('Ctrl Pts',(373.74904795132,-23.3825173048699,-2.64315456786081));
#45370=CARTESIAN_POINT('Ctrl Pts',(373.668709442221,-23.376651103687,-2.7266670717601));
#45371=CARTESIAN_POINT('Ctrl Pts',(373.588453196589,-23.370790909263,-2.81009406214707));
#45372=CARTESIAN_POINT('Ctrl Pts',(373.504424958444,-23.3649307148389,-2.89006356021101));
#45373=CARTESIAN_POINT('Ctrl Pts',(373.416957609282,-23.3590705204149,-2.96621996662902));
#45374=CARTESIAN_POINT('Ctrl Pts',(373.326336645055,-23.3529990380349,-3.04512217468414));
#45375=CARTESIAN_POINT('Ctrl Pts',(373.232024180959,-23.3469275556549,-3.11993079081061));
#45376=CARTESIAN_POINT('Ctrl Pts',(373.134432603918,-23.3408560732749,-3.19029170039991));
#45377=CARTESIAN_POINT('Ctrl Pts',(373.040345492086,-23.3350026148209,-3.25812598456511));
#45378=CARTESIAN_POINT('Ctrl Pts',(372.943211083313,-23.3291491563668,-3.32182623581534));
#45379=CARTESIAN_POINT('Ctrl Pts',(372.843432051197,-23.3232956979128,-3.3811165521914));
#45380=CARTESIAN_POINT('Ctrl Pts',(372.743668006188,-23.3174431186656,-3.44039796298622));
#45381=CARTESIAN_POINT('Ctrl Pts',(372.641260482743,-23.3115905394184,-3.49527054499489));
#45382=CARTESIAN_POINT('Ctrl Pts',(372.53663941868,-23.3057379601712,-3.5455028258041));
#45383=CARTESIAN_POINT('Ctrl Pts',(372.432008770451,-23.2998848447787,-3.595739708311));
#45384=CARTESIAN_POINT('Ctrl Pts',(372.325164550945,-23.2940317293862,-3.64133526575361));
#45385=CARTESIAN_POINT('Ctrl Pts',(372.21655882358,-23.2881786139937,-3.68210522661568));
#45386=CARTESIAN_POINT('Ctrl Pts',(372.107916884977,-23.28232354706,-3.72288878096662));
#45387=CARTESIAN_POINT('Ctrl Pts',(371.99751265722,-23.2764684801262,-3.75884339430151));
#45388=CARTESIAN_POINT('Ctrl Pts',(371.885814906657,-23.2706134131925,-3.78983415819493));
#45389=CARTESIAN_POINT('Ctrl Pts',(371.77399058791,-23.2647517117009,-3.82086003868378));
#45390=CARTESIAN_POINT('Ctrl Pts',(371.66087021916,-23.2588900102093,-3.84691073266935));
#45391=CARTESIAN_POINT('Ctrl Pts',(371.546934440917,-23.2530283087177,-3.86790209272996));
#45392=CARTESIAN_POINT('Ctrl Pts',(371.432921848747,-23.247162655348,-3.88890760487548));
#45393=CARTESIAN_POINT('Ctrl Pts',(371.318093160626,-23.2412970019783,-3.90484693450206));
#45394=CARTESIAN_POINT('Ctrl Pts',(371.202934117157,-23.2354313486085,-3.91568781313882));
#45395=CARTESIAN_POINT('Ctrl Pts',(371.087606718133,-23.2295571200084,-3.92654454048432));
#45396=CARTESIAN_POINT('Ctrl Pts',(370.97194841093,-23.2236828914082,-3.93228792085756));
#45397=CARTESIAN_POINT('Ctrl Pts',(370.856444988247,-23.2178086628081,-3.93293775565997));
#45398=CARTESIAN_POINT('Ctrl Pts',(370.827254213739,-23.2163240896371,-3.93310198612816));
#45399=CARTESIAN_POINT('Ctrl Pts',(370.798073303989,-23.2148395164661,-3.93294114682943));
#45400=CARTESIAN_POINT('Ctrl Pts',(370.768910031146,-23.2133549432951,-3.93245607945098));
#45401=CARTESIAN_POINT('Ctrl Pts',(370.653524345242,-23.2074811686151,-3.93053689046032));
#45402=CARTESIAN_POINT('Ctrl Pts',(370.538031092616,-23.2016073939351,-3.9235317517467));
#45403=CARTESIAN_POINT('Ctrl Pts',(370.422915275364,-23.1957336192552,-3.91142389916133));
#45404=CARTESIAN_POINT('Ctrl Pts',(370.307948048513,-23.1898674263876,-3.89933167527679));
#45405=CARTESIAN_POINT('Ctrl Pts',(370.193357695288,-23.18400123352,-3.8821498788094));
#45406=CARTESIAN_POINT('Ctrl Pts',(370.079629247252,-23.1781350406525,-3.85991374359787));
#45407=CARTESIAN_POINT('Ctrl Pts',(369.966017223771,-23.1722748530449,-3.8377003716631));
#45408=CARTESIAN_POINT('Ctrl Pts',(369.85326575348,-23.1664146654373,-3.81044303162838));
#45409=CARTESIAN_POINT('Ctrl Pts',(369.741854105687,-23.1605544778296,-3.77822868025699));
#45410=CARTESIAN_POINT('Ctrl Pts',(369.626425343137,-23.1544829923319,-3.74485279192934));
#45411=CARTESIAN_POINT('Ctrl Pts',(369.512435294055,-23.1484115068341,-3.70615572923897));
#45412=CARTESIAN_POINT('Ctrl Pts',(369.400405081633,-23.1423400213364,-3.66229206419552));
#45413=CARTESIAN_POINT('Ctrl Pts',(369.292397929558,-23.1364865658862,-3.62000356506178));
#45414=CARTESIAN_POINT('Ctrl Pts',(369.186212695366,-23.1306331104361,-3.57291331529551));
#45415=CARTESIAN_POINT('Ctrl Pts',(369.082299511122,-23.1247796549859,-3.52121012280412));
#45416=CARTESIAN_POINT('Ctrl Pts',(368.978401909709,-23.1189270773205,-3.46951468372823));
#45417=CARTESIAN_POINT('Ctrl Pts',(368.876776050546,-23.113074499655,-3.41320786138786));
#45418=CARTESIAN_POINT('Ctrl Pts',(368.777849510401,-23.1072219219896,-3.35252545925701));
#45419=CARTESIAN_POINT('Ctrl Pts',(368.678913883569,-23.101368806748,-3.29183748327281));
#45420=CARTESIAN_POINT('Ctrl Pts',(368.582678420814,-23.0955156915065,-3.2267733445655));
#45421=CARTESIAN_POINT('Ctrl Pts',(368.489543029175,-23.0896625762649,-3.15761302640246));
#45422=CARTESIAN_POINT('Ctrl Pts',(368.396376561482,-23.0838075080416,-3.08842963183652));
#45423=CARTESIAN_POINT('Ctrl Pts',(368.306312553243,-23.0779524398182,-3.01514758625118));
#45424=CARTESIAN_POINT('Ctrl Pts',(368.219718485244,-23.0720973715948,-2.93808766801781));
#45425=CARTESIAN_POINT('Ctrl Pts',(368.133026263153,-23.0662356666708,-2.86094040261986));
#45426=CARTESIAN_POINT('Ctrl Pts',(368.049812140463,-23.0603739617468,-2.78000699234342));
#45427=CARTESIAN_POINT('Ctrl Pts',(367.970407379493,-23.0545122568227,-2.69564571085522));
#45428=CARTESIAN_POINT('Ctrl Pts',(367.890949067956,-23.0486465987652,-2.6112275361234));
#45429=CARTESIAN_POINT('Ctrl Pts',(367.815305502559,-23.0427809407077,-2.52337719924941));
#45430=CARTESIAN_POINT('Ctrl Pts',(367.743767115392,-23.0369152826502,-2.4324853826663));
#45431=CARTESIAN_POINT('Ctrl Pts',(367.672124121428,-23.0310410475515,-2.34146065979118));
#45432=CARTESIAN_POINT('Ctrl Pts',(367.604598525725,-23.0251668124527,-2.24738591565487));
#45433=CARTESIAN_POINT('Ctrl Pts',(367.541437033318,-23.0192925773539,-2.15068010310603));
#45434=CARTESIAN_POINT('Ctrl Pts',(367.525474354209,-23.0178079935305,-2.12623983428272));
#45435=CARTESIAN_POINT('Ctrl Pts',(367.50979018446,-23.016323409707,-2.1016316320158));
#45436=CARTESIAN_POINT('Ctrl Pts',(367.494388030071,-23.0148388258835,-2.07686248375052));
#45437=CARTESIAN_POINT('Ctrl Pts',(367.431746748682,-23.0088009541236,-1.97612520070657));
#45438=CARTESIAN_POINT('Ctrl Pts',(367.373574834104,-23.0027630823638,-1.87240387406079));
#45439=CARTESIAN_POINT('Ctrl Pts',(367.320159377181,-22.9967252106039,-1.76611981622393));
#45440=CARTESIAN_POINT('Ctrl Pts',(367.266825227544,-22.9906965294975,-1.65999754054877));
#45441=CARTESIAN_POINT('Ctrl Pts',(367.218233294385,-22.9846678483911,-1.5513206366528));
#45442=CARTESIAN_POINT('Ctrl Pts',(367.174626820583,-22.9786391672847,-1.44053828328386));
#45443=CARTESIAN_POINT('Ctrl Pts',(367.129735571898,-22.9724328635139,-1.32649195618223));
#45444=CARTESIAN_POINT('Ctrl Pts',(367.0901283489,-22.9662265597431,-1.21021451682593));
#45445=CARTESIAN_POINT('Ctrl Pts',(367.056019779913,-22.9600202559723,-1.09222372672062));
#45446=CARTESIAN_POINT('Ctrl Pts',(367.022980401753,-22.9540084992981,-0.977931557645554));
#45447=CARTESIAN_POINT('Ctrl Pts',(366.995100256272,-22.9479967426239,-0.862032241019598));
#45448=CARTESIAN_POINT('Ctrl Pts',(366.972525565224,-22.9419849859498,-0.745016324883455));
#45449=CARTESIAN_POINT('Ctrl Pts',(366.948855061212,-22.9356814086307,-0.622320261999813));
#45450=CARTESIAN_POINT('Ctrl Pts',(366.931018180592,-22.9293778313115,-0.498396867271249));
#45451=CARTESIAN_POINT('Ctrl Pts',(366.919124201177,-22.9230742539924,-0.373828392409864));
#45452=CARTESIAN_POINT('Ctrl Pts',(366.907230221762,-22.9167706766733,-0.249259917548461));
#45453=CARTESIAN_POINT('Ctrl Pts',(366.901279235717,-22.9104670993541,-0.12404684158491));
#45454=CARTESIAN_POINT('Ctrl Pts',(366.901318041952,-22.904163522035,0.00121841377663275));
#45455=CARTESIAN_POINT('',(366.901318968034,-21.6541635220757,0.00296126550371377));
#45456=CARTESIAN_POINT('Ctrl Pts',(366.901318041952,-22.9041635220074,0.00121841432564433));
#45457=CARTESIAN_POINT('Ctrl Pts',(366.901356814938,-22.8978653482165,0.126376290286846));
#45458=CARTESIAN_POINT('Ctrl Pts',(366.907374045914,-22.8915671744257,0.251362841332967));
#45459=CARTESIAN_POINT('Ctrl Pts',(366.919295671331,-22.8852690006348,0.375619908000912));
#45460=CARTESIAN_POINT('Ctrl Pts',(366.931264251033,-22.8789460209772,0.500366371174498));
#45461=CARTESIAN_POINT('Ctrl Pts',(366.94918373839,-22.8726230413195,0.624377293027341));
#45462=CARTESIAN_POINT('Ctrl Pts',(366.972928461376,-22.8663000616618,0.74710170962471));
#45463=CARTESIAN_POINT('Ctrl Pts',(366.996721025578,-22.8599643423721,0.870073393174389));
#45464=CARTESIAN_POINT('Ctrl Pts',(367.026362194002,-22.8536286230824,0.99175309786698));
#45465=CARTESIAN_POINT('Ctrl Pts',(367.06167635572,-22.8472929037927,1.11160475498688));
#45466=CARTESIAN_POINT('Ctrl Pts',(367.097101549305,-22.8409372642584,1.23183323977499));
#45467=CARTESIAN_POINT('Ctrl Pts',(367.138235322381,-22.8345816247241,1.3502218874582));
#45468=CARTESIAN_POINT('Ctrl Pts',(367.184852995517,-22.8282259851898,1.46625211077756));
#45469=CARTESIAN_POINT('Ctrl Pts',(367.213955918482,-22.8242582262838,1.53868855866898));
#45470=CARTESIAN_POINT('Ctrl Pts',(367.245195188944,-22.8202904673778,1.61020630411966));
#45471=CARTESIAN_POINT('Ctrl Pts',(367.278507222014,-22.8163227084717,1.68068431151555));
#45472=CARTESIAN_POINT('Ctrl Pts',(367.32782096343,-22.8104490040274,1.78501700789984));
#45473=CARTESIAN_POINT('Ctrl Pts',(367.381812636293,-22.8045752995831,1.88735121774635));
#45474=CARTESIAN_POINT('Ctrl Pts',(367.440297597901,-22.7987015951388,1.98723816047698));
#45475=CARTESIAN_POINT('Ctrl Pts',(367.498707051017,-22.7928354740894,2.08699614163915));
#45476=CARTESIAN_POINT('Ctrl Pts',(367.561598049398,-22.78696935304,2.18431278583786));
#45477=CARTESIAN_POINT('Ctrl Pts',(367.628738563243,-22.7811032319907,2.2787607192605));
#45478=CARTESIAN_POINT('Ctrl Pts',(367.695810327044,-22.7752431176882,2.37311194059153));
#45479=CARTESIAN_POINT('Ctrl Pts',(367.767122713087,-22.7693830033858,2.46459995931142));
#45480=CARTESIAN_POINT('Ctrl Pts',(367.8423989425,-22.7635228890834,2.55282397192895));
#45481=CARTESIAN_POINT('Ctrl Pts',(367.920390691134,-22.7574513766658,2.64423058287519));
#45482=CARTESIAN_POINT('Ctrl Pts',(368.002637437747,-22.7513798642481,2.73213286028289));
#45483=CARTESIAN_POINT('Ctrl Pts',(368.088783529227,-22.7453083518305,2.81611971971314));
#45484=CARTESIAN_POINT('Ctrl Pts',(368.171834617418,-22.7394549729415,2.89708915140137));
#45485=CARTESIAN_POINT('Ctrl Pts',(368.258509364299,-22.7336015940525,2.97441935203995));
#45486=CARTESIAN_POINT('Ctrl Pts',(368.348450205572,-22.7277482151635,3.04777804939232));
#45487=CARTESIAN_POINT('Ctrl Pts',(368.438377542599,-22.7218957151351,3.12112573223926));
#45488=CARTESIAN_POINT('Ctrl Pts',(368.531569678868,-22.7160432151068,3.19050283641997));
#45489=CARTESIAN_POINT('Ctrl Pts',(368.627635530635,-22.7101907150784,3.25561701174666));
#45490=CARTESIAN_POINT('Ctrl Pts',(368.72371019009,-22.7043376784703,3.32073715699181));
#45491=CARTESIAN_POINT('Ctrl Pts',(368.822658746798,-22.6984846418622,3.38159336461209));
#45492=CARTESIAN_POINT('Ctrl Pts',(368.924061271353,-22.6926316052541,3.43793670555734));
#45493=CARTESIAN_POINT('Ctrl Pts',(369.025497614978,-22.6867766165817,3.49429883774479));
#45494=CARTESIAN_POINT('Ctrl Pts',(369.129389192919,-22.6809216279092,3.54614490987749));
#45495=CARTESIAN_POINT('Ctrl Pts',(369.235292274704,-22.6750666392367,3.59327235249964));
#45496=CARTESIAN_POINT('Ctrl Pts',(369.341315381472,-22.669205014828,3.64045320688651));
#45497=CARTESIAN_POINT('Ctrl Pts',(369.449354164626,-22.6633433904193,3.68290458971904));
#45498=CARTESIAN_POINT('Ctrl Pts',(369.558945662437,-22.6574817660107,3.7204723859972));
#45499=CARTESIAN_POINT('Ctrl Pts',(369.6686110574,-22.6516161891298,3.75806551410465));
#45500=CARTESIAN_POINT('Ctrl Pts',(369.779830856427,-22.645750612249,3.79076838233586));
#45501=CARTESIAN_POINT('Ctrl Pts',(369.892129401949,-22.6398850353681,3.81847743508899));
#45502=CARTESIAN_POINT('Ctrl Pts',(370.004592151318,-22.634010881793,3.84622700424463));
#45503=CARTESIAN_POINT('Ctrl Pts',(370.118136391639,-22.6281367282179,3.86896810414709));
#45504=CARTESIAN_POINT('Ctrl Pts',(370.232278734123,-22.6222625746428,3.88664867193735));
#45505=CARTESIAN_POINT('Ctrl Pts',(370.261140560636,-22.620777246782,3.89111934836741));
#45506=CARTESIAN_POINT('Ctrl Pts',(370.290040617557,-22.6192919189211,3.8952667281833));
#45507=CARTESIAN_POINT('Ctrl Pts',(370.318971081571,-22.6178065910602,3.89909049714761));
#45508=CARTESIAN_POINT('Ctrl Pts',(370.433375978564,-22.6119328940175,3.91421150918101));
#45509=CARTESIAN_POINT('Ctrl Pts',(370.548637482259,-22.6060591969748,3.92431823208454));
#45510=CARTESIAN_POINT('Ctrl Pts',(370.664278383264,-22.6001854999321,3.92932253431245));
#45511=CARTESIAN_POINT('Ctrl Pts',(370.779769984465,-22.5943193862082,3.93432037566593));
#45512=CARTESIAN_POINT('Ctrl Pts',(370.895639599885,-22.5884532724842,3.93422887912631));
#45513=CARTESIAN_POINT('Ctrl Pts',(371.011402319388,-22.5825871587603,3.9290113377087));
#45514=CARTESIAN_POINT('Ctrl Pts',(371.127046502571,-22.5767270516983,3.92379913884144));
#45515=CARTESIAN_POINT('Ctrl Pts',(371.242583597283,-22.5708669446364,3.91347135400912));
#45516=CARTESIAN_POINT('Ctrl Pts',(371.357526761736,-22.5650068375745,3.89804328324526));
#45517=CARTESIAN_POINT('Ctrl Pts',(371.476616593808,-22.5589353224109,3.88205863235104));
#45518=CARTESIAN_POINT('Ctrl Pts',(371.595068382299,-22.5528638072473,3.86059873458005));
#45519=CARTESIAN_POINT('Ctrl Pts',(371.712343885212,-22.5467922920837,3.83373959563648));
#45520=CARTESIAN_POINT('Ctrl Pts',(371.825405800721,-22.5409389201742,3.807845477748));
#45521=CARTESIAN_POINT('Ctrl Pts',(371.93737406427,-22.5350855482646,3.77693352043325));
#45522=CARTESIAN_POINT('Ctrl Pts',(372.047775626912,-22.529232176355,3.7411240598883));
#45523=CARTESIAN_POINT('Ctrl Pts',(372.158160615257,-22.5233796831969,3.70531997532418));
#45524=CARTESIAN_POINT('Ctrl Pts',(372.266978977489,-22.5175271900388,3.6646199769158));
#45525=CARTESIAN_POINT('Ctrl Pts',(372.373773040315,-22.5116746968806,3.61919420961895));
#45526=CARTESIAN_POINT('Ctrl Pts',(372.480576896583,-22.5058216670255,3.57376427659764));
#45527=CARTESIAN_POINT('Ctrl Pts',(372.585355704218,-22.4999686371703,3.52360787490648));
#45528=CARTESIAN_POINT('Ctrl Pts',(372.687672639604,-22.4941156073152,3.4689429277235));
#45529=CARTESIAN_POINT('Ctrl Pts',(372.79002370126,-22.4882606252702,3.41425974787208));
#45530=CARTESIAN_POINT('Ctrl Pts',(372.889910893705,-22.4824056432253,3.35506522695551));
#45531=CARTESIAN_POINT('Ctrl Pts',(372.986923446946,-22.4765506611803,3.2916224203086));
#45532=CARTESIAN_POINT('Ctrl Pts',(373.084045952894,-22.4706890431784,3.22810770844783));
#45533=CARTESIAN_POINT('Ctrl Pts',(373.178286970748,-22.4648274251764,3.1603353267557));
#45534=CARTESIAN_POINT('Ctrl Pts',(373.26926602179,-22.4589658071745,3.08861075831808));
#45535=CARTESIAN_POINT('Ctrl Pts',(373.360306421624,-22.4531002365793,3.01683782472846));
#45536=CARTESIAN_POINT('Ctrl Pts',(373.448080162715,-22.4472346659841,2.94110766694654));
#45537=CARTESIAN_POINT('Ctrl Pts',(373.532242369358,-22.4413690953889,2.86176384512115));
#45538=CARTESIAN_POINT('Ctrl Pts',(373.616527642049,-22.4354949478727,2.78230400292307));
#45539=CARTESIAN_POINT('Ctrl Pts',(373.697190554142,-22.4296208003566,2.69922024628117));
#45540=CARTESIAN_POINT('Ctrl Pts',(373.773925308593,-22.4237466528405,2.61289054656712));
#45541=CARTESIAN_POINT('Ctrl Pts',(373.793329191747,-22.4222612597764,2.59106039388171));
#45542=CARTESIAN_POINT('Ctrl Pts',(373.812482109396,-22.4207758667124,2.56902283568234));
#45543=CARTESIAN_POINT('Ctrl Pts',(373.831379555812,-22.4192904736484,2.54678427647057));
#45544=CARTESIAN_POINT('Ctrl Pts',(373.906105627588,-22.413416791762,2.4588464601537));
#45545=CARTESIAN_POINT('Ctrl Pts',(373.977082558144,-22.4075431098756,2.36747054783791));
#45546=CARTESIAN_POINT('Ctrl Pts',(374.043977589642,-22.4016694279892,2.27300976161881));
#45547=CARTESIAN_POINT('Ctrl Pts',(374.110786252033,-22.3958033296954,2.17867093503745));
#45548=CARTESIAN_POINT('Ctrl Pts',(374.173523259468,-22.3899372314015,2.08125548936411));
#45549=CARTESIAN_POINT('Ctrl Pts',(374.231894891679,-22.3840711331077,1.9811509957004));
#45550=CARTESIAN_POINT('Ctrl Pts',(374.29020675103,-22.3782110417294,1.88114900956628));
#45551=CARTESIAN_POINT('Ctrl Pts',(374.344161919814,-22.3723509503512,1.77846380735943));
#45552=CARTESIAN_POINT('Ctrl Pts',(374.393509332309,-22.3664908589729,1.67351277712822));
#45553=CARTESIAN_POINT('Ctrl Pts',(374.444637178159,-22.3604193380256,1.56477515899839));
#45554=CARTESIAN_POINT('Ctrl Pts',(374.490818237052,-22.3543478170783,1.45360549414194));
#45555=CARTESIAN_POINT('Ctrl Pts',(374.531824587499,-22.3482762961309,1.34049727713028));
#45556=CARTESIAN_POINT('Ctrl Pts',(374.571357475034,-22.3424229404393,1.23145332726116));
#45557=CARTESIAN_POINT('Ctrl Pts',(374.606080981888,-22.3365695847477,1.12060816350951));
#45558=CARTESIAN_POINT('Ctrl Pts',(374.635839782227,-22.3307162290561,1.00842452534259));
#45559=CARTESIAN_POINT('Ctrl Pts',(374.665594114077,-22.3248637522862,0.896257732320513));
#45560=CARTESIAN_POINT('Ctrl Pts',(374.690385115814,-22.3190112755162,0.782753263736838));
#45561=CARTESIAN_POINT('Ctrl Pts',(374.710107651526,-22.3131587987462,0.668387940778114));
#45562=CARTESIAN_POINT('Ctrl Pts',(374.729831995362,-22.3073057854323,0.554012133024494));
#45563=CARTESIAN_POINT('Ctrl Pts',(374.744486879243,-22.3014527721184,0.438775721166163));
#45564=CARTESIAN_POINT('Ctrl Pts',(374.754018618452,-22.2955997588045,0.323163907441151));
#45565=CARTESIAN_POINT('Ctrl Pts',(374.763553536615,-22.2897447934369,0.207513535719724));
#45566=CARTESIAN_POINT('Ctrl Pts',(374.767961878637,-22.2838898280694,0.0914879247014605));
#45567=CARTESIAN_POINT('Ctrl Pts',(374.767242008615,-22.2780348627018,-0.0244251497270083));
#45568=CARTESIAN_POINT('Ctrl Pts',(374.766521322715,-22.2721732614956,-0.140469596488608));
#45569=CARTESIAN_POINT('Ctrl Pts',(374.760660826619,-22.2663116602893,-0.256400838717909));
#45570=CARTESIAN_POINT('Ctrl Pts',(374.749710957994,-22.2604500590831,-0.37173355393506));
#45571=CARTESIAN_POINT('Ctrl Pts',(374.738753705824,-22.2545845053732,-0.48714403851341));
#45572=CARTESIAN_POINT('Ctrl Pts',(374.722700304747,-22.2487189516633,-0.60195478429041));
#45573=CARTESIAN_POINT('Ctrl Pts',(374.701652489631,-22.2428533979533,-0.715689744265365));
#45574=CARTESIAN_POINT('Ctrl Pts',(374.680573897299,-22.2369792673241,-0.829591013445971));
#45575=CARTESIAN_POINT('Ctrl Pts',(374.654486408507,-22.2311051366948,-0.942412956393667));
#45576=CARTESIAN_POINT('Ctrl Pts',(374.623541859078,-22.2252310060656,-1.05369370950997));
#45577=CARTESIAN_POINT('Ctrl Pts',(374.615716075734,-22.2237454561226,-1.08183627678901));
#45578=CARTESIAN_POINT('Ctrl Pts',(374.607579891213,-22.2222599061797,-1.10988037189724));
#45579=CARTESIAN_POINT('Ctrl Pts',(374.59913624562,-22.2207743562368,-1.13781873436821));
#45580=CARTESIAN_POINT('Ctrl Pts',(374.565751053908,-22.2149006647021,-1.24828376714679));
#45581=CARTESIAN_POINT('Ctrl Pts',(374.527444341865,-22.2090269731674,-1.35746218034026));
#45582=CARTESIAN_POINT('Ctrl Pts',(374.484332535484,-22.2031532816327,-1.46488286879456));
#45583=CARTESIAN_POINT('Ctrl Pts',(374.441276390344,-22.1972871735652,-1.57216486742287));
#45584=CARTESIAN_POINT('Ctrl Pts',(374.393427640688,-22.1914210654976,-1.67769327445173));
#45585=CARTESIAN_POINT('Ctrl Pts',(374.340952738837,-22.18555495743,-1.78101116756819));
#45586=CARTESIAN_POINT('Ctrl Pts',(374.288531570463,-22.1796948561652,-1.88422326478095));
#45587=CARTESIAN_POINT('Ctrl Pts',(374.23149385837,-22.1738347549003,-1.9852289842659));
#45588=CARTESIAN_POINT('Ctrl Pts',(374.170054233665,-22.1679746536355,-2.08359108277054));
#45589=CARTESIAN_POINT('Ctrl Pts',(374.10639803961,-22.1619031363517,-2.18550180993181));
#45590=CARTESIAN_POINT('Ctrl Pts',(374.038016487171,-22.155831619068,-2.28457414669948));
#45591=CARTESIAN_POINT('Ctrl Pts',(373.965200705124,-22.1497601017842,-2.3803490432448));
#45592=CARTESIAN_POINT('Ctrl Pts',(373.895001216564,-22.1439067359873,-2.47268271824497));
#45593=CARTESIAN_POINT('Ctrl Pts',(373.820680932575,-22.1380533701905,-2.5619514741141));
#45594=CARTESIAN_POINT('Ctrl Pts',(373.742544494684,-22.1322000043936,-2.64777393330716));
#45595=CARTESIAN_POINT('Ctrl Pts',(373.664419788648,-22.1263475174548,-2.73358350662222));
#45596=CARTESIAN_POINT('Ctrl Pts',(373.582480346069,-22.1204950305159,-2.8159475067253));
#45597=CARTESIAN_POINT('Ctrl Pts',(373.497069849824,-22.1146425435771,-2.89451909729439));
#45598=CARTESIAN_POINT('Ctrl Pts',(373.411651522551,-22.1087895200416,-2.97309789185331));
#45599=CARTESIAN_POINT('Ctrl Pts',(373.322761813033,-22.102936496506,-3.04788330592844));
#45600=CARTESIAN_POINT('Ctrl Pts',(373.230779338935,-22.0970834729705,-3.11856719464307));
#45601=CARTESIAN_POINT('Ctrl Pts',(373.138766186917,-22.0912284973393,-3.18927465779119));
#45602=CARTESIAN_POINT('Ctrl Pts',(373.04365854665,-22.0853735217081,-3.2558776238942));
#45603=CARTESIAN_POINT('Ctrl Pts',(372.945865414572,-22.0795185460768,-3.31811028993385));
#45604=CARTESIAN_POINT('Ctrl Pts',(372.847961446768,-22.0736569345964,-3.38041348856185));
#45605=CARTESIAN_POINT('Ctrl Pts',(372.747366260951,-22.067795323116,-3.43833627897722));
#45606=CARTESIAN_POINT('Ctrl Pts',(372.644515021486,-22.0619337116356,-3.49165794602192));
#45607=CARTESIAN_POINT('Ctrl Pts',(372.541594428768,-22.0560681476329,-3.54501556820991));
#45608=CARTESIAN_POINT('Ctrl Pts',(372.436415127124,-22.0502025836301,-3.59376571582147));
#45609=CARTESIAN_POINT('Ctrl Pts',(372.329432295354,-22.0443370196274,-3.63773580746802));
#45610=CARTESIAN_POINT('Ctrl Pts',(372.222293028913,-22.0384628787572,-3.68177019397988));
#45611=CARTESIAN_POINT('Ctrl Pts',(372.113345356373,-22.032588737887,-3.72101043559348));
#45612=CARTESIAN_POINT('Ctrl Pts',(372.003059698307,-22.0267145970168,-3.75533374010241));
#45613=CARTESIAN_POINT('Ctrl Pts',(371.975170661334,-22.0252291442863,-3.76401341727225));
#45614=CARTESIAN_POINT('Ctrl Pts',(371.947196111318,-22.0237436915557,-3.77237892031219));
#45615=CARTESIAN_POINT('Ctrl Pts',(371.919143741613,-22.0222582388252,-3.78042878413019));
#45616=CARTESIAN_POINT('Ctrl Pts',(371.808220707546,-22.01638454881,-3.81225908324351));
#45617=CARTESIAN_POINT('Ctrl Pts',(371.695710827206,-22.0105108587948,-3.83925630424263));
#45618=CARTESIAN_POINT('Ctrl Pts',(371.582073089335,-22.0046371687797,-3.86126289015244));
#45619=CARTESIAN_POINT('Ctrl Pts',(371.468582068139,-21.9987710622335,-3.88324106355463));
#45620=CARTESIAN_POINT('Ctrl Pts',(371.353966487155,-21.9929049556873,-3.90024133777612));
#45621=CARTESIAN_POINT('Ctrl Pts',(371.238700536937,-21.9870388491412,-3.91215588200584));
#45622=CARTESIAN_POINT('Ctrl Pts',(371.123552617278,-21.9811787493978,-3.92405822592576));
#45623=CARTESIAN_POINT('Ctrl Pts',(371.007756061563,-21.9753186496544,-3.93088515619298));
#45624=CARTESIAN_POINT('Ctrl Pts',(370.89179464207,-21.969458549911,-3.93257999521229));
#45625=CARTESIAN_POINT('Ctrl Pts',(370.771649617299,-21.9633870320569,-3.93433597989108));
#45626=CARTESIAN_POINT('Ctrl Pts',(370.651328051823,-21.9573155142029,-3.9305824892373));
#45627=CARTESIAN_POINT('Ctrl Pts',(370.531373512831,-21.9512439963488,-3.92131530568809));
#45628=CARTESIAN_POINT('Ctrl Pts',(370.415729018113,-21.9453906320634,-3.91238109804568));
#45629=CARTESIAN_POINT('Ctrl Pts',(370.300426076018,-21.9395372677781,-3.89832263430539));
#45630=CARTESIAN_POINT('Ctrl Pts',(370.185950309952,-21.9336839034927,-3.87918915868136));
#45631=CARTESIAN_POINT('Ctrl Pts',(370.071491731816,-21.927831418059,-3.86005855584751));
#45632=CARTESIAN_POINT('Ctrl Pts',(369.957860490144,-21.9219789326253,-3.83585452433464));
#45633=CARTESIAN_POINT('Ctrl Pts',(369.845534347769,-21.9161264471917,-3.80667784023542));
#45634=CARTESIAN_POINT('Ctrl Pts',(369.733197906395,-21.9102734251533,-3.77749848097424));
#45635=CARTESIAN_POINT('Ctrl Pts',(369.622167202093,-21.9044204031149,-3.74334566664515));
#45636=CARTESIAN_POINT('Ctrl Pts',(369.512906423454,-21.8985673810765,-3.70437050431956));
#45637=CARTESIAN_POINT('Ctrl Pts',(369.403609204057,-21.8927124069327,-3.66538234296141));
#45638=CARTESIAN_POINT('Ctrl Pts',(369.29608347304,-21.886857432789,-3.62156877420024));
#45639=CARTESIAN_POINT('Ctrl Pts',(369.190774307414,-21.8810024586452,-3.57312938654996));
#45640=CARTESIAN_POINT('Ctrl Pts',(369.085345787194,-21.8751408486302,-3.52463509899225));
#45641=CARTESIAN_POINT('Ctrl Pts',(368.982139222108,-21.8692792386152,-3.47150470101704));
#45642=CARTESIAN_POINT('Ctrl Pts',(368.881575987362,-21.8634176286002,-3.41398421280908));
#45643=CARTESIAN_POINT('Ctrl Pts',(368.780944941972,-21.8575520660518,-3.35642493804724));
#45644=CARTESIAN_POINT('Ctrl Pts',(368.682961124448,-21.8516865035034,-3.29446989873784));
#45645=CARTESIAN_POINT('Ctrl Pts',(368.588016312816,-21.8458209409549,-3.2284080271181));
#45646=CARTESIAN_POINT('Ctrl Pts',(368.492932668519,-21.8399468015116,-3.16224955679558));
#45647=CARTESIAN_POINT('Ctrl Pts',(368.40089722587,-21.8340726620682,-3.09197251906454));
#45648=CARTESIAN_POINT('Ctrl Pts',(368.312268187356,-21.8281985226248,-3.01790564512828));
#45649=CARTESIAN_POINT('Ctrl Pts',(368.289855454484,-21.8267130555544,-2.9991754288466));
#45650=CARTESIAN_POINT('Ctrl Pts',(368.267660371344,-21.8252275884839,-2.980203033827));
#45651=CARTESIAN_POINT('Ctrl Pts',(368.24568833986,-21.8237421214135,-2.96099413078456));
#45652=CARTESIAN_POINT('Ctrl Pts',(368.160079295419,-21.8179543354027,-2.88615099052049));
#45653=CARTESIAN_POINT('Ctrl Pts',(368.077556050416,-21.812166549392,-2.80744951203021));
#45654=CARTESIAN_POINT('Ctrl Pts',(367.998494309132,-21.8063787633812,-2.72517776058249));
#45655=CARTESIAN_POINT('Ctrl Pts',(367.919535386016,-21.800598504267,-2.64301300185433));
#45656=CARTESIAN_POINT('Ctrl Pts',(367.844029312231,-21.7948182451529,-2.55728750250962));
#45657=CARTESIAN_POINT('Ctrl Pts',(367.772318758495,-21.7890379860387,-2.46832950472104));
#45658=CARTESIAN_POINT('Ctrl Pts',(367.700688942408,-21.7832642348164,-2.37947166317517));
#45659=CARTESIAN_POINT('Ctrl Pts',(367.632846412028,-21.7774904835942,-2.28738889234054));
#45660=CARTESIAN_POINT('Ctrl Pts',(367.569096284465,-21.7717167323719,-2.19244546269971));
#45661=CARTESIAN_POINT('Ctrl Pts',(367.505385908326,-21.7659465813751,-2.09756123508105));
#45662=CARTESIAN_POINT('Ctrl Pts',(367.445763102122,-21.7601764303783,-1.9998202451201));
#45663=CARTESIAN_POINT('Ctrl Pts',(367.390491709746,-21.7544062793814,-1.89961851262268));
#45664=CARTESIAN_POINT('Ctrl Pts',(367.335240498746,-21.7486382352536,-1.79945336702284));
#45665=CARTESIAN_POINT('Ctrl Pts',(367.284337749468,-21.7428701911257,-1.69682963741078));
#45666=CARTESIAN_POINT('Ctrl Pts',(367.238002619847,-21.7371021469979,-1.59217013606627));
#45667=CARTESIAN_POINT('Ctrl Pts',(367.191672436426,-21.7313347185994,-1.48752180695413));
#45668=CARTESIAN_POINT('Ctrl Pts',(367.149909074613,-21.7255672902009,-1.38083852842445));
#45669=CARTESIAN_POINT('Ctrl Pts',(367.112884205147,-21.7197998618025,-1.27256457712676));
#45670=CARTESIAN_POINT('Ctrl Pts',(367.075835587684,-21.7140287341372,-1.16422117819842));
#45671=CARTESIAN_POINT('Ctrl Pts',(367.043531673585,-21.7082576064719,-1.05428547188577));
#45672=CARTESIAN_POINT('Ctrl Pts',(367.016094664113,-21.7024864788066,-0.943218255833407));
#45673=CARTESIAN_POINT('Ctrl Pts',(366.988648916011,-21.6967135130491,-0.832115665104043));
#45674=CARTESIAN_POINT('Ctrl Pts',(366.966073245815,-21.6909405472917,-0.719881264654684));
#45675=CARTESIAN_POINT('Ctrl Pts',(366.948438634091,-21.6851675815342,-0.606985744735938));
#45676=CARTESIAN_POINT('Ctrl Pts',(366.930781460406,-21.6793872297663,-0.493945784760898));
#45677=CARTESIAN_POINT('Ctrl Pts',(366.918078021018,-21.6736068779983,-0.380243439605345));
#45678=CARTESIAN_POINT('Ctrl Pts',(366.910347366434,-21.6678265262303,-0.26635431064342));
#45679=CARTESIAN_POINT('Ctrl Pts',(366.904256389624,-21.6632721915121,-0.176621153410323));
#45680=CARTESIAN_POINT('Ctrl Pts',(366.901251405202,-21.6587178567939,-0.086772175312987));
#45681=CARTESIAN_POINT('Ctrl Pts',(366.901318968034,-21.6541635220757,0.00296126550371329));
#45682=CARTESIAN_POINT('',(366.901319018817,-20.4041635219962,-0.00302796160370392));
#45683=CARTESIAN_POINT('Ctrl Pts',(366.901318968035,-21.654163522035,0.00296126630494888));
#45684=CARTESIAN_POINT('Ctrl Pts',(366.901462062567,-21.6445176826906,0.193011933961706));
#45685=CARTESIAN_POINT('Ctrl Pts',(366.915382244365,-21.6348718433462,0.382553237646774));
#45686=CARTESIAN_POINT('Ctrl Pts',(366.942850574199,-21.6252260040018,0.570062642413103));
#45687=CARTESIAN_POINT('Ctrl Pts',(366.959577003038,-21.6193523143247,0.684243691444853));
#45688=CARTESIAN_POINT('Ctrl Pts',(366.981360893976,-21.6134786246476,0.797878119509283));
#45689=CARTESIAN_POINT('Ctrl Pts',(367.008156582755,-21.6076049349706,0.910482801795613));
#45690=CARTESIAN_POINT('Ctrl Pts',(367.034917675798,-21.6017388287755,1.02294210091921));
#45691=CARTESIAN_POINT('Ctrl Pts',(367.066677603814,-21.5958727225804,1.13437389994923));
#45692=CARTESIAN_POINT('Ctrl Pts',(367.103339131433,-21.5900066163853,1.24430172287202));
#45693=CARTESIAN_POINT('Ctrl Pts',(367.139963118132,-21.5841465170056,1.35411698115575));
#45694=CARTESIAN_POINT('Ctrl Pts',(367.181478590949,-21.5782864176258,1.4624309370287));
#45695=CARTESIAN_POINT('Ctrl Pts',(367.227737760038,-21.572426318246,1.56877947189326));
#45696=CARTESIAN_POINT('Ctrl Pts',(367.275665851171,-21.5663548002604,1.67896481182259));
#45697=CARTESIAN_POINT('Ctrl Pts',(367.328686279273,-21.5602832822747,1.78703979826397));
#45698=CARTESIAN_POINT('Ctrl Pts',(367.386578809746,-21.554211764289,1.89250746050753));
#45699=CARTESIAN_POINT('Ctrl Pts',(367.442391219151,-21.5483584003963,1.99418559231555));
#45700=CARTESIAN_POINT('Ctrl Pts',(367.502731424096,-21.5425050365037,2.09344014831502));
#45701=CARTESIAN_POINT('Ctrl Pts',(367.567354368616,-21.536651672611,2.18984898799886));
#45702=CARTESIAN_POINT('Ctrl Pts',(367.631967610231,-21.5307991875801,2.28624335223775));
#45703=CARTESIAN_POINT('Ctrl Pts',(367.700862082847,-21.5249467025493,2.37979250665416));
#45704=CARTESIAN_POINT('Ctrl Pts',(367.773749021348,-21.5190942175184,2.47010271554592));
#45705=CARTESIAN_POINT('Ctrl Pts',(367.84664264261,-21.5132411958926,2.56042120468205));
#45706=CARTESIAN_POINT('Ctrl Pts',(367.923529197954,-21.5073881742667,2.64749983643114));
#45707=CARTESIAN_POINT('Ctrl Pts',(368.004079662593,-21.5015351526409,2.7309779904447));
#45708=CARTESIAN_POINT('Ctrl Pts',(368.084656992372,-21.4956801789189,2.81448398603912));
#45709=CARTESIAN_POINT('Ctrl Pts',(368.168900374585,-21.489825205197,2.89438681895903));
#45710=CARTESIAN_POINT('Ctrl Pts',(368.25644449253,-21.4839702314751,2.97036326671102));
#45711=CARTESIAN_POINT('Ctrl Pts',(368.34408783047,-21.4781086218938,3.04642582399143));
#45712=CARTESIAN_POINT('Ctrl Pts',(368.435039058674,-21.4722470123125,3.11855284312117));
#45713=CARTESIAN_POINT('Ctrl Pts',(368.528900328275,-21.4663854027312,3.18646183652911));
#45714=CARTESIAN_POINT('Ctrl Pts',(368.622824889213,-21.4605198406238,3.25441662146577));
#45715=CARTESIAN_POINT('Ctrl Pts',(368.719663054588,-21.4546542785165,3.31814749059416));
#45716=CARTESIAN_POINT('Ctrl Pts',(368.818990080293,-21.4487887164091,3.37741661150248));
#45717=CARTESIAN_POINT('Ctrl Pts',(368.91846234642,-21.4429145774144,3.4367723983722));
#45718=CARTESIAN_POINT('Ctrl Pts',(369.020430373649,-21.4370404384196,3.49165322137277));
#45719=CARTESIAN_POINT('Ctrl Pts',(369.12444699891,-21.4311662994248,3.54186824452422));
#45720=CARTESIAN_POINT('Ctrl Pts',(369.15075105381,-21.4296808284799,3.55456677922894));
#45721=CARTESIAN_POINT('Ctrl Pts',(369.177186030337,-21.4281953575351,3.56696718210002));
#45722=CARTESIAN_POINT('Ctrl Pts',(369.20374453511,-21.4267098865903,3.57906686920699));
#45723=CARTESIAN_POINT('Ctrl Pts',(369.308759318052,-21.4208361971574,3.62691015052295));
#45724=CARTESIAN_POINT('Ctrl Pts',(369.416056469331,-21.4149625077246,3.67020727878341));
#45725=CARTESIAN_POINT('Ctrl Pts',(369.525205260397,-21.4090888182918,3.70873471945656));
#45726=CARTESIAN_POINT('Ctrl Pts',(369.634213130147,-21.4032227123424,3.74721241759396));
#45727=CARTESIAN_POINT('Ctrl Pts',(369.745067499455,-21.397356606393,3.78093253835209));
#45728=CARTESIAN_POINT('Ctrl Pts',(369.85731526961,-21.3914905004436,3.80971848718675));
#45729=CARTESIAN_POINT('Ctrl Pts',(369.969448099506,-21.3856304013105,3.83847495958339));
#45730=CARTESIAN_POINT('Ctrl Pts',(370.082971094361,-21.3797703021775,3.86230720793355));
#45731=CARTESIAN_POINT('Ctrl Pts',(370.197414133432,-21.3739102030444,3.88108781808859));
#45732=CARTESIAN_POINT('Ctrl Pts',(370.315986015037,-21.3678386849667,3.90054598961064));
#45733=CARTESIAN_POINT('Ctrl Pts',(370.435545154513,-21.3617671668889,3.91458098755703));
#45734=CARTESIAN_POINT('Ctrl Pts',(370.555554552153,-21.3556956488112,3.92310846421255));
#45735=CARTESIAN_POINT('Ctrl Pts',(370.67125191749,-21.3498422851663,3.93132954190662));
#45736=CARTESIAN_POINT('Ctrl Pts',(370.78736729414,-21.3439889215214,3.93443203439455));
#45737=CARTESIAN_POINT('Ctrl Pts',(370.903413106987,-21.3381355578765,3.932393017732));
#45738=CARTESIAN_POINT('Ctrl Pts',(371.019441495968,-21.3322830730934,3.93035430722056));
#45739=CARTESIAN_POINT('Ctrl Pts',(371.135399928944,-21.3264305883103,3.92317562979976));
#45740=CARTESIAN_POINT('Ctrl Pts',(371.250801004433,-21.3205781035271,3.91088618918516));
#45741=CARTESIAN_POINT('Ctrl Pts',(371.366212660671,-21.3147250821487,3.89859562179172));
#45742=CARTESIAN_POINT('Ctrl Pts',(371.48106644699,-21.3088720607703,3.88119340344505));
#45743=CARTESIAN_POINT('Ctrl Pts',(371.59488096385,-21.3030190393919,3.85876052052402));
#45744=CARTESIAN_POINT('Ctrl Pts',(371.708733440068,-21.2971640659168,3.83632015579964));
#45745=CARTESIAN_POINT('Ctrl Pts',(371.821545552466,-21.2913090924418,3.80884587007231));
#45746=CARTESIAN_POINT('Ctrl Pts',(371.932847653023,-21.2854541189668,3.77646941983565));
#45747=CARTESIAN_POINT('Ctrl Pts',(372.044275900236,-21.2795925096302,3.74405627504493));
#45748=CARTESIAN_POINT('Ctrl Pts',(372.154190322822,-21.2737309002936,3.70672999181425));
#45749=CARTESIAN_POINT('Ctrl Pts',(372.262137866638,-21.267869290957,3.66467174645908));
#45750=CARTESIAN_POINT('Ctrl Pts',(372.370158200288,-21.2620037290935,3.62258514091495));
#45751=CARTESIAN_POINT('Ctrl Pts',(372.47620863724,-21.25613816723,3.57576038612259));
#45752=CARTESIAN_POINT('Ctrl Pts',(372.579859067264,-21.2502726053664,3.52442546666655));
#45753=CARTESIAN_POINT('Ctrl Pts',(372.68366105965,-21.2443984666122,3.47301548296206));
#45754=CARTESIAN_POINT('Ctrl Pts',(372.785055680867,-21.238524327858,3.41708237148672));
#45755=CARTESIAN_POINT('Ctrl Pts',(372.883640158626,-21.2326501891038,3.35689843286626));
#45756=CARTESIAN_POINT('Ctrl Pts',(372.908570555483,-21.2311647157954,3.3416789022838));
#45757=CARTESIAN_POINT('Ctrl Pts',(372.933321403113,-21.229679242487,3.32618773626215));
#45758=CARTESIAN_POINT('Ctrl Pts',(372.957886522166,-21.2281937691786,3.310429746768));
#45759=CARTESIAN_POINT('Ctrl Pts',(373.055019116987,-21.2223200798767,3.24812130016971));
#45760=CARTESIAN_POINT('Ctrl Pts',(373.14956883754,-21.2164463905749,3.18143044890682));
#45761=CARTESIAN_POINT('Ctrl Pts',(373.241114343966,-21.2105727012731,3.11059795733082));
#45762=CARTESIAN_POINT('Ctrl Pts',(373.332541656519,-21.2047065954575,3.03985691717411));
#45763=CARTESIAN_POINT('Ctrl Pts',(373.420972144683,-21.1988404896419,2.96498512114153));
#45764=CARTESIAN_POINT('Ctrl Pts',(373.506011785558,-21.1929743838263,2.88626757802014));
#45765=CARTESIAN_POINT('Ctrl Pts',(373.590964346904,-21.1871142848296,2.8076306406784));
#45766=CARTESIAN_POINT('Ctrl Pts',(373.672532666037,-21.181254185833,2.72515606823215));
#45767=CARTESIAN_POINT('Ctrl Pts',(373.750354818921,-21.1753940868364,2.6391698343777));
#45768=CARTESIAN_POINT('Ctrl Pts',(373.830984619247,-21.1693225687085,2.55008141148618));
#45769=CARTESIAN_POINT('Ctrl Pts',(373.907592486155,-21.1632510505806,2.4572234339288));
#45770=CARTESIAN_POINT('Ctrl Pts',(373.97981642891,-21.1571795324527,2.3610014210833));
#45771=CARTESIAN_POINT('Ctrl Pts',(374.049445306176,-21.15132616895,2.26823674406441));
#45772=CARTESIAN_POINT('Ctrl Pts',(374.114999604277,-21.1454728054472,2.17234597520425));
#45773=CARTESIAN_POINT('Ctrl Pts',(374.176195740932,-21.1396194419445,2.07372640038332));
#45774=CARTESIAN_POINT('Ctrl Pts',(374.237382689185,-21.1337669573054,1.97512163297348));
#45775=CARTESIAN_POINT('Ctrl Pts',(374.294212559335,-21.1279144726664,1.87378922523877));
#45776=CARTESIAN_POINT('Ctrl Pts',(374.346445666511,-21.1220619880273,1.77015457605792));
#45777=CARTESIAN_POINT('Ctrl Pts',(374.398683562755,-21.1162089667947,1.66651042498352));
#45778=CARTESIAN_POINT('Ctrl Pts',(374.446323672241,-21.110355945562,1.56056398180142));
#45779=CARTESIAN_POINT('Ctrl Pts',(374.489173077186,-21.1045029243294,1.45276367378729));
#45780=CARTESIAN_POINT('Ctrl Pts',(374.532036773231,-21.0986479510017,1.34492741229908));
#45781=CARTESIAN_POINT('Ctrl Pts',(374.570106435071,-21.092792977674,1.23523644023758));
#45782=CARTESIAN_POINT('Ctrl Pts',(374.603238178056,-21.0869380043463,1.12415683294903));
#45783=CARTESIAN_POINT('Ctrl Pts',(374.636407471615,-21.0810763951587,1.01295133119911));
#45784=CARTESIAN_POINT('Ctrl Pts',(374.664627557895,-21.0752147859711,0.90035444906362));
#45785=CARTESIAN_POINT('Ctrl Pts',(374.68780507581,-21.0693531767835,0.786845108878447));
#45786=CARTESIAN_POINT('Ctrl Pts',(374.710998222494,-21.0634876150701,0.67325922851727));
#45787=CARTESIAN_POINT('Ctrl Pts',(374.729141965679,-21.0576220533567,0.55876007199698));
#45788=CARTESIAN_POINT('Ctrl Pts',(374.742194715749,-21.0517564916432,0.44383265691022));
#45789=CARTESIAN_POINT('Ctrl Pts',(374.755266552142,-21.0458823530396,0.328737189747755));
#45790=CARTESIAN_POINT('Ctrl Pts',(374.763232510194,-21.040008214436,0.213212624824722));
#45791=CARTESIAN_POINT('Ctrl Pts',(374.766103059565,-21.0341340758323,0.0977450315970521));
#45792=CARTESIAN_POINT('Ctrl Pts',(374.766828975093,-21.0326486011438,0.0685451439789517));
#45793=CARTESIAN_POINT('Ctrl Pts',(374.76722929728,-21.0311631264554,0.0393488768321781));
#45794=CARTESIAN_POINT('Ctrl Pts',(374.767304719775,-21.0296776517669,0.0101640313471547));
#45795=CARTESIAN_POINT('Ctrl Pts',(374.767602946543,-21.0238039623397,-0.105235254610351));
#45796=CARTESIAN_POINT('Ctrl Pts',(374.762818403329,-21.0179302729126,-0.220839874219748));
#45797=CARTESIAN_POINT('Ctrl Pts',(374.752924993982,-21.0120565834854,-0.336165251624106));
#45798=CARTESIAN_POINT('Ctrl Pts',(374.743044357955,-21.0061904775427,-0.451341733140617));
#45799=CARTESIAN_POINT('Ctrl Pts',(374.728068008118,-21.0003243715999,-0.566239281550414));
#45800=CARTESIAN_POINT('Ctrl Pts',(374.708021836049,-20.9944582656572,-0.680372290326572));
#45801=CARTESIAN_POINT('Ctrl Pts',(374.687996191004,-20.9885981665318,-0.79438842836331));
#45802=CARTESIAN_POINT('Ctrl Pts',(374.662911120963,-20.9827380674064,-0.907641179479606));
#45803=CARTESIAN_POINT('Ctrl Pts',(374.632844341741,-20.9768779682811,-1.01964970261153));
#45804=CARTESIAN_POINT('Ctrl Pts',(374.601692821987,-20.9708064502008,-1.13569923672116));
#45805=CARTESIAN_POINT('Ctrl Pts',(374.565193387622,-20.9647349321206,-1.25041261998707));
#45806=CARTESIAN_POINT('Ctrl Pts',(374.523490561151,-20.9586634140403,-1.36326583287554));
#45807=CARTESIAN_POINT('Ctrl Pts',(374.48328615021,-20.9528100504056,-1.47206414058933));
#45808=CARTESIAN_POINT('Ctrl Pts',(374.438245991465,-20.9469566867709,-1.57913323143716));
#45809=CARTESIAN_POINT('Ctrl Pts',(374.388550194724,-20.9411033231361,-1.6840194365367));
#45810=CARTESIAN_POINT('Ctrl Pts',(374.338861859639,-20.9352508383641,-1.78888989332864));
#45811=CARTESIAN_POINT('Ctrl Pts',(374.28451945334,-20.929398353592,-1.89157774281137));
#45812=CARTESIAN_POINT('Ctrl Pts',(374.225750506413,-20.92354586882,-1.99165096311623));
#45813=CARTESIAN_POINT('Ctrl Pts',(374.166976171161,-20.9176928474535,-2.09173335879387));
#45814=CARTESIAN_POINT('Ctrl Pts',(374.103774697706,-20.9118398260871,-2.18920029246472));
#45815=CARTESIAN_POINT('Ctrl Pts',(374.036418320457,-20.9059868047206,-2.28364655709858));
#45816=CARTESIAN_POINT('Ctrl Pts',(373.969039478554,-20.9001318312584,-2.37812432138689));
#45817=CARTESIAN_POINT('Ctrl Pts',(373.897503217131,-20.8942768577962,-2.46957907718035));
#45818=CARTESIAN_POINT('Ctrl Pts',(373.822123181737,-20.8884218843341,-2.55763725319067));
#45819=CARTESIAN_POINT('Ctrl Pts',(373.746657712757,-20.8825602750116,-2.64579523183126));
#45820=CARTESIAN_POINT('Ctrl Pts',(373.667340043466,-20.8766986656891,-2.73054863311337));
#45821=CARTESIAN_POINT('Ctrl Pts',(373.584522004144,-20.8708370563667,-2.81155937662081));
#45822=CARTESIAN_POINT('Ctrl Pts',(373.501648120009,-20.864971494518,-2.89262474626734));
#45823=CARTESIAN_POINT('Ctrl Pts',(373.415269472988,-20.8591059326693,-2.96994215802653));
#45824=CARTESIAN_POINT('Ctrl Pts',(373.325771081059,-20.8532403708207,-3.04321373115855));
#45825=CARTESIAN_POINT('Ctrl Pts',(373.236141820534,-20.8473662320823,-3.11659244529731));
#45826=CARTESIAN_POINT('Ctrl Pts',(373.143384040499,-20.8414920933439,-3.18591326757319));
#45827=CARTESIAN_POINT('Ctrl Pts',(373.047911864646,-20.8356179546056,-3.25092149283786));
#45828=CARTESIAN_POINT('Ctrl Pts',(373.023768516049,-20.8341324811888,-3.26736100759955));
#45829=CARTESIAN_POINT('Ctrl Pts',(372.999451702815,-20.832647007772,-3.28352496149948));
#45830=CARTESIAN_POINT('Ctrl Pts',(372.974968356363,-20.8311615343553,-3.29940970832831));
#45831=CARTESIAN_POINT('Ctrl Pts',(372.878159103019,-20.8252878449632,-3.3622193607201));
#45832=CARTESIAN_POINT('Ctrl Pts',(372.778421888268,-20.8194141555711,-3.42086923500197));
#45833=CARTESIAN_POINT('Ctrl Pts',(372.676149758024,-20.8135404661791,-3.47507470919122));
#45834=CARTESIAN_POINT('Ctrl Pts',(372.574009670706,-20.8076743602717,-3.52921019902198));
#45835=CARTESIAN_POINT('Ctrl Pts',(372.469341538159,-20.8018082543643,-3.57891250832556));
#45836=CARTESIAN_POINT('Ctrl Pts',(372.36256745542,-20.795942148457,-3.62394014208116));
#45837=CARTESIAN_POINT('Ctrl Pts',(372.25590270798,-20.7900820493672,-3.66892166811432));
#45838=CARTESIAN_POINT('Ctrl Pts',(372.147136678156,-20.7842219502774,-3.70923788037558));
#45839=CARTESIAN_POINT('Ctrl Pts',(372.036715550944,-20.7783618511876,-3.74469341555734));
#45840=CARTESIAN_POINT('Ctrl Pts',(371.922310681417,-20.7722903330941,-3.78142810554691));
#45841=CARTESIAN_POINT('Ctrl Pts',(371.806129434527,-20.7662188150006,-3.81294456082372));
#45842=CARTESIAN_POINT('Ctrl Pts',(371.688690495029,-20.7601472969071,-3.83908014880324));
#45843=CARTESIAN_POINT('Ctrl Pts',(371.575471230432,-20.7542939333084,-3.86427666423074));
#45844=CARTESIAN_POINT('Ctrl Pts',(371.461083535459,-20.7484405697096,-3.88447223798209));
#45845=CARTESIAN_POINT('Ctrl Pts',(371.346006270866,-20.7425872061109,-3.89957227952645));
#45846=CARTESIAN_POINT('Ctrl Pts',(371.230946284735,-20.7367347213749,-3.91467005385065));
#45847=CARTESIAN_POINT('Ctrl Pts',(371.115197344378,-20.7308822366389,-3.92467376349189));
#45848=CARTESIAN_POINT('Ctrl Pts',(370.999245827649,-20.7250297519029,-3.92954040102045));
#45849=CARTESIAN_POINT('Ctrl Pts',(370.883283679722,-20.7191767305725,-3.9344074847544));
#45850=CARTESIAN_POINT('Ctrl Pts',(370.767119331304,-20.7133237092421,-3.93413654274455));
#45851=CARTESIAN_POINT('Ctrl Pts',(370.651240861902,-20.7074706879118,-3.92873666911497));
#45852=CARTESIAN_POINT('Ctrl Pts',(370.535323744791,-20.7016157144856,-3.92333499452317));
#45853=CARTESIAN_POINT('Ctrl Pts',(370.41969310876,-20.6957607410595,-3.91280100608526));
#45854=CARTESIAN_POINT('Ctrl Pts',(370.304832898927,-20.6899057676334,-3.89719574606833));
#45855=CARTESIAN_POINT('Ctrl Pts',(370.189842509796,-20.6840441583469,-3.88157279949325));
#45856=CARTESIAN_POINT('Ctrl Pts',(370.075624699288,-20.6781825490603,-3.86086716505694));
#45857=CARTESIAN_POINT('Ctrl Pts',(369.962654289566,-20.6723209397737,-3.83519121189423));
#45858=CARTESIAN_POINT('Ctrl Pts',(369.849607703065,-20.6664553779609,-3.80949794524739));
#45859=CARTESIAN_POINT('Ctrl Pts',(369.737810589667,-20.660589816148,-3.77882779528158));
#45860=CARTESIAN_POINT('Ctrl Pts',(369.627721982798,-20.6547242543352,-3.74334281164189));
#45861=CARTESIAN_POINT('Ctrl Pts',(369.517472399383,-20.6488501156323,-3.70780594025235));
#45862=CARTESIAN_POINT('Ctrl Pts',(369.408936694131,-20.6429759769294,-3.66744032764705));
#45863=CARTESIAN_POINT('Ctrl Pts',(369.302553398164,-20.6371018382264,-3.62245588713179));
#45864=CARTESIAN_POINT('Ctrl Pts',(369.275650799715,-20.6356163644655,-3.6110800566627));
#45865=CARTESIAN_POINT('Ctrl Pts',(369.248885720453,-20.6341308907045,-3.59940907819713));
#45866=CARTESIAN_POINT('Ctrl Pts',(369.222264981911,-20.6326454169436,-3.58744679961843));
#45867=CARTESIAN_POINT('Ctrl Pts',(369.117004321368,-20.6267717275623,-3.54014693441));
#45868=CARTESIAN_POINT('Ctrl Pts',(369.013651879269,-20.6208980381811,-3.48813162499381));
#45869=CARTESIAN_POINT('Ctrl Pts',(368.912659899626,-20.6150243487998,-3.43157685465056));
#45870=CARTESIAN_POINT('Ctrl Pts',(368.81179831012,-20.6091582429035,-3.37509510183053));
#45871=CARTESIAN_POINT('Ctrl Pts',(368.713291479616,-20.6032921370072,-3.31408574345183));
#45872=CARTESIAN_POINT('Ctrl Pts',(368.61757116001,-20.5974260311109,-3.24877255253829));
#45873=CARTESIAN_POINT('Ctrl Pts',(368.521948856795,-20.5915659320324,-3.18352624150192));
#45874=CARTESIAN_POINT('Ctrl Pts',(368.429107728167,-20.585705832954,-3.1139850954336));
#45875=CARTESIAN_POINT('Ctrl Pts',(368.339453820575,-20.5798457338755,-3.0404181387758));
#45876=CARTESIAN_POINT('Ctrl Pts',(368.246565404325,-20.5737742157779,-2.96419705398559));
#45877=CARTESIAN_POINT('Ctrl Pts',(368.157098920584,-20.5677026976802,-2.88365441067547));
#45878=CARTESIAN_POINT('Ctrl Pts',(368.071472214734,-20.5616311795826,-2.79913789904588));
#45879=CARTESIAN_POINT('Ctrl Pts',(367.988922145043,-20.5557778159957,-2.71765813340816));
#45880=CARTESIAN_POINT('Ctrl Pts',(367.909940988646,-20.5499244524088,-2.63248546851741));
#45881=CARTESIAN_POINT('Ctrl Pts',(367.83486782568,-20.544071088822,-2.54397101639699));
#45882=CARTESIAN_POINT('Ctrl Pts',(367.759805934698,-20.538218604098,-2.45546985442505));
#45883=CARTESIAN_POINT('Ctrl Pts',(367.688651137584,-20.5323661193741,-2.36362821790201));
#45884=CARTESIAN_POINT('Ctrl Pts',(367.621703243882,-20.5265136346502,-2.26883149921726));
#45885=CARTESIAN_POINT('Ctrl Pts',(367.554749211957,-20.520660613332,-2.1740260889475));
#45886=CARTESIAN_POINT('Ctrl Pts',(367.492003088555,-20.5148075920139,-2.07626539540011));
#45887=CARTESIAN_POINT('Ctrl Pts',(367.433721824355,-20.5089545706958,-1.97596448562208));
#45888=CARTESIAN_POINT('Ctrl Pts',(367.375421122228,-20.5030995972821,-1.87563012355448));
#45889=CARTESIAN_POINT('Ctrl Pts',(367.321588447799,-20.4972446238683,-1.77275421764004));
#45890=CARTESIAN_POINT('Ctrl Pts',(367.272434858023,-20.4913896504546,-1.66777652234879));
#45891=CARTESIAN_POINT('Ctrl Pts',(367.223225558967,-20.4855280411807,-1.5626798483248));
#45892=CARTESIAN_POINT('Ctrl Pts',(367.178706104605,-20.4796664319067,-1.4554770047493));
#45893=CARTESIAN_POINT('Ctrl Pts',(367.139039475882,-20.4738048226327,-1.34662790478673));
#45894=CARTESIAN_POINT('Ctrl Pts',(367.099346099661,-20.4679392608326,-1.23770540707748));
#45895=CARTESIAN_POINT('Ctrl Pts',(367.06451218878,-20.4620736990324,-1.12713483563783));
#45896=CARTESIAN_POINT('Ctrl Pts',(367.034650418039,-20.4562081372323,-1.01538976851012));
#45897=CARTESIAN_POINT('Ctrl Pts',(367.004744982065,-20.4503339985422,-0.903481302686307));
#45898=CARTESIAN_POINT('Ctrl Pts',(366.979826284859,-20.4444598598521,-0.790395315589137));
#45899=CARTESIAN_POINT('Ctrl Pts',(366.959955666518,-20.4385857211619,-0.676614104360887));
#45900=CARTESIAN_POINT('Ctrl Pts',(366.954930711198,-20.4371002472853,-0.647840691635513));
#45901=CARTESIAN_POINT('Ctrl Pts',(366.950228321566,-20.4356147734086,-0.61902283481969));
#45902=CARTESIAN_POINT('Ctrl Pts',(366.945848962233,-20.4341292995319,-0.590168352075471));
#45903=CARTESIAN_POINT('Ctrl Pts',(366.916401365424,-20.4241407070329,-0.396145640250567));
#45904=CARTESIAN_POINT('Ctrl Pts',(366.901470561325,-20.414152114534,-0.199865450662548));
#45905=CARTESIAN_POINT('Ctrl Pts',(366.901319018817,-20.404163522035,-0.00302796236916899));
#45906=CARTESIAN_POINT('',(366.901318010803,-19.1541635220604,-0.00111333548553648));
#45907=CARTESIAN_POINT('Ctrl Pts',(366.901319018817,-20.4041635219962,-0.0030279616036751));
#45908=CARTESIAN_POINT('Ctrl Pts',(366.901231322656,-20.3983832201483,0.11087998863384));
#45909=CARTESIAN_POINT('Ctrl Pts',(366.90609632481,-20.3926029183004,0.224972287379443));
#45910=CARTESIAN_POINT('Ctrl Pts',(366.915935485385,-20.3868226164526,0.338775175314392));
#45911=CARTESIAN_POINT('Ctrl Pts',(366.925764417016,-20.3810483238963,0.452459752000542));
#45912=CARTESIAN_POINT('Ctrl Pts',(366.940557191422,-20.3752740313399,0.565855093955342));
#45913=CARTESIAN_POINT('Ctrl Pts',(366.960283225851,-20.3694997387836,0.678487071293573));
#45914=CARTESIAN_POINT('Ctrl Pts',(366.979994813569,-20.3637296751327,0.791036560608706));
#45915=CARTESIAN_POINT('Ctrl Pts',(367.004632405412,-20.3579596114818,0.902823378231744));
#45916=CARTESIAN_POINT('Ctrl Pts',(367.034113639211,-20.3521895478308,1.01337896751405));
#45917=CARTESIAN_POINT('Ctrl Pts',(367.063583643743,-20.3464216819709,1.1238924466753));
#45918=CARTESIAN_POINT('Ctrl Pts',(367.097893515297,-20.340653816111,1.23317521771722));
#45919=CARTESIAN_POINT('Ctrl Pts',(367.136910043896,-20.3348859502511,1.34077011136149));
#45920=CARTESIAN_POINT('Ctrl Pts',(367.175921796339,-20.3291187904567,1.44835183392218));
#45921=CARTESIAN_POINT('Ctrl Pts',(367.219638915172,-20.3233516306623,1.55424568894855));
#45922=CARTESIAN_POINT('Ctrl Pts',(367.267878980043,-20.3175844708678,1.65801168990651));
#45923=CARTESIAN_POINT('Ctrl Pts',(367.316125609432,-20.3118165262773,1.76179181136108));
#45924=CARTESIAN_POINT('Ctrl Pts',(367.368896227151,-20.3060485816867,1.86344311711508));
#45925=CARTESIAN_POINT('Ctrl Pts',(367.425961516331,-20.3002806370961,1.96254836392981));
#45926=CARTESIAN_POINT('Ctrl Pts',(367.483083981629,-20.2945069133588,2.06175290846663));
#45927=CARTESIAN_POINT('Ctrl Pts',(367.54450949664,-20.2887331896216,2.15840593060013));
#45928=CARTESIAN_POINT('Ctrl Pts',(367.609964294208,-20.2829594658843,2.25211747616834));
#45929=CARTESIAN_POINT('Ctrl Pts',(367.675453624201,-20.277182696065,2.34587846176203));
#45930=CARTESIAN_POINT('Ctrl Pts',(367.744976208484,-20.2714059262458,2.43669454396946));
#45931=CARTESIAN_POINT('Ctrl Pts',(367.818217922316,-20.2656291564266,2.52420882788628));
#45932=CARTESIAN_POINT('Ctrl Pts',(367.89157503594,-20.2598432847172,2.61186099948479));
#45933=CARTESIAN_POINT('Ctrl Pts',(367.968662692478,-20.2540574130078,2.69620067064413));
#45934=CARTESIAN_POINT('Ctrl Pts',(368.049129715814,-20.2482715412984,2.77690763966548));
#45935=CARTESIAN_POINT('Ctrl Pts',(368.107811768382,-20.2440520882391,2.83576467702415));
#45936=CARTESIAN_POINT('Ctrl Pts',(368.168290314052,-20.2398326351797,2.89269051561767));
#45937=CARTESIAN_POINT('Ctrl Pts',(368.230418786639,-20.2356131821203,2.94757504587047));
#45938=CARTESIAN_POINT('Ctrl Pts',(368.316904723356,-20.2297394927299,3.02397705307496));
#45939=CARTESIAN_POINT('Ctrl Pts',(368.406900162807,-20.2238658033395,3.09669665584127));
#45940=CARTESIAN_POINT('Ctrl Pts',(368.500058339928,-20.2179921139491,3.16539437109935));
#45941=CARTESIAN_POINT('Ctrl Pts',(368.59309624109,-20.2121260080435,3.23400339115313));
#45942=CARTESIAN_POINT('Ctrl Pts',(368.689288429921,-20.2062599021379,3.29860060718184));
#45943=CARTESIAN_POINT('Ctrl Pts',(368.788253048743,-20.2003937962324,3.35888490661179));
#45944=CARTESIAN_POINT('Ctrl Pts',(368.887116329057,-20.1945336971445,3.41910747568724));
#45945=CARTESIAN_POINT('Ctrl Pts',(368.988746041749,-20.1886735980566,3.47502569904019));
#45946=CARTESIAN_POINT('Ctrl Pts',(369.092729698256,-20.1828134989688,3.52638053795624));
#45947=CARTESIAN_POINT('Ctrl Pts',(369.20046484787,-20.1767419808746,3.57958814230331));
#45948=CARTESIAN_POINT('Ctrl Pts',(369.310726634467,-20.1706704627804,3.627896604315));
#45949=CARTESIAN_POINT('Ctrl Pts',(369.423026034938,-20.1645989446862,3.67106856427918));
#45950=CARTESIAN_POINT('Ctrl Pts',(369.531290428198,-20.1587455810896,3.71268932121818));
#45951=CARTESIAN_POINT('Ctrl Pts',(369.641448110423,-20.152892217493,3.74953617995368));
#45952=CARTESIAN_POINT('Ctrl Pts',(369.753039410706,-20.1470388538964,3.78144495262681));
#45953=CARTESIAN_POINT('Ctrl Pts',(369.864613955932,-20.1411863691627,3.81334893430517));
#45954=CARTESIAN_POINT('Ctrl Pts',(369.977621294096,-20.1353338844289,3.84031619062319));
#45955=CARTESIAN_POINT('Ctrl Pts',(370.09158671091,-20.1294813996951,3.86223244383833));
#45956=CARTESIAN_POINT('Ctrl Pts',(370.205562576823,-20.1236283783671,3.8841507064796));
#45957=CARTESIAN_POINT('Ctrl Pts',(370.320496290277,-20.1177753570391,3.90101696737526));
#45958=CARTESIAN_POINT('Ctrl Pts',(370.43590376897,-20.111922335711,3.91276822945954));
#45959=CARTESIAN_POINT('Ctrl Pts',(370.551349738286,-20.1060673622873,3.92452341081674));
#45960=CARTESIAN_POINT('Ctrl Pts',(370.667269376239,-20.1002123888636,3.93116015932616));
#45961=CARTESIAN_POINT('Ctrl Pts',(370.783175027343,-20.0943574154399,3.93266746768156));
#45962=CARTESIAN_POINT('Ctrl Pts',(370.899212042615,-20.0884958061559,3.93417648437738));
#45963=CARTESIAN_POINT('Ctrl Pts',(371.015234626056,-20.0826341968718,3.93054445202503));
#45964=CARTESIAN_POINT('Ctrl Pts',(371.130756574637,-20.0767725875878,3.92181247441115));
#45965=CARTESIAN_POINT('Ctrl Pts',(371.246356420516,-20.0709070257775,3.91307460876061));
#45966=CARTESIAN_POINT('Ctrl Pts',(371.361454550161,-20.0650414639673,3.89922999939243));
#45967=CARTESIAN_POINT('Ctrl Pts',(371.475573048707,-20.059175902157,3.88037121603933));
#45968=CARTESIAN_POINT('Ctrl Pts',(371.589858416487,-20.0533017634568,3.8614848565195));
#45969=CARTESIAN_POINT('Ctrl Pts',(371.703160891651,-20.0474276247565,3.8375697752771));
#45970=CARTESIAN_POINT('Ctrl Pts',(371.815015777495,-20.0415534860563,3.80876890626494));
#45971=CARTESIAN_POINT('Ctrl Pts',(371.843302052105,-20.0400680122737,3.80148563666306));
#45972=CARTESIAN_POINT('Ctrl Pts',(371.871495846026,-20.0385825384911,3.79389016328918));
#45973=CARTESIAN_POINT('Ctrl Pts',(371.899589844776,-20.0370970647086,3.78598528576312));
#45974=CARTESIAN_POINT('Ctrl Pts',(372.010675899816,-20.0312233753189,3.75472872923835));
#45975=CARTESIAN_POINT('Ctrl Pts',(372.120570136323,-20.0253496859293,3.71852684355849));
#45976=CARTESIAN_POINT('Ctrl Pts',(372.228799299368,-20.0194759965397,3.67748698112704));
#45977=CARTESIAN_POINT('Ctrl Pts',(372.336888728397,-20.0136098906349,3.63650010501367));
#45978=CARTESIAN_POINT('Ctrl Pts',(372.443316976368,-20.0077437847302,3.59068781910305));
#45979=CARTESIAN_POINT('Ctrl Pts',(372.547624007345,-20.0018776788254,3.54020776540738));
#45980=CARTESIAN_POINT('Ctrl Pts',(372.651824229251,-19.9960175797383,3.48977940264374));
#45981=CARTESIAN_POINT('Ctrl Pts',(372.753907184975,-19.9901574806513,3.43469295828946));
#45982=CARTESIAN_POINT('Ctrl Pts',(372.853431588279,-19.9842973815643,3.37515462237087));
#45983=CARTESIAN_POINT('Ctrl Pts',(372.956546605026,-19.9782258634698,3.31346827910693));
#45984=CARTESIAN_POINT('Ctrl Pts',(373.056914547964,-19.9721543453753,3.24700291130202));
#45985=CARTESIAN_POINT('Ctrl Pts',(373.154070857786,-19.9660828272808,3.17604077395526));
#45986=CARTESIAN_POINT('Ctrl Pts',(373.247736263728,-19.9602294636851,3.10762836293089));
#45987=CARTESIAN_POINT('Ctrl Pts',(373.338416495504,-19.9543761000894,3.03503703071331));
#45988=CARTESIAN_POINT('Ctrl Pts',(373.425724392798,-19.9485227364937,2.95856403457036));
#45989=CARTESIAN_POINT('Ctrl Pts',(373.513019181105,-19.9426702517608,2.8821025205905));
#45990=CARTESIAN_POINT('Ctrl Pts',(373.596942331033,-19.9368177670279,2.80176077369107));
#45991=CARTESIAN_POINT('Ctrl Pts',(373.677140466967,-19.930965282295,2.7178757489612));
#45992=CARTESIAN_POINT('Ctrl Pts',(373.757345955993,-19.9251122609679,2.63398303310116));
#45993=CARTESIAN_POINT('Ctrl Pts',(373.833825466572,-19.9192592396408,2.54654669224039));
#45994=CARTESIAN_POINT('Ctrl Pts',(373.906263636155,-19.9134062183136,2.45593935322757));
#45995=CARTESIAN_POINT('Ctrl Pts',(373.978725965266,-19.9075512448909,2.36530179491757));
#45996=CARTESIAN_POINT('Ctrl Pts',(374.047144015364,-19.9016962714681,2.27149145800744));
#45997=CARTESIAN_POINT('Ctrl Pts',(374.111244174247,-19.8958412980453,2.17491215606266));
#45998=CARTESIAN_POINT('Ctrl Pts',(374.175416982426,-19.8899796887622,2.07822339388427));
#45999=CARTESIAN_POINT('Ctrl Pts',(374.235261903116,-19.8841180794791,1.9787597473006));
#46000=CARTESIAN_POINT('Ctrl Pts',(374.290549900864,-19.878256470196,1.87695205928742));
#46001=CARTESIAN_POINT('Ctrl Pts',(374.345875179716,-19.8723909083867,1.7750757216023));
#46002=CARTESIAN_POINT('Ctrl Pts',(374.396637236606,-19.8665253465774,1.67085256566643));
#46003=CARTESIAN_POINT('Ctrl Pts',(374.442654776415,-19.8606597847681,1.56473437002358));
#46004=CARTESIAN_POINT('Ctrl Pts',(374.488739605154,-19.8547856460689,1.4584610035519));
#46005=CARTESIAN_POINT('Ctrl Pts',(374.530065924134,-19.8489115073696,1.35028745158401));
#46006=CARTESIAN_POINT('Ctrl Pts',(374.566501925374,-19.8430373686703,1.24068168826238));
#46007=CARTESIAN_POINT('Ctrl Pts',(374.575715995328,-19.8415518948792,1.2129641798573));
#46008=CARTESIAN_POINT('Ctrl Pts',(374.584617583338,-19.8400664210881,1.18515513506618));
#46009=CARTESIAN_POINT('Ctrl Pts',(374.593205076696,-19.838580947297,1.15726221800511));
#46010=CARTESIAN_POINT('Ctrl Pts',(374.627160753958,-19.8327072579059,1.04697125763385));
#46011=CARTESIAN_POINT('Ctrl Pts',(374.656314736158,-19.8268335685148,0.93500088175898));
#46012=CARTESIAN_POINT('Ctrl Pts',(374.680500676367,-19.8209598791237,0.821806966968872));
#46013=CARTESIAN_POINT('Ctrl Pts',(374.704655390255,-19.8150937732174,0.708759196156783));
#46014=CARTESIAN_POINT('Ctrl Pts',(374.723854732371,-19.8092276673111,0.594491428277202));
#46015=CARTESIAN_POINT('Ctrl Pts',(374.737981780678,-19.8033615614048,0.479475694372454));
#46016=CARTESIAN_POINT('Ctrl Pts',(374.752094363068,-19.7975014623162,0.364577735113922));
#46017=CARTESIAN_POINT('Ctrl Pts',(374.761144932806,-19.7916413632276,0.248933740910155));
#46018=CARTESIAN_POINT('Ctrl Pts',(374.765067527524,-19.785781264139,0.133026305624597));
#46019=CARTESIAN_POINT('Ctrl Pts',(374.76913164051,-19.7797097460451,0.0129371945163077));
#46020=CARTESIAN_POINT('Ctrl Pts',(374.767690686835,-19.7736382279512,-0.107434283569311));
#46021=CARTESIAN_POINT('Ctrl Pts',(374.760730005568,-19.7675667098573,-0.227544742681113));
#46022=CARTESIAN_POINT('Ctrl Pts',(374.754019427142,-19.76171334626,-0.343339537021934));
#46023=CARTESIAN_POINT('Ctrl Pts',(374.742178977134,-19.7558599826627,-0.458891299009031));
#46024=CARTESIAN_POINT('Ctrl Pts',(374.72524855987,-19.7500066190654,-0.573713548799026));
#46025=CARTESIAN_POINT('Ctrl Pts',(374.708320684652,-19.7441541343309,-0.688518558414818));
#46026=CARTESIAN_POINT('Ctrl Pts',(374.686304422026,-19.7383016495965,-0.80259386501185));
#46027=CARTESIAN_POINT('Ctrl Pts',(374.659291349718,-19.732449164862,-0.915459857730073));
#46028=CARTESIAN_POINT('Ctrl Pts',(374.632275800675,-19.7265961435332,-1.02833619874454));
#46029=CARTESIAN_POINT('Ctrl Pts',(374.600262627379,-19.7207431222045,-1.1400026036461));
#46030=CARTESIAN_POINT('Ctrl Pts',(374.563393990059,-19.7148901008758,-1.24999206625128));
#46031=CARTESIAN_POINT('Ctrl Pts',(374.526513056336,-19.7090351274514,-1.360018212466));
#46032=CARTESIAN_POINT('Ctrl Pts',(374.484773569738,-19.703180154027,-1.46836591274371));
#46033=CARTESIAN_POINT('Ctrl Pts',(374.438366530196,-19.6973251806026,-1.57458633742882));
#46034=CARTESIAN_POINT('Ctrl Pts',(374.391906894235,-19.6914635713179,-1.68092714932196));
#46035=CARTESIAN_POINT('Ctrl Pts',(374.340769312161,-19.6856019620332,-1.7851354946226));
#46036=CARTESIAN_POINT('Ctrl Pts',(374.285191662409,-19.6797403527485,-1.88678534896728));
#46037=CARTESIAN_POINT('Ctrl Pts',(374.229576536241,-19.6738747909376,-1.98850374655527));
#46038=CARTESIAN_POINT('Ctrl Pts',(374.169515594253,-19.6680092291267,-2.08765986541362));
#46039=CARTESIAN_POINT('Ctrl Pts',(374.105290187692,-19.6621436673158,-2.1838564483839));
#46040=CARTESIAN_POINT('Ctrl Pts',(374.040970867834,-19.6562695286149,-2.28019369435216));
#46041=CARTESIAN_POINT('Ctrl Pts',(373.972475173792,-19.650395389914,-2.37356243585731));
#46042=CARTESIAN_POINT('Ctrl Pts',(373.900124893551,-19.6445212512131,-2.46359822038484));
#46043=CARTESIAN_POINT('Ctrl Pts',(373.881828688872,-19.6430357774372,-2.48636680036273));
#46044=CARTESIAN_POINT('Ctrl Pts',(373.863286166021,-19.6415503036612,-2.50892242206025));
#46045=CARTESIAN_POINT('Ctrl Pts',(373.844502890951,-19.6400648298853,-2.53125957551702));
#46046=CARTESIAN_POINT('Ctrl Pts',(373.77023222708,-19.6341911404948,-2.61958257616356));
#46047=CARTESIAN_POINT('Ctrl Pts',(373.691947292622,-19.6283174511043,-2.70478110188831));
#46048=CARTESIAN_POINT('Ctrl Pts',(373.609940985998,-19.6224437617138,-2.78646823502634));
#46049=CARTESIAN_POINT('Ctrl Pts',(373.52804055722,-19.6165776558081,-2.86804990240119));
#46050=CARTESIAN_POINT('Ctrl Pts',(373.442428601165,-19.6107115499024,-2.94612890400492));
#46051=CARTESIAN_POINT('Ctrl Pts',(373.353438384673,-19.6048454439967,-3.02035109681497));
#46052=CARTESIAN_POINT('Ctrl Pts',(373.26453929303,-19.5989853449088,-3.09449728704487));
#46053=CARTESIAN_POINT('Ctrl Pts',(373.172269137165,-19.5931252458208,-3.16479426096192));
#46054=CARTESIAN_POINT('Ctrl Pts',(373.076997685662,-19.5872651467329,-3.23092497114606));
#46055=CARTESIAN_POINT('Ctrl Pts',(372.978289057536,-19.5811936286387,-3.29944152648665));
#46056=CARTESIAN_POINT('Ctrl Pts',(372.876358805226,-19.5751221105446,-3.36348520493569));
#46057=CARTESIAN_POINT('Ctrl Pts',(372.771655592382,-19.5690505924505,-3.42274911210763));
#46058=CARTESIAN_POINT('Ctrl Pts',(372.670714449654,-19.5631972288538,-3.47988361973153));
#46059=CARTESIAN_POINT('Ctrl Pts',(372.567196576746,-19.5573438652571,-3.53257570586077));
#46060=CARTESIAN_POINT('Ctrl Pts',(372.461532399002,-19.5514905016604,-3.58059517706343));
#46061=CARTESIAN_POINT('Ctrl Pts',(372.355884086378,-19.5456380169266,-3.62860743830404));
#46062=CARTESIAN_POINT('Ctrl Pts',(372.248090485718,-19.5397855321927,-3.6719483087314));
#46063=CARTESIAN_POINT('Ctrl Pts',(372.138604262947,-19.5339330474589,-3.71043474021725));
#46064=CARTESIAN_POINT('Ctrl Pts',(372.02910800176,-19.5280800261308,-3.74892470039212));
#46065=CARTESIAN_POINT('Ctrl Pts',(371.917919199743,-19.5222270048027,-3.78255919981715));
#46066=CARTESIAN_POINT('Ctrl Pts',(371.80550735227,-19.5163739834746,-3.81120452835368));
#46067=CARTESIAN_POINT('Ctrl Pts',(371.693058013274,-19.5105190100508,-3.83985941066048));
#46068=CARTESIAN_POINT('Ctrl Pts',(371.579385217847,-19.504664036627,-3.8635217113549));
#46069=CARTESIAN_POINT('Ctrl Pts',(371.464969663949,-19.4988090632033,-3.88210861435243));
#46070=CARTESIAN_POINT('Ctrl Pts',(371.350424434717,-19.4929474539192,-3.90071658321714));
#46071=CARTESIAN_POINT('Ctrl Pts',(371.235135174816,-19.4870858446351,-3.91423760683349));
#46072=CARTESIAN_POINT('Ctrl Pts',(371.119588832025,-19.481224235351,-3.92264062445873));
#46073=CARTESIAN_POINT('Ctrl Pts',(371.003964575486,-19.4753586735407,-3.93104930830047));
#46074=CARTESIAN_POINT('Ctrl Pts',(370.888083302831,-19.4694931117304,-3.9343331025536));
#46075=CARTESIAN_POINT('Ctrl Pts',(370.772431355553,-19.4636275499201,-3.93251307199429));
#46076=CARTESIAN_POINT('Ctrl Pts',(370.656610296762,-19.4577534112198,-3.93069038010392));
#46077=CARTESIAN_POINT('Ctrl Pts',(370.5410196434,-19.4518792725196,-3.92374899371222));
#46078=CARTESIAN_POINT('Ctrl Pts',(370.4261400921,-19.4460051338193,-3.91176174061301));
#46079=CARTESIAN_POINT('Ctrl Pts',(370.397088928987,-19.4445196600374,-3.90873035999636));
#46080=CARTESIAN_POINT('Ctrl Pts',(370.368083184964,-19.4430341862556,-3.90537654957453));
#46081=CARTESIAN_POINT('Ctrl Pts',(370.339130507451,-19.4415487124737,-3.90170199945955));
#46082=CARTESIAN_POINT('Ctrl Pts',(370.224649163647,-19.4356750230832,-3.88717251648345));
#46083=CARTESIAN_POINT('Ctrl Pts',(370.110617166372,-19.4298013336927,-3.86757600285977));
#46084=CARTESIAN_POINT('Ctrl Pts',(369.997518428598,-19.4239276443022,-3.84294883168448));
#46085=CARTESIAN_POINT('Ctrl Pts',(369.884565711919,-19.4180615383965,-3.8183534565009));
#46086=CARTESIAN_POINT('Ctrl Pts',(369.772544258537,-19.4121954324909,-3.78874042739295));
#46087=CARTESIAN_POINT('Ctrl Pts',(369.661932324736,-19.4063293265852,-3.75419780680127));
#46088=CARTESIAN_POINT('Ctrl Pts',(369.551433656145,-19.4004692274973,-3.71969055741278));
#46089=CARTESIAN_POINT('Ctrl Pts',(369.442342028251,-19.3946091284093,-3.68026387953251));
#46090=CARTESIAN_POINT('Ctrl Pts',(369.335124313554,-19.3887490293213,-3.63605661818013));
#46091=CARTESIAN_POINT('Ctrl Pts',(369.224038428312,-19.3826775112271,-3.59025445969042));
#46092=CARTESIAN_POINT('Ctrl Pts',(369.11496466351,-19.376605993133,-3.53932035601397));
#46093=CARTESIAN_POINT('Ctrl Pts',(369.008404129742,-19.3705344750389,-3.48346495237152));
#46094=CARTESIAN_POINT('Ctrl Pts',(368.905672401115,-19.3646811114422,-3.42961647802152));
#46095=CARTESIAN_POINT('Ctrl Pts',(368.805276804193,-19.3588277478455,-3.37119447813662));
#46096=CARTESIAN_POINT('Ctrl Pts',(368.707644109995,-19.3529743842489,-3.30843585246246));
#46097=CARTESIAN_POINT('Ctrl Pts',(368.610026075017,-19.3471218995151,-3.2456866497847));
#46098=CARTESIAN_POINT('Ctrl Pts',(368.515170465349,-19.3412694147812,-3.17860233934627));
#46099=CARTESIAN_POINT('Ctrl Pts',(368.423476492272,-19.3354169300474,-3.10746406774455));
#46100=CARTESIAN_POINT('Ctrl Pts',(368.331774112089,-19.3295639087193,-3.03631927371842));
#46101=CARTESIAN_POINT('Ctrl Pts',(368.243234271194,-19.3237108873912,-2.96112003289903));
#46102=CARTESIAN_POINT('Ctrl Pts',(368.158223845174,-19.3178578660631,-2.88218838039403));
#46103=CARTESIAN_POINT('Ctrl Pts',(368.073185066535,-19.3120028926394,-2.80323040265899));
#46104=CARTESIAN_POINT('Ctrl Pts',(367.991678346035,-19.3061479192157,-2.72053781890731));
#46105=CARTESIAN_POINT('Ctrl Pts',(367.914033865616,-19.300292945792,-2.63446966802033));
#46106=CARTESIAN_POINT('Ctrl Pts',(367.836301385151,-19.2944313365079,-2.54830396993912));
#46107=CARTESIAN_POINT('Ctrl Pts',(367.762440158595,-19.2885697272239,-2.45875537564755));
#46108=CARTESIAN_POINT('Ctrl Pts',(367.692740265555,-19.2827081179398,-2.36621623286088));
#46109=CARTESIAN_POINT('Ctrl Pts',(367.622993373365,-19.2768425561296,-2.27361469025088));
#46110=CARTESIAN_POINT('Ctrl Pts',(367.557413635232,-19.2709769943193,-2.17801892359211));
#46111=CARTESIAN_POINT('Ctrl Pts',(367.496247000607,-19.2651114325091,-2.07984902887398));
#46112=CARTESIAN_POINT('Ctrl Pts',(367.43499092536,-19.2592372938089,-1.98153558569172));
#46113=CARTESIAN_POINT('Ctrl Pts',(367.378161034244,-19.2533631551086,-1.88064086102556));
#46114=CARTESIAN_POINT('Ctrl Pts',(367.325956719709,-19.2474890164084,-1.77760826866929));
#46115=CARTESIAN_POINT('Ctrl Pts',(367.312755100797,-19.2460035426262,-1.75155300806664));
#46116=CARTESIAN_POINT('Ctrl Pts',(367.299849044302,-19.2445180688441,-1.72536112121797));
#46117=CARTESIAN_POINT('Ctrl Pts',(367.287241275747,-19.243032595062,-1.69903995053532));
#46118=CARTESIAN_POINT('Ctrl Pts',(367.233428325467,-19.23669224019,-1.58669494331932));
#46119=CARTESIAN_POINT('Ctrl Pts',(367.184895602673,-19.2303518853181,-1.47166404912409));
#46120=CARTESIAN_POINT('Ctrl Pts',(367.141897960567,-19.2240115304461,-1.35444613636435));
#46121=CARTESIAN_POINT('Ctrl Pts',(367.099044455801,-19.2176924298067,-1.23762116324669));
#46122=CARTESIAN_POINT('Ctrl Pts',(367.061689140577,-19.2113733291672,-1.11862407952074));
#46123=CARTESIAN_POINT('Ctrl Pts',(367.030039023062,-19.2050542285278,-0.99797373832264));
#46124=CARTESIAN_POINT('Ctrl Pts',(366.998454638872,-19.198748251868,-0.877573972753616));
#46125=CARTESIAN_POINT('Ctrl Pts',(366.972551921596,-19.1924422752082,-0.755528088159374));
#46126=CARTESIAN_POINT('Ctrl Pts',(366.952489164617,-19.1861362985484,-0.632372542341981));
#46127=CARTESIAN_POINT('Ctrl Pts',(366.932489836403,-19.1798502583463,-0.50960635497981));
#46128=CARTESIAN_POINT('Ctrl Pts',(366.918293709533,-19.1735642181442,-0.385737804481959));
#46129=CARTESIAN_POINT('Ctrl Pts',(366.910008536092,-19.167278177942,-0.261314721109544));
#46130=CARTESIAN_POINT('Ctrl Pts',(366.904246710676,-19.1629066259815,-0.174786166317576));
#46131=CARTESIAN_POINT('Ctrl Pts',(366.901342603383,-19.158535074021,-0.0879897673060905));
#46132=CARTESIAN_POINT('Ctrl Pts',(366.901318010803,-19.1541635220605,-0.00111333548552649));
#46133=CARTESIAN_POINT('',(366.901319490285,-17.9041635219925,0.00358847020308838));
#46134=CARTESIAN_POINT('Ctrl Pts',(366.901318010803,-19.154163522035,-0.0011133349797373));
#46135=CARTESIAN_POINT('Ctrl Pts',(366.90128418225,-19.1481501902697,0.118390404615894));
#46136=CARTESIAN_POINT('Ctrl Pts',(366.906701360906,-19.1421368585045,0.237841410527132));
#46137=CARTESIAN_POINT('Ctrl Pts',(366.917528943227,-19.1361235267392,0.356726273948674));
#46138=CARTESIAN_POINT('Ctrl Pts',(366.928364304895,-19.1301058745454,0.47569655317238));
#46139=CARTESIAN_POINT('Ctrl Pts',(366.944617781229,-19.1240882223516,0.594099501001153));
#46140=CARTESIAN_POINT('Ctrl Pts',(366.966197139492,-19.1180705701578,0.711428945152156));
#46141=CARTESIAN_POINT('Ctrl Pts',(366.988177612702,-19.1119410624489,0.830939297238127));
#46142=CARTESIAN_POINT('Ctrl Pts',(367.015683841127,-19.1058115547399,0.949335435228387));
#46143=CARTESIAN_POINT('Ctrl Pts',(367.048564873449,-19.0996820470309,1.06609726391429));
#46144=CARTESIAN_POINT('Ctrl Pts',(367.080932279724,-19.0936482867664,1.18103518646783));
#46145=CARTESIAN_POINT('Ctrl Pts',(367.118507592269,-19.0876145265018,1.29438915399849));
#46146=CARTESIAN_POINT('Ctrl Pts',(367.161097846325,-19.0815807662372,1.40568267433245));
#46147=CARTESIAN_POINT('Ctrl Pts',(367.204701873171,-19.0754033848061,1.51962530641805));
#46148=CARTESIAN_POINT('Ctrl Pts',(367.253562401351,-19.0692260033749,1.6314077777596));
#46149=CARTESIAN_POINT('Ctrl Pts',(367.30742253689,-19.0630486219438,1.74054543968912));
#46150=CARTESIAN_POINT('Ctrl Pts',(367.361282672429,-19.0568712405126,1.84968310161863));
#46151=CARTESIAN_POINT('Ctrl Pts',(367.420142152239,-19.0506938590815,1.95617561959075));
#46152=CARTESIAN_POINT('Ctrl Pts',(367.483697301148,-19.0445164776503,2.05957056592082));
#46153=CARTESIAN_POINT('Ctrl Pts',(367.544127955791,-19.0386427882598,2.15788241634883));
#46154=CARTESIAN_POINT('Ctrl Pts',(367.608989833161,-19.0327690988692,2.25369607202037));
#46155=CARTESIAN_POINT('Ctrl Pts',(367.678050308889,-19.0268954094786,2.34658564484133));
#46156=CARTESIAN_POINT('Ctrl Pts',(367.747021621055,-19.0210293035729,2.43935528849727));
#46157=CARTESIAN_POINT('Ctrl Pts',(367.820180507169,-19.0151631976671,2.52920802854385));
#46158=CARTESIAN_POINT('Ctrl Pts',(367.897249581732,-19.0092970917614,2.61574443870113));
#46159=CARTESIAN_POINT('Ctrl Pts',(367.974239738545,-19.0034369926734,2.70219223667677));
#46160=CARTESIAN_POINT('Ctrl Pts',(368.055131846414,-18.9975768935853,2.7853301527562));
#46161=CARTESIAN_POINT('Ctrl Pts',(368.139606945752,-18.9917167944973,2.86479006650617));
#46162=CARTESIAN_POINT('Ctrl Pts',(368.227129713956,-18.9856452764032,2.94711671266731));
#46163=CARTESIAN_POINT('Ctrl Pts',(368.318498617669,-18.9795737583091,3.02549459551379));
#46164=CARTESIAN_POINT('Ctrl Pts',(368.413315167613,-18.973502240215,3.09955399957246));
#46165=CARTESIAN_POINT('Ctrl Pts',(368.504724883143,-18.9676488766182,3.17095239005631));
#46166=CARTESIAN_POINT('Ctrl Pts',(368.59933840182,-18.9617955130215,3.23833701764886));
#46167=CARTESIAN_POINT('Ctrl Pts',(368.696763959796,-18.9559421494248,3.30141671902981));
#46168=CARTESIAN_POINT('Ctrl Pts',(368.794174889652,-18.9500896646909,3.3644869492059));
#46169=CARTESIAN_POINT('Ctrl Pts',(368.894396672571,-18.944237179957,3.42325331391641));
#46170=CARTESIAN_POINT('Ctrl Pts',(368.997008593458,-18.9383846952231,3.47746799898695));
#46171=CARTESIAN_POINT('Ctrl Pts',(369.09962992248,-18.9325316738949,3.5316876548161));
#46172=CARTESIAN_POINT('Ctrl Pts',(369.204641459794,-18.9266786525668,3.58135460838431));
#46173=CARTESIAN_POINT('Ctrl Pts',(369.311598567582,-18.9208256312386,3.62626736150748));
#46174=CARTESIAN_POINT('Ctrl Pts',(369.418591347632,-18.9149706578148,3.67119509390114));
#46175=CARTESIAN_POINT('Ctrl Pts',(369.527530607717,-18.909115684391,3.71136531305094));
#46176=CARTESIAN_POINT('Ctrl Pts',(369.637953123096,-18.9032607109672,3.74662520576918));
#46177=CARTESIAN_POINT('Ctrl Pts',(369.748500788212,-18.8973991016831,3.78192506104692));
#46178=CARTESIAN_POINT('Ctrl Pts',(369.860534670168,-18.891537492399,3.81230335629716));
#46179=CARTESIAN_POINT('Ctrl Pts',(369.973577728849,-18.8856758831148,3.83765754572904));
#46180=CARTESIAN_POINT('Ctrl Pts',(370.086697013295,-18.8798103213045,3.86302883167708));
#46181=CARTESIAN_POINT('Ctrl Pts',(370.200826423755,-18.8739447594941,3.88336919365258));
#46182=CARTESIAN_POINT('Ctrl Pts',(370.315481831255,-18.8680791976838,3.89862773066463));
#46183=CARTESIAN_POINT('Ctrl Pts',(370.430304893082,-18.8622050589835,3.91390857940021));
#46184=CARTESIAN_POINT('Ctrl Pts',(370.54565507699,-18.8563309202831,3.92409273681971));
#46185=CARTESIAN_POINT('Ctrl Pts',(370.66104620208,-18.8504567815828,3.92918133138568));
#46186=CARTESIAN_POINT('Ctrl Pts',(370.690226733843,-18.8489713078014,3.93046815387957));
#46187=CARTESIAN_POINT('Ctrl Pts',(370.719409901697,-18.8474858340201,3.93142937397189));
#46188=CARTESIAN_POINT('Ctrl Pts',(370.748587892579,-18.8460003602387,3.93206553529412));
#46189=CARTESIAN_POINT('Ctrl Pts',(370.863960144606,-18.8401266708481,3.9345809711476));
#46190=CARTESIAN_POINT('Ctrl Pts',(370.979635351959,-18.8342529814576,3.93201852063389));
#46191=CARTESIAN_POINT('Ctrl Pts',(371.095129529651,-18.828379292067,3.92434278184756));
#46192=CARTESIAN_POINT('Ctrl Pts',(371.21047459351,-18.8225131861612,3.91667695316111));
#46193=CARTESIAN_POINT('Ctrl Pts',(371.325638684041,-18.8166470802555,3.90391099203634));
#46194=CARTESIAN_POINT('Ctrl Pts',(371.440135786891,-18.8107809743497,3.88606145489848));
#46195=CARTESIAN_POINT('Ctrl Pts',(371.554515646166,-18.8049208752617,3.86823019545921));
#46196=CARTESIAN_POINT('Ctrl Pts',(371.668229470489,-18.7990607761736,3.84532577747209));
#46197=CARTESIAN_POINT('Ctrl Pts',(371.780795014347,-18.7932006770856,3.81741666359245));
#46198=CARTESIAN_POINT('Ctrl Pts',(371.897421666223,-18.7871291589915,3.78850065255498));
#46199=CARTESIAN_POINT('Ctrl Pts',(372.012815167939,-18.7810576408974,3.75421204151851));
#46200=CARTESIAN_POINT('Ctrl Pts',(372.126448819855,-18.7749861228033,3.71468525787507));
#46201=CARTESIAN_POINT('Ctrl Pts',(372.235999523843,-18.7691327592065,3.67657870315703));
#46202=CARTESIAN_POINT('Ctrl Pts',(372.343914243535,-18.7632793956098,3.63360406847437));
#46203=CARTESIAN_POINT('Ctrl Pts',(372.449735933199,-18.757426032013,3.58593271365921));
#46204=CARTESIAN_POINT('Ctrl Pts',(372.555541734092,-18.7515735472791,3.53826851653749));
#46205=CARTESIAN_POINT('Ctrl Pts',(372.65925475324,-18.7457210625452,3.48590917112646));
#46206=CARTESIAN_POINT('Ctrl Pts',(372.760438676795,-18.7398685778113,3.4290738652014));
#46207=CARTESIAN_POINT('Ctrl Pts',(372.861631877556,-18.7340155564832,3.37223334824185));
#46208=CARTESIAN_POINT('Ctrl Pts',(372.96029516153,-18.728162535155,3.31091625730226));
#46209=CARTESIAN_POINT('Ctrl Pts',(373.056018165821,-18.7223095138268,3.24538699094666));
#46210=CARTESIAN_POINT('Ctrl Pts',(373.151773095583,-18.716454540403,3.17983586931544));
#46211=CARTESIAN_POINT('Ctrl Pts',(373.244585454973,-18.7105995669792,3.11007001205712));
#46212=CARTESIAN_POINT('Ctrl Pts',(373.334075715332,-18.7047445935554,3.0363958290761));
#46213=CARTESIAN_POINT('Ctrl Pts',(373.423667401406,-18.6988829842713,2.96263814587162));
#46214=CARTESIAN_POINT('Ctrl Pts',(373.509929154253,-18.6930213749871,2.88496355849492));
#46215=CARTESIAN_POINT('Ctrl Pts',(373.592516195857,-18.687159765703,2.80371733644781));
#46216=CARTESIAN_POINT('Ctrl Pts',(373.675158926509,-18.6812942038926,2.72241632947651));
#46217=CARTESIAN_POINT('Ctrl Pts',(373.754121731188,-18.6754286420823,2.63753919395465));
#46218=CARTESIAN_POINT('Ctrl Pts',(373.82909938647,-18.669563080272,2.54946515334626));
#46219=CARTESIAN_POINT('Ctrl Pts',(373.904186677474,-18.6636889415716,2.46126232688874));
#46220=CARTESIAN_POINT('Ctrl Pts',(373.975276936664,-18.6578148028713,2.36985359077235));
#46221=CARTESIAN_POINT('Ctrl Pts',(374.042107549006,-18.651940664171,2.27564809837372));
#46222=CARTESIAN_POINT('Ctrl Pts',(374.05900791985,-18.6504551903896,2.25182506726159));
#46223=CARTESIAN_POINT('Ctrl Pts',(374.075636113491,-18.6489697166083,2.22782330886233));
#46224=CARTESIAN_POINT('Ctrl Pts',(374.091988351211,-18.647484242827,2.20364968326233));
#46225=CARTESIAN_POINT('Ctrl Pts',(374.156646486828,-18.6416105534364,2.10806511623511));
#46226=CARTESIAN_POINT('Ctrl Pts',(374.217201869648,-18.6357368640458,2.00947320297338));
#46227=CARTESIAN_POINT('Ctrl Pts',(374.273362378306,-18.6298631746553,1.90826144815202));
#46228=CARTESIAN_POINT('Ctrl Pts',(374.329450378471,-18.6239970687495,1.80718036721465));
#46229=CARTESIAN_POINT('Ctrl Pts',(374.381154589964,-18.6181309628438,1.70348652928221));
#46230=CARTESIAN_POINT('Ctrl Pts',(374.428225452276,-18.612264856938,1.59759731142581));
#46231=CARTESIAN_POINT('Ctrl Pts',(374.475248114625,-18.60640475785,1.49181652277923));
#46232=CARTESIAN_POINT('Ctrl Pts',(374.517646698153,-18.6005446587619,1.38384520102957));
#46233=CARTESIAN_POINT('Ctrl Pts',(374.555217302689,-18.5946845596739,1.27412569512333));
#46234=CARTESIAN_POINT('Ctrl Pts',(374.594143368923,-18.5886130415798,1.16044775975463));
#46235=CARTESIAN_POINT('Ctrl Pts',(374.627886294788,-18.5825415234857,1.044893512584));
#46236=CARTESIAN_POINT('Ctrl Pts',(374.656273511792,-18.5764700053915,0.927978417820083));
#46237=CARTESIAN_POINT('Ctrl Pts',(374.683640753402,-18.5706166417948,0.815264175847031));
#46238=CARTESIAN_POINT('Ctrl Pts',(374.706030426571,-18.564763278198,0.701285631866943));
#46239=CARTESIAN_POINT('Ctrl Pts',(374.72333875747,-18.5589099146013,0.586519740789697));
#46240=CARTESIAN_POINT('Ctrl Pts',(374.740644489582,-18.5530574298674,0.471771081424861));
#46241=CARTESIAN_POINT('Ctrl Pts',(374.752870334855,-18.5472049451335,0.356235718439138));
#46242=CARTESIAN_POINT('Ctrl Pts',(374.759963948607,-18.5413524603996,0.240399113562284));
#46243=CARTESIAN_POINT('Ctrl Pts',(374.767058212749,-18.5354994390714,0.124551888024065));
#46244=CARTESIAN_POINT('Ctrl Pts',(374.769019284694,-18.5296464177432,0.00840377808418154));
#46245=CARTESIAN_POINT('Ctrl Pts',(374.765846879003,-18.523793396415,-0.107557052120743));
#46246=CARTESIAN_POINT('Ctrl Pts',(374.762673415252,-18.5179384229912,-0.223556557501702));
#46247=CARTESIAN_POINT('Ctrl Pts',(374.754363080696,-18.5120834495674,-0.339368246178464));
#46248=CARTESIAN_POINT('Ctrl Pts',(374.740967607883,-18.5062284761436,-0.454507089516433));
#46249=CARTESIAN_POINT('Ctrl Pts',(374.727556953023,-18.5003668668594,-0.569776427944547));
#46250=CARTESIAN_POINT('Ctrl Pts',(374.709049704376,-18.4945052575753,-0.684370988356086));
#46251=CARTESIAN_POINT('Ctrl Pts',(374.685549087174,-18.4886436482911,-0.797813877198597));
#46252=CARTESIAN_POINT('Ctrl Pts',(374.662032623332,-18.4827780864808,-0.911333261414341));
#46253=CARTESIAN_POINT('Ctrl Pts',(374.633516187737,-18.4769125246704,-1.02369902825722));
#46254=CARTESIAN_POINT('Ctrl Pts',(374.60015298032,-18.4710469628601,-1.13444911544304));
#46255=CARTESIAN_POINT('Ctrl Pts',(374.566740987711,-18.4651728241597,-1.24536114641937));
#46256=CARTESIAN_POINT('Ctrl Pts',(374.528468215096,-18.4592986854594,-1.35465239431463));
#46257=CARTESIAN_POINT('Ctrl Pts',(374.485536111161,-18.4534245467591,-1.4618803757175));
#46258=CARTESIAN_POINT('Ctrl Pts',(374.474679282948,-18.4519390729778,-1.4889965817034));
#46259=CARTESIAN_POINT('Ctrl Pts',(374.463524718943,-18.4504535991966,-1.51598096481221));
#46260=CARTESIAN_POINT('Ctrl Pts',(374.452076135251,-18.4489681254154,-1.54282663083928));
#46261=CARTESIAN_POINT('Ctrl Pts',(374.406807463788,-18.4430944360248,-1.64897667247484));
#46262=CARTESIAN_POINT('Ctrl Pts',(374.356787554373,-18.4372207466342,-1.75330944973641));
#46263=CARTESIAN_POINT('Ctrl Pts',(374.302183668454,-18.4313470572437,-1.85536942077899));
#46264=CARTESIAN_POINT('Ctrl Pts',(374.247650281281,-18.4254809513379,-1.95729762281074));
#46265=CARTESIAN_POINT('Ctrl Pts',(374.188544880369,-18.4196148454322,-2.05695849323815));
#46266=CARTESIAN_POINT('Ctrl Pts',(374.125082901821,-18.4137487395264,-2.15391606032656));
#46267=CARTESIAN_POINT('Ctrl Pts',(374.06168590753,-18.4078886404384,-2.25077434410155));
#46268=CARTESIAN_POINT('Ctrl Pts',(373.993941433975,-18.4020285413504,-2.34493448698738));
#46269=CARTESIAN_POINT('Ctrl Pts',(373.922110654224,-18.3961684422623,-2.43598534849728));
#46270=CARTESIAN_POINT('Ctrl Pts',(373.847688383811,-18.3900969241682,-2.53032111737022));
#46271=CARTESIAN_POINT('Ctrl Pts',(373.768879604177,-18.3840254060741,-2.62131861919105));
#46272=CARTESIAN_POINT('Ctrl Pts',(373.686023912919,-18.37795388798,-2.70855340525163));
#46273=CARTESIAN_POINT('Ctrl Pts',(373.606145292864,-18.3721005243832,-2.79265377573266));
#46274=CARTESIAN_POINT('Ctrl Pts',(373.522505882718,-18.3662471607865,-2.87325684653467));
#46275=CARTESIAN_POINT('Ctrl Pts',(373.435450214655,-18.3603937971898,-2.95001685390382));
#46276=CARTESIAN_POINT('Ctrl Pts',(373.348407617707,-18.3545413124558,-3.02676533601632));
#46277=CARTESIAN_POINT('Ctrl Pts',(373.257950092563,-18.3486888277219,-3.09967162886994));
#46278=CARTESIAN_POINT('Ctrl Pts',(373.164457199974,-18.342836342988,-3.16842857339812));
#46279=CARTESIAN_POINT('Ctrl Pts',(373.070955735342,-18.3369833216598,-3.23719182201521));
#46280=CARTESIAN_POINT('Ctrl Pts',(372.974418682875,-18.3311303003316,-3.30180472124391));
#46281=CARTESIAN_POINT('Ctrl Pts',(372.875256095986,-18.3252772790034,-3.36200239280549));
#46282=CARTESIAN_POINT('Ctrl Pts',(372.776060436461,-18.3194223055796,-3.42222014145301));
#46283=CARTESIAN_POINT('Ctrl Pts',(372.674237854264,-18.3135673321557,-3.47801952003003));
#46284=CARTESIAN_POINT('Ctrl Pts',(372.570223967472,-18.3077123587319,-3.5291810611691));
#46285=CARTESIAN_POINT('Ctrl Pts',(372.466092194301,-18.3018507494477,-3.58040058734349));
#46286=CARTESIAN_POINT('Ctrl Pts',(372.359764530426,-18.2959891401635,-3.62697160218444));
#46287=CARTESIAN_POINT('Ctrl Pts',(372.251697672621,-18.2901275308794,-3.66872231813269));
#46288=CARTESIAN_POINT('Ctrl Pts',(372.143557944541,-18.284261969069,-3.71050118689534));
#46289=CARTESIAN_POINT('Ctrl Pts',(372.03367707795,-18.2783964072587,-3.74745315320763));
#46290=CARTESIAN_POINT('Ctrl Pts',(371.922526398551,-18.2725308454483,-3.7794564638157));
#46291=CARTESIAN_POINT('Ctrl Pts',(371.811213189597,-18.266656706748,-3.81150657111314));
#46292=CARTESIAN_POINT('Ctrl Pts',(371.698626862312,-18.2607825680476,-3.83859348490467));
#46293=CARTESIAN_POINT('Ctrl Pts',(371.585248446229,-18.2549084293473,-3.86064660963543));
#46294=CARTESIAN_POINT('Ctrl Pts',(371.556576895719,-18.2534229555661,-3.86622348485963));
#46295=CARTESIAN_POINT('Ctrl Pts',(371.527854711603,-18.2519374817849,-3.87147870792586));
#46296=CARTESIAN_POINT('Ctrl Pts',(371.49908970167,-18.2504520080037,-3.87641166409268));
#46297=CARTESIAN_POINT('Ctrl Pts',(371.385350411352,-18.2445783186131,-3.89591699139472));
#46298=CARTESIAN_POINT('Ctrl Pts',(371.270562491265,-18.2387046292226,-3.91044465985997));
#46299=CARTESIAN_POINT('Ctrl Pts',(371.155199410817,-18.232830939832,-3.91988826702961));
#46300=CARTESIAN_POINT('Ctrl Pts',(371.039985274945,-18.2269648339262,-3.92931968161521));
#46301=CARTESIAN_POINT('Ctrl Pts',(370.924197863479,-18.2210987280205,-3.9336800551511));
#46302=CARTESIAN_POINT('Ctrl Pts',(370.80832031685,-18.2152326221147,-3.93291407586061));
#46303=CARTESIAN_POINT('Ctrl Pts',(370.692561427353,-18.2093725230267,-3.93214888092315));
#46304=CARTESIAN_POINT('Ctrl Pts',(370.57671299696,-18.2035124239387,-3.92626777720655));
#46305=CARTESIAN_POINT('Ctrl Pts',(370.461262094652,-18.1976523248507,-3.91526734732078));
#46306=CARTESIAN_POINT('Ctrl Pts',(370.341645987175,-18.1915808067566,-3.90387004702072));
#46307=CARTESIAN_POINT('Ctrl Pts',(370.222457083328,-18.1855092886625,-3.88697702228025));
#46308=CARTESIAN_POINT('Ctrl Pts',(370.104236149779,-18.1794377705683,-3.86464354194478));
#46309=CARTESIAN_POINT('Ctrl Pts',(369.990262988853,-18.1735844069716,-3.84311252140624));
#46310=CARTESIAN_POINT('Ctrl Pts',(369.877189876214,-18.1677310433748,-3.81652536002296));
#46311=CARTESIAN_POINT('Ctrl Pts',(369.765494134026,-18.1618776797781,-3.7849841290658));
#46312=CARTESIAN_POINT('Ctrl Pts',(369.653815162578,-18.1560251950442,-3.7534476339183));
#46313=CARTESIAN_POINT('Ctrl Pts',(369.543513547859,-18.1501727103103,-3.71695866046925));
#46314=CARTESIAN_POINT('Ctrl Pts',(369.435053161538,-18.1443202255764,-3.67566964274565));
#46315=CARTESIAN_POINT('Ctrl Pts',(369.326582830856,-18.1384672042482,-3.63437683937355));
#46316=CARTESIAN_POINT('Ctrl Pts',(369.219954450297,-18.1326141829201,-3.58828326384494));
#46317=CARTESIAN_POINT('Ctrl Pts',(369.115612893013,-18.1267611615919,-3.53758989422811));
#46318=CARTESIAN_POINT('Ctrl Pts',(369.011236535803,-18.1209061881681,-3.48687961739333));
#46319=CARTESIAN_POINT('Ctrl Pts',(368.909148889872,-18.1150512147442,-3.43156667638602));
#46320=CARTESIAN_POINT('Ctrl Pts',(368.809770528071,-18.1091962413204,-3.37189814914625));
#46321=CARTESIAN_POINT('Ctrl Pts',(368.710279533662,-18.1033346320362,-3.31216199529506));
#46322=CARTESIAN_POINT('Ctrl Pts',(368.613504306569,-18.0974730227521,-3.24806061504867));
#46323=CARTESIAN_POINT('Ctrl Pts',(368.51983678089,-18.0916114134679,-3.17988464662003));
#46324=CARTESIAN_POINT('Ctrl Pts',(368.426106094512,-18.0857458516576,-3.11166270663559));
#46325=CARTESIAN_POINT('Ctrl Pts',(368.335487604394,-18.0798802898473,-3.03936096456994));
#46326=CARTESIAN_POINT('Ctrl Pts',(368.248339130896,-18.074014728037,-2.96330947551348));
#46327=CARTESIAN_POINT('Ctrl Pts',(368.161063224955,-18.0681405893366,-2.88714678052682));
#46328=CARTESIAN_POINT('Ctrl Pts',(368.077267759909,-18.0622664506363,-2.80722367981215));
#46329=CARTESIAN_POINT('Ctrl Pts',(367.99727282844,-18.056392311936,-2.72390611573736));
#46330=CARTESIAN_POINT('Ctrl Pts',(367.977043416199,-18.0549068381547,-2.70283646395222));
#46331=CARTESIAN_POINT('Ctrl Pts',(367.95705684183,-18.0534213643734,-2.68154989365601));
#46332=CARTESIAN_POINT('Ctrl Pts',(367.937317854584,-18.0519358905921,-2.66005263253901));
#46333=CARTESIAN_POINT('Ctrl Pts',(367.860117706328,-18.0461261297005,-2.57597578884998));
#46334=CARTESIAN_POINT('Ctrl Pts',(367.78643768348,-18.040316368809,-2.48837936147946));
#46335=CARTESIAN_POINT('Ctrl Pts',(367.716621101547,-18.0345066079174,-2.39759378639936));
#46336=CARTESIAN_POINT('Ctrl Pts',(367.646917585048,-18.0287062557239,-2.3069552352809));
#46337=CARTESIAN_POINT('Ctrl Pts',(367.581065314757,-18.0229059035304,-2.21313814581991));
#46338=CARTESIAN_POINT('Ctrl Pts',(367.519370000745,-18.0171055513369,-2.11650885548427));
#46339=CARTESIAN_POINT('Ctrl Pts',(367.457731987188,-18.0113105863081,-2.01996931106288));
#46340=CARTESIAN_POINT('Ctrl Pts',(367.400243484369,-18.0055156212794,-1.92062310980084));
#46341=CARTESIAN_POINT('Ctrl Pts',(367.347169085525,-17.9997206562507,-1.81886845921795));
#46342=CARTESIAN_POINT('Ctrl Pts',(367.294130453419,-17.993929596438,-1.71718238090259));
#46343=CARTESIAN_POINT('Ctrl Pts',(367.245500207612,-17.9881385366253,-1.61309145307366));
#46344=CARTESIAN_POINT('Ctrl Pts',(367.201498406724,-17.9823474768126,-1.50702085889003));
#46345=CARTESIAN_POINT('Ctrl Pts',(367.157515047021,-17.9765588440371,-1.40099471896696));
#46346=CARTESIAN_POINT('Ctrl Pts',(367.118156436423,-17.9707702112616,-1.29299095283894));
#46347=CARTESIAN_POINT('Ctrl Pts',(367.083595280145,-17.9649815784862,-1.18345645454238));
#46348=CARTESIAN_POINT('Ctrl Pts',(367.04903064302,-17.9591923627051,-1.07391092441323));
#46349=CARTESIAN_POINT('Ctrl Pts',(367.019264562183,-17.953403146924,-0.962834754694295));
#46350=CARTESIAN_POINT('Ctrl Pts',(366.994420301154,-17.9476139311429,-0.850691359780153));
#46351=CARTESIAN_POINT('Ctrl Pts',(366.96957484929,-17.9418244378733,-0.738542589612216));
#46352=CARTESIAN_POINT('Ctrl Pts',(366.949651770194,-17.9360349446037,-0.625326907398582));
#46353=CARTESIAN_POINT('Ctrl Pts',(366.934723222317,-17.9302454513341,-0.511518049147073));
#46354=CARTESIAN_POINT('Ctrl Pts',(366.919784200993,-17.9244518963195,-0.397629345815158));
#46355=CARTESIAN_POINT('Ctrl Pts',(366.909846752754,-17.918658341305,-0.283147056364034));
#46356=CARTESIAN_POINT('Ctrl Pts',(366.90493114092,-17.9128647862904,-0.168549889250918));
#46357=CARTESIAN_POINT('Ctrl Pts',(366.902470243282,-17.909964364872,-0.1111792287226));
#46358=CARTESIAN_POINT('Ctrl Pts',(366.901267147452,-17.9070639434535,-0.0537797989658822));
#46359=CARTESIAN_POINT('Ctrl Pts',(366.901319490284,-17.904163522035,0.00358846936293337));
#46360=CARTESIAN_POINT('',(366.901317976443,-16.6541635220067,-0.000984499013828783));
#46361=CARTESIAN_POINT('Ctrl Pts',(366.901319490285,-17.9041635219925,0.0035884702030614));
#46362=CARTESIAN_POINT('Ctrl Pts',(366.901453987089,-17.8967107857687,0.150998280634382));
#46363=CARTESIAN_POINT('Ctrl Pts',(366.909879461701,-17.8892580495449,0.298039224628797));
#46364=CARTESIAN_POINT('Ctrl Pts',(366.926450625096,-17.881805313321,0.443917478055424));
#46365=CARTESIAN_POINT('Ctrl Pts',(366.943372590596,-17.87419480691,0.592883891139391));
#46366=CARTESIAN_POINT('Ctrl Pts',(366.968788773385,-17.866584300499,0.740638106576088));
#46367=CARTESIAN_POINT('Ctrl Pts',(367.00249633415,-17.858973794088,0.886359321021127));
#46368=CARTESIAN_POINT('Ctrl Pts',(367.010696073086,-17.8571224537854,0.921807626648902));
#46369=CARTESIAN_POINT('Ctrl Pts',(367.019386242384,-17.8552711134829,0.9571357292265));
#46370=CARTESIAN_POINT('Ctrl Pts',(367.028563499469,-17.8534197731803,0.992332000328052));
#46371=CARTESIAN_POINT('Ctrl Pts',(367.057679895574,-17.8475460837898,1.10399810724094));
#46372=CARTESIAN_POINT('Ctrl Pts',(367.091763607331,-17.8416723943992,1.21456763442583));
#46373=CARTESIAN_POINT('Ctrl Pts',(367.130716395201,-17.8357987050086,1.3235653516671));
#46374=CARTESIAN_POINT('Ctrl Pts',(367.169618891363,-17.8299325991029,1.43242234261545));
#46375=CARTESIAN_POINT('Ctrl Pts',(367.213377824216,-17.8240664931971,1.5397111738462));
#46376=CARTESIAN_POINT('Ctrl Pts',(367.261844419909,-17.8182003872913,1.64496886543682));
#46377=CARTESIAN_POINT('Ctrl Pts',(367.310261386425,-17.8123402882033,1.7501187744923));
#46378=CARTESIAN_POINT('Ctrl Pts',(367.363376255463,-17.8064801891153,1.85324130788109));
#46379=CARTESIAN_POINT('Ctrl Pts',(367.420991353868,-17.8006200900272,1.9538912991242));
#46380=CARTESIAN_POINT('Ctrl Pts',(367.480685073582,-17.7945485719331,2.05817251243197));
#46381=CARTESIAN_POINT('Ctrl Pts',(367.545209717467,-17.788477053839,2.15979898249089));
#46382=CARTESIAN_POINT('Ctrl Pts',(367.6142920086,-17.7824055357449,2.25830081254818));
#46383=CARTESIAN_POINT('Ctrl Pts',(367.680892117804,-17.7765521721482,2.35326339313078));
#46384=CARTESIAN_POINT('Ctrl Pts',(367.751727733438,-17.7706988085514,2.44532164376651));
#46385=CARTESIAN_POINT('Ctrl Pts',(367.826509091948,-17.7648454449547,2.53408276415557));
#46386=CARTESIAN_POINT('Ctrl Pts',(367.901279222288,-17.7589929602208,2.62283055736104));
#46387=CARTESIAN_POINT('Ctrl Pts',(367.979993651387,-17.7531404754869,2.70828188879846));
#46388=CARTESIAN_POINT('Ctrl Pts',(368.062322276064,-17.747287990753,2.790076973885));
#46389=CARTESIAN_POINT('Ctrl Pts',(368.14465844917,-17.7414349694248,2.87187955848261));
#46390=CARTESIAN_POINT('Ctrl Pts',(368.23060918349,-17.7355819480967,2.95002493912365));
#46391=CARTESIAN_POINT('Ctrl Pts',(368.319807980291,-17.7297289267685,3.02419065188109));
#46392=CARTESIAN_POINT('Ctrl Pts',(368.409036526614,-17.7238739533447,3.09838110033589));
#46393=CARTESIAN_POINT('Ctrl Pts',(368.501514971988,-17.7180189799209,3.16858897764201));
#46394=CARTESIAN_POINT('Ctrl Pts',(368.596844834535,-17.7121640064971,3.23453296329477));
#46395=CARTESIAN_POINT('Ctrl Pts',(368.692282741237,-17.706302397213,3.30055168798519));
#46396=CARTESIAN_POINT('Ctrl Pts',(368.790578175458,-17.7004407879289,3.36229664032803));
#46397=CARTESIAN_POINT('Ctrl Pts',(368.891304774407,-17.6945791786447,3.41953054900028));
#46398=CARTESIAN_POINT('Ctrl Pts',(368.992099294042,-17.6887136168344,3.47680305091751));
#46399=CARTESIAN_POINT('Ctrl Pts',(369.095327875743,-17.682848055024,3.52955826466164));
#46400=CARTESIAN_POINT('Ctrl Pts',(369.200542307743,-17.6769824932137,3.57760624817583));
#46401=CARTESIAN_POINT('Ctrl Pts',(369.305910589047,-17.6711083545134,3.6257244896264));
#46402=CARTESIAN_POINT('Ctrl Pts',(369.413270134343,-17.6652342158131,3.66912160962348));
#46403=CARTESIAN_POINT('Ctrl Pts',(369.522155588414,-17.6593600771127,3.70765683293493));
#46404=CARTESIAN_POINT('Ctrl Pts',(369.549690942181,-17.6578746033314,3.71740176181834));
#46405=CARTESIAN_POINT('Ctrl Pts',(369.577323819415,-17.6563891295501,3.72683602521239));
#46406=CARTESIAN_POINT('Ctrl Pts',(369.6050465884,-17.6549036557688,3.73595786345068));
#46407=CARTESIAN_POINT('Ctrl Pts',(369.714664769561,-17.6490299663783,3.77202638593624));
#46408=CARTESIAN_POINT('Ctrl Pts',(369.82605431523,-17.6431562769877,3.80332636779954));
#46409=CARTESIAN_POINT('Ctrl Pts',(369.938762629141,-17.6372825875971,3.82968273367613));
#46410=CARTESIAN_POINT('Ctrl Pts',(370.051325426029,-17.6314164816914,3.8560050710083));
#46411=CARTESIAN_POINT('Ctrl Pts',(370.165203206521,-17.6255503757856,3.87739639218186));
#46412=CARTESIAN_POINT('Ctrl Pts',(370.279926273235,-17.6196842698798,3.89373072721228));
#46413=CARTESIAN_POINT('Ctrl Pts',(370.394531864989,-17.6138241707918,3.91004833609172));
#46414=CARTESIAN_POINT('Ctrl Pts',(370.509980614702,-17.6079640717038,3.92131920098443));
#46415=CARTESIAN_POINT('Ctrl Pts',(370.625791284987,-17.6021039726157,3.92746809921346));
#46416=CARTESIAN_POINT('Ctrl Pts',(370.74578014005,-17.5960324545216,3.9338388356627));
#46417=CARTESIAN_POINT('Ctrl Pts',(370.866157083469,-17.5899609364275,3.93471094705701));
#46418=CARTESIAN_POINT('Ctrl Pts',(370.986379111295,-17.5838894183334,3.93005933464035));
#46419=CARTESIAN_POINT('Ctrl Pts',(371.102281465584,-17.5780360547366,3.92557485837528));
#46420=CARTESIAN_POINT('Ctrl Pts',(371.218039396946,-17.5721826911399,3.91595678793277));
#46421=CARTESIAN_POINT('Ctrl Pts',(371.33316574863,-17.5663293275431,3.9012356731232));
#46422=CARTESIAN_POINT('Ctrl Pts',(371.44827481448,-17.5604768428092,3.88651676863947));
#46423=CARTESIAN_POINT('Ctrl Pts',(371.562752079509,-17.5546243580753,3.86669639567965));
#46424=CARTESIAN_POINT('Ctrl Pts',(371.676116261836,-17.5487718733413,3.84185689989346));
#46425=CARTESIAN_POINT('Ctrl Pts',(371.789490838136,-17.5429188520131,3.81701512665902));
#46426=CARTESIAN_POINT('Ctrl Pts',(371.901751725264,-17.537065830685,3.78715340422332));
#46427=CARTESIAN_POINT('Ctrl Pts',(372.012429271805,-17.5312128093568,3.75240489358614));
#46428=CARTESIAN_POINT('Ctrl Pts',(372.123143731444,-17.5253578359329,3.7176447936496));
#46429=CARTESIAN_POINT('Ctrl Pts',(372.232273406481,-17.5195028625091,3.67799478833975));
#46430=CARTESIAN_POINT('Ctrl Pts',(372.339365880272,-17.5136478890852,3.63363721858418));
#46431=CARTESIAN_POINT('Ctrl Pts',(372.446579729625,-17.5077862798011,3.58922937522082));
#46432=CARTESIAN_POINT('Ctrl Pts',(372.551751387384,-17.5019246705169,3.54010347642277));
#46433=CARTESIAN_POINT('Ctrl Pts',(372.65445033727,-17.4960630612327,3.48648917114653));
#46434=CARTESIAN_POINT('Ctrl Pts',(372.757218537811,-17.4901974994224,3.43283871335054));
#46435=CARTESIAN_POINT('Ctrl Pts',(372.857510353849,-17.484331937612,3.37469402921715));
#46436=CARTESIAN_POINT('Ctrl Pts',(372.954923195721,-17.4784663758017,3.3123287852164));
#46437=CARTESIAN_POINT('Ctrl Pts',(373.05247847906,-17.4725922371013,3.24987234793281));
#46438=CARTESIAN_POINT('Ctrl Pts',(373.147146050141,-17.466718098401,3.18318327104919));
#46439=CARTESIAN_POINT('Ctrl Pts',(373.238555340947,-17.4608439597007,3.11257628061211));
#46440=CARTESIAN_POINT('Ctrl Pts',(373.261671258322,-17.4593584859195,3.09472092539933));
#46441=CARTESIAN_POINT('Ctrl Pts',(373.284578989448,-17.4578730121383,3.07661520573558));
#46442=CARTESIAN_POINT('Ctrl Pts',(373.307272918438,-17.4563875383571,3.05826458067883));
#46443=CARTESIAN_POINT('Ctrl Pts',(373.397006639506,-17.4505138489665,2.98570465194085));
#46444=CARTESIAN_POINT('Ctrl Pts',(373.483693592017,-17.4446401595759,2.90907116048099));
#46445=CARTESIAN_POINT('Ctrl Pts',(373.566941302027,-17.4387664701854,2.82864951647443));
#46446=CARTESIAN_POINT('Ctrl Pts',(373.650081531423,-17.4329003642796,2.7483317043656));
#46447=CARTESIAN_POINT('Ctrl Pts',(373.729791054364,-17.4270342583739,2.66423575045738));
#46448=CARTESIAN_POINT('Ctrl Pts',(373.805709389867,-17.4211681524681,2.57668805561883));
#46449=CARTESIAN_POINT('Ctrl Pts',(373.881549985961,-17.4153080533801,2.48923000850444));
#46450=CARTESIAN_POINT('Ctrl Pts',(373.953606847428,-17.4094479542921,2.39832756122708));
#46451=CARTESIAN_POINT('Ctrl Pts',(374.021555880699,-17.403587855204,2.30434432240852));
#46452=CARTESIAN_POINT('Ctrl Pts',(374.091956360075,-17.3975163371099,2.20697038274338));
#46453=CARTESIAN_POINT('Ctrl Pts',(374.157946688056,-17.3914448190158,2.10628947244759));
#46454=CARTESIAN_POINT('Ctrl Pts',(374.219211406358,-17.3853733009217,2.00274427572518));
#46455=CARTESIAN_POINT('Ctrl Pts',(374.27827483437,-17.379519937325,1.90291954067239));
#46456=CARTESIAN_POINT('Ctrl Pts',(374.332946169868,-17.3736665737282,1.80043319510798));
#46457=CARTESIAN_POINT('Ctrl Pts',(374.38298699179,-17.3678132101315,1.69571116201729));
#46458=CARTESIAN_POINT('Ctrl Pts',(374.43302030025,-17.3619607253976,1.59100485258745));
#46459=CARTESIAN_POINT('Ctrl Pts',(374.478424299484,-17.3561082406637,1.48406389576369));
#46460=CARTESIAN_POINT('Ctrl Pts',(374.519007277702,-17.3502557559298,1.37533735684865));
#46461=CARTESIAN_POINT('Ctrl Pts',(374.559593976833,-17.3444027346017,1.26660084916981));
#46462=CARTESIAN_POINT('Ctrl Pts',(374.595358631766,-17.3385497132735,1.156078821034));
#46463=CARTESIAN_POINT('Ctrl Pts',(374.626158536234,-17.3326966919453,1.0442381120572));
#46464=CARTESIAN_POINT('Ctrl Pts',(374.656968713064,-17.3268417185215,0.932360102044108));
#46465=CARTESIAN_POINT('Ctrl Pts',(374.682810737231,-17.3209867450977,0.819162934758138));
#46466=CARTESIAN_POINT('Ctrl Pts',(374.703592571882,-17.3151317716739,0.705125628206122));
#46467=CARTESIAN_POINT('Ctrl Pts',(374.724397960073,-17.3092701623897,0.590959075014662));
#46468=CARTESIAN_POINT('Ctrl Pts',(374.740131637772,-17.3034085531056,0.475950888721588));
#46469=CARTESIAN_POINT('Ctrl Pts',(374.750753193829,-17.2975469438215,0.360587330416915));
#46470=CARTESIAN_POINT('Ctrl Pts',(374.76138191208,-17.2916813820111,0.245145981617632));
#46471=CARTESIAN_POINT('Ctrl Pts',(374.766891625081,-17.2858158202008,0.129349195307191));
#46472=CARTESIAN_POINT('Ctrl Pts',(374.767294049227,-17.2799502583904,0.013683627934948));
#46473=CARTESIAN_POINT('Ctrl Pts',(374.767697061816,-17.2740761196901,-0.102151070865607));
#46474=CARTESIAN_POINT('Ctrl Pts',(374.762977897856,-17.2682019809898,-0.217853756580347));
#46475=CARTESIAN_POINT('Ctrl Pts',(374.753200135664,-17.2623278422895,-0.332942422010732));
#46476=CARTESIAN_POINT('Ctrl Pts',(374.750727499229,-17.2608423685082,-0.362046466662447));
#46477=CARTESIAN_POINT('Ctrl Pts',(374.747931619835,-17.2593568947268,-0.391111295725008));
#46478=CARTESIAN_POINT('Ctrl Pts',(374.744814040346,-17.2578714209455,-0.420129230717538));
#46479=CARTESIAN_POINT('Ctrl Pts',(374.732486866484,-17.2519977315549,-0.534868608177085));
#46480=CARTESIAN_POINT('Ctrl Pts',(374.715084963688,-17.2461240421644,-0.649256079204849));
#46481=CARTESIAN_POINT('Ctrl Pts',(374.692635400511,-17.2402503527738,-0.762807121295351));
#46482=CARTESIAN_POINT('Ctrl Pts',(374.670214821828,-17.234384246868,-0.876211558322815));
#46483=CARTESIAN_POINT('Ctrl Pts',(374.642759622345,-17.2285181409623,-0.98878131239848));
#46484=CARTESIAN_POINT('Ctrl Pts',(374.610348659104,-17.2226520350565,-1.10003652350676));
#46485=CARTESIAN_POINT('Ctrl Pts',(374.577970884275,-17.2167919359685,-1.21117781069622));
#46486=CARTESIAN_POINT('Ctrl Pts',(374.540647554432,-17.2109318368804,-1.3210068380751));
#46487=CARTESIAN_POINT('Ctrl Pts',(374.498508518548,-17.2050717377924,-1.42905415158215));
#46488=CARTESIAN_POINT('Ctrl Pts',(374.454849202383,-17.1990002196983,-1.54099956566508));
#46489=CARTESIAN_POINT('Ctrl Pts',(374.406020227831,-17.1929287016042,-1.65103183515607));
#46490=CARTESIAN_POINT('Ctrl Pts',(374.352222572966,-17.1868571835101,-1.75864589466433));
#46491=CARTESIAN_POINT('Ctrl Pts',(374.300357910833,-17.1810038199133,-1.8623932950115));
#46492=CARTESIAN_POINT('Ctrl Pts',(374.243875681377,-17.1751504563166,-1.96389286992713));
#46493=CARTESIAN_POINT('Ctrl Pts',(374.183004540698,-17.1692970927198,-2.06271337541898));
#46494=CARTESIAN_POINT('Ctrl Pts',(374.122142539616,-17.1634446079859,-2.16151904334446));
#46495=CARTESIAN_POINT('Ctrl Pts',(374.056893154232,-17.157592123252,-2.25764609000586));
#46496=CARTESIAN_POINT('Ctrl Pts',(373.987529808859,-17.1517396385181,-2.35068997590965));
#46497=CARTESIAN_POINT('Ctrl Pts',(373.918160103798,-17.1458866171899,-2.44374239268857));
#46498=CARTESIAN_POINT('Ctrl Pts',(373.844675935864,-17.1400335958617,-2.5337107555099));
#46499=CARTESIAN_POINT('Ctrl Pts',(373.767392231623,-17.1341805745335,-2.62022206898151));
#46500=CARTESIAN_POINT('Ctrl Pts',(373.690082751775,-17.1283256011097,-2.70676223564684));
#46501=CARTESIAN_POINT('Ctrl Pts',(373.608971490908,-17.1224706276859,-2.78984275234716));
#46502=CARTESIAN_POINT('Ctrl Pts',(373.524411077558,-17.1166156542621,-2.86912659957516));
#46503=CARTESIAN_POINT('Ctrl Pts',(373.439754825842,-17.1107540449779,-2.94850030486038));
#46504=CARTESIAN_POINT('Ctrl Pts',(373.35164192073,-17.1048924356937,-3.02406846932926));
#46505=CARTESIAN_POINT('Ctrl Pts',(373.260459063966,-17.0990308264096,-3.09553352841481));
#46506=CARTESIAN_POINT('Ctrl Pts',(373.169214721931,-17.0931652645992,-3.16704677691452));
#46507=CARTESIAN_POINT('Ctrl Pts',(373.074896641534,-17.0872997027889,-3.23445117118757));
#46508=CARTESIAN_POINT('Ctrl Pts',(372.977920115577,-17.0814341409785,-3.29749273552443));
#46509=CARTESIAN_POINT('Ctrl Pts',(372.880801786154,-17.0755600022782,-3.3606264820903));
#46510=CARTESIAN_POINT('Ctrl Pts',(372.781017607738,-17.0696858635779,-3.41938445795735));
#46511=CARTESIAN_POINT('Ctrl Pts',(372.679007081172,-17.0638117248775,-3.47355878779874));
#46512=CARTESIAN_POINT('Ctrl Pts',(372.653210284338,-17.0623262510963,-3.48725859141288));
#46513=CARTESIAN_POINT('Ctrl Pts',(372.627271207589,-17.060840777315,-3.50066551228831));
#46514=CARTESIAN_POINT('Ctrl Pts',(372.601197139614,-17.0593553035338,-3.51377668432798));
#46515=CARTESIAN_POINT('Ctrl Pts',(372.498098062157,-17.0534816141432,-3.56561937120597));
#46516=CARTESIAN_POINT('Ctrl Pts',(372.392543635615,-17.0476079247526,-3.61300695171475));
#46517=CARTESIAN_POINT('Ctrl Pts',(372.284955682171,-17.041734235362,-3.65569950751248));
#46518=CARTESIAN_POINT('Ctrl Pts',(372.177506634883,-17.0358681294563,-3.69833694320987));
#46519=CARTESIAN_POINT('Ctrl Pts',(372.068029662409,-17.0300020235505,-3.73629125797415));
#46520=CARTESIAN_POINT('Ctrl Pts',(371.956970744038,-17.0241359176448,-3.7693685793176));
#46521=CARTESIAN_POINT('Ctrl Pts',(371.846025548585,-17.0182758185567,-3.80241202990538));
#46522=CARTESIAN_POINT('Ctrl Pts',(371.733502022937,-17.0124157194687,-3.83058830328173));
#46523=CARTESIAN_POINT('Ctrl Pts',(371.61986504539,-17.0065556203807,-3.85375201704524));
#46524=CARTESIAN_POINT('Ctrl Pts',(371.50212830494,-17.0004841022865,-3.87775142475645));
#46525=CARTESIAN_POINT('Ctrl Pts',(371.383196673924,-16.9944125841924,-3.89636959407857));
#46526=CARTESIAN_POINT('Ctrl Pts',(371.263603514877,-16.9883410660983,-3.90950160771155));
#46527=CARTESIAN_POINT('Ctrl Pts',(371.148307433611,-16.9824877025016,-3.92216177759986));
#46528=CARTESIAN_POINT('Ctrl Pts',(371.03239699053,-16.9766343389048,-3.92972320188549));
#46529=CARTESIAN_POINT('Ctrl Pts',(370.916358519993,-16.9707809753081,-3.93214424061429));
#46530=CARTESIAN_POINT('Ctrl Pts',(370.800337472241,-16.9649284905742,-3.93456491583227));
#46531=CARTESIAN_POINT('Ctrl Pts',(370.684188848199,-16.9590760058403,-3.93184673152903));
#46532=CARTESIAN_POINT('Ctrl Pts',(370.568400811497,-16.9532235211064,-3.92400014359316));
#46533=CARTESIAN_POINT('Ctrl Pts',(370.452602158587,-16.9473704997782,-3.91615283623052));
#46534=CARTESIAN_POINT('Ctrl Pts',(370.337164570962,-16.94151747845,-3.90317621844518));
#46535=CARTESIAN_POINT('Ctrl Pts',(370.222572204265,-16.9356644571218,-3.88513272115385));
#46536=CARTESIAN_POINT('Ctrl Pts',(370.107941618801,-16.929809483698,-3.86708320600773));
#46537=CARTESIAN_POINT('Ctrl Pts',(369.994157222702,-16.9239545102742,-3.84396351528716));
#46538=CARTESIAN_POINT('Ctrl Pts',(369.881693379389,-16.9180995368504,-3.81588726403835));
#46539=CARTESIAN_POINT('Ctrl Pts',(369.769102072754,-16.9122379275662,-3.78777919196498));
#46540=CARTESIAN_POINT('Ctrl Pts',(369.657834707248,-16.9063763182821,-3.75470344704786));
#46541=CARTESIAN_POINT('Ctrl Pts',(369.548350963405,-16.9005147089979,-3.7168236652132));
#46542=CARTESIAN_POINT('Ctrl Pts',(369.438793393869,-16.8946491471876,-3.67891834076345));
#46543=CARTESIAN_POINT('Ctrl Pts',(369.331022223981,-16.8887835853773,-3.63620268089129));
#46544=CARTESIAN_POINT('Ctrl Pts',(369.225476005703,-16.8829180235669,-3.58888797675068));
#46545=CARTESIAN_POINT('Ctrl Pts',(369.119775452967,-16.8770438848666,-3.54150408690794));
#46546=CARTESIAN_POINT('Ctrl Pts',(369.016306712592,-16.8711697461663,-3.48950791632338));
#46547=CARTESIAN_POINT('Ctrl Pts',(368.915482721435,-16.8652956074659,-3.43315608981197));
#46548=CARTESIAN_POINT('Ctrl Pts',(368.889985980036,-16.8638101336847,-3.41890563283775));
#46549=CARTESIAN_POINT('Ctrl Pts',(368.864658219004,-16.8623246599034,-3.40437684241616));
#46550=CARTESIAN_POINT('Ctrl Pts',(368.839505798013,-16.8608391861221,-3.38957428955112));
#46551=CARTESIAN_POINT('Ctrl Pts',(368.740050990944,-16.8549654967315,-3.3310437393572));
#46552=CARTESIAN_POINT('Ctrl Pts',(368.643008776625,-16.849091807341,-3.26803478452446));
#46553=CARTESIAN_POINT('Ctrl Pts',(368.548809434139,-16.8432181179504,-3.20077182352843));
#46554=CARTESIAN_POINT('Ctrl Pts',(368.454731711855,-16.8373520120447,-3.13359570533412));
#46555=CARTESIAN_POINT('Ctrl Pts',(368.363489895308,-16.8314859061389,-3.06217674129353));
#46556=CARTESIAN_POINT('Ctrl Pts',(368.275488666688,-16.8256198002332,-2.98678459118322));
#46557=CARTESIAN_POINT('Ctrl Pts',(368.187577550204,-16.8197597011451,-2.91146964167412));
#46558=CARTESIAN_POINT('Ctrl Pts',(368.102900733115,-16.8138996020571,-2.83218986585944));
#46559=CARTESIAN_POINT('Ctrl Pts',(368.021832396338,-16.8080395029691,-2.74925709143536));
#46560=CARTESIAN_POINT('Ctrl Pts',(367.937839298918,-16.801967984875,-2.66333229171));
#46561=CARTESIAN_POINT('Ctrl Pts',(367.857720336802,-16.7958964667808,-2.57348619555311));
#46562=CARTESIAN_POINT('Ctrl Pts',(367.781852813725,-16.7898249486867,-2.48011011502305));
#46563=CARTESIAN_POINT('Ctrl Pts',(367.708711271385,-16.78397158509,-2.39008911169083));
#46564=CARTESIAN_POINT('Ctrl Pts',(367.639521193603,-16.7781182214932,-2.29678777681932));
#46565=CARTESIAN_POINT('Ctrl Pts',(367.574581217239,-16.7722648578965,-2.20059220757036));
#46566=CARTESIAN_POINT('Ctrl Pts',(367.509650991395,-16.7664123731626,-2.1044110817624));
#46567=CARTESIAN_POINT('Ctrl Pts',(367.448969829211,-16.7605598884287,-2.00533692797415));
#46568=CARTESIAN_POINT('Ctrl Pts',(367.39279358267,-16.7547074036948,-1.90378562217243));
#46569=CARTESIAN_POINT('Ctrl Pts',(367.336612185522,-16.7488543823666,-1.80222500547942));
#46570=CARTESIAN_POINT('Ctrl Pts',(367.284936725098,-16.7430013610385,-1.69818714681387));
#46571=CARTESIAN_POINT('Ctrl Pts',(367.237977205588,-16.7371483397103,-1.59211273035536));
#46572=CARTESIAN_POINT('Ctrl Pts',(367.191002024171,-16.7312933662865,-1.48600293603049));
#46573=CARTESIAN_POINT('Ctrl Pts',(367.148746078379,-16.7254383928627,-1.37785561086782));
#46574=CARTESIAN_POINT('Ctrl Pts',(367.111371053518,-16.7195834194389,-1.26813095796898));
#46575=CARTESIAN_POINT('Ctrl Pts',(367.073953668867,-16.7137218101547,-1.15828194626963));
#46576=CARTESIAN_POINT('Ctrl Pts',(367.041428379768,-16.7078602008705,-1.04685242999428));
#46577=CARTESIAN_POINT('Ctrl Pts',(367.013906878856,-16.7019985915864,-0.934317390893775));
#46578=CARTESIAN_POINT('Ctrl Pts',(366.986366819993,-16.696133029776,-0.821706468590008));
#46579=CARTESIAN_POINT('Ctrl Pts',(366.963837347974,-16.6902674679657,-0.707988943345657));
#46580=CARTESIAN_POINT('Ctrl Pts',(366.946378656372,-16.6844019061554,-0.593647876758552));
#46581=CARTESIAN_POINT('Ctrl Pts',(366.92889443588,-16.6785277674551,-0.479139615488192));
#46582=CARTESIAN_POINT('Ctrl Pts',(366.916495837798,-16.6726536287547,-0.364006402401481));
#46583=CARTESIAN_POINT('Ctrl Pts',(366.909191075276,-16.6667794900544,-0.248734350331171));
#46584=CARTESIAN_POINT('Ctrl Pts',(366.907343820085,-16.6652940162731,-0.219583930192212));
#46585=CARTESIAN_POINT('Ctrl Pts',(366.905822056539,-16.6638085424918,-0.19042461837385));
#46586=CARTESIAN_POINT('Ctrl Pts',(366.904625391226,-16.6623230687105,-0.161264236942553));
#46587=CARTESIAN_POINT('Ctrl Pts',(366.902434340218,-16.6596032198186,-0.107872630763614));
#46588=CARTESIAN_POINT('Ctrl Pts',(366.901331356318,-16.6568833709268,-0.0544360677886615));
#46589=CARTESIAN_POINT('Ctrl Pts',(366.901317976443,-16.654163522035,-0.000984499569211797));
#46590=CARTESIAN_POINT('',(366.90131898798,-15.4041635220771,-0.00298763949216439));
#46591=CARTESIAN_POINT('Ctrl Pts',(366.901317976443,-16.6541635220067,-0.000984499013828783));
#46592=CARTESIAN_POINT('Ctrl Pts',(366.901289272163,-16.6483285386861,0.113686948345892));
#46593=CARTESIAN_POINT('Ctrl Pts',(366.906279900742,-16.6424935553654,0.228559854945339));
#46594=CARTESIAN_POINT('Ctrl Pts',(366.916316614802,-16.6366585720448,0.343154915056637));
#46595=CARTESIAN_POINT('Ctrl Pts',(366.926340568907,-16.6308310069019,0.457604287256876));
#46596=CARTESIAN_POINT('Ctrl Pts',(366.941397817925,-16.625003441759,0.571776101619367));
#46597=CARTESIAN_POINT('Ctrl Pts',(366.9614631222,-16.6191758766162,0.68518992431947));
#46598=CARTESIAN_POINT('Ctrl Pts',(366.981508457437,-16.6133541110802,0.79849087730859));
#46599=CARTESIAN_POINT('Ctrl Pts',(367.006551864193,-16.6075323455443,0.911034928450505));
#46600=CARTESIAN_POINT('Ctrl Pts',(367.036516271438,-16.6017105800084,1.02234639207432));
#46601=CARTESIAN_POINT('Ctrl Pts',(367.066460120965,-16.5958928086184,1.13358148810336));
#46602=CARTESIAN_POINT('Ctrl Pts',(367.101318148562,-16.5900750372285,1.24358527486813));
#46603=CARTESIAN_POINT('Ctrl Pts',(367.140962274659,-16.5842572658385,1.35189258829449));
#46604=CARTESIAN_POINT('Ctrl Pts',(367.180592203786,-16.5784415778525,1.46016111575435));
#46605=CARTESIAN_POINT('Ctrl Pts',(367.22500468116,-16.5726258898665,1.56673398421441));
#46606=CARTESIAN_POINT('Ctrl Pts',(367.274022078907,-16.5668102018805,1.67116217028183));
#46607=CARTESIAN_POINT('Ctrl Pts',(367.323034171011,-16.5609951433846,1.77557905304157));
#46608=CARTESIAN_POINT('Ctrl Pts',(367.376650014403,-16.5551800848887,1.87785133560505));
#46609=CARTESIAN_POINT('Ctrl Pts',(367.434644568087,-16.5493650263928,1.97755165655074));
#46610=CARTESIAN_POINT('Ctrl Pts',(367.492647335919,-16.5435491442721,2.07726609870441));
#46611=CARTESIAN_POINT('Ctrl Pts',(367.555029835655,-16.5377332621515,2.17440749309849));
#46612=CARTESIAN_POINT('Ctrl Pts',(367.621522377866,-16.5319173800309,2.26857537532211));
#46613=CARTESIAN_POINT('Ctrl Pts',(367.688083066218,-16.5260955373933,2.36283976728419));
#46614=CARTESIAN_POINT('Ctrl Pts',(367.758761967659,-16.5202736947556,2.45412421762823));
#46615=CARTESIAN_POINT('Ctrl Pts',(367.833247496876,-16.514451852118,2.54205934554102));
#46616=CARTESIAN_POINT('Ctrl Pts',(367.907771530795,-16.5086269999252,2.63003993081756));
#46617=CARTESIAN_POINT('Ctrl Pts',(367.986105826632,-16.5028021477324,2.71466743813535));
#46618=CARTESIAN_POINT('Ctrl Pts',(368.06790144736,-16.4969772955396,2.79560892640024));
#46619=CARTESIAN_POINT('Ctrl Pts',(368.149831300989,-16.4911428843166,2.87668324586925));
#46620=CARTESIAN_POINT('Ctrl Pts',(368.235233516678,-16.4853084730937,2.95405918018264));
#46621=CARTESIAN_POINT('Ctrl Pts',(368.323725223505,-16.4794740618707,3.02744341773692));
#46622=CARTESIAN_POINT('Ctrl Pts',(368.40293397897,-16.4742516916801,3.09312950670421));
#46623=CARTESIAN_POINT('Ctrl Pts',(368.484617425624,-16.4690293214894,3.15561790045603));
#46624=CARTESIAN_POINT('Ctrl Pts',(368.568482590461,-16.4638069512988,3.21472853628711));
#46625=CARTESIAN_POINT('Ctrl Pts',(368.662807180821,-16.4579332619082,3.28121128298605));
#46626=CARTESIAN_POINT('Ctrl Pts',(368.760217391912,-16.4520595725177,3.34364981695612));
#46627=CARTESIAN_POINT('Ctrl Pts',(368.860331403367,-16.4461858831271,3.40174462530376));
#46628=CARTESIAN_POINT('Ctrl Pts',(368.960316158229,-16.4403197772213,3.45976442779601));
#46629=CARTESIAN_POINT('Ctrl Pts',(369.062997417204,-16.4344536713156,3.51345145198798));
#46630=CARTESIAN_POINT('Ctrl Pts',(369.167962675288,-16.4285875654098,3.56254816402064));
#46631=CARTESIAN_POINT('Ctrl Pts',(369.272820450285,-16.4227274663218,3.61159460164553));
#46632=CARTESIAN_POINT('Ctrl Pts',(369.379957200345,-16.4168673672338,3.65605990263528));
#46633=CARTESIAN_POINT('Ctrl Pts',(369.488934575887,-16.4110072681458,3.69573170523251));
#46634=CARTESIAN_POINT('Ctrl Pts',(369.601843606521,-16.4049357500516,3.73683477596164));
#46635=CARTESIAN_POINT('Ctrl Pts',(369.716728190647,-16.3988642319575,3.77279171431088));
#46636=CARTESIAN_POINT('Ctrl Pts',(369.833076274915,-16.3927927138634,3.80342007959482));
#46637=CARTESIAN_POINT('Ctrl Pts',(369.945243879532,-16.3869393502667,3.83294794323654));
#46638=CARTESIAN_POINT('Ctrl Pts',(370.058771190997,-16.3810859866699,3.85752344941448));
#46639=CARTESIAN_POINT('Ctrl Pts',(370.173183336342,-16.3752326230732,3.87703367932067));
#46640=CARTESIAN_POINT('Ctrl Pts',(370.287578303087,-16.3693801383393,3.8965409798315));
#46641=CARTESIAN_POINT('Ctrl Pts',(370.40285743239,-16.3635276536054,3.91098444686748));
#46642=CARTESIAN_POINT('Ctrl Pts',(370.518536357881,-16.3576751688715,3.92030241782428));
#46643=CARTESIAN_POINT('Ctrl Pts',(370.634225889576,-16.3518221475433,3.92962124311391));
#46644=CARTESIAN_POINT('Ctrl Pts',(370.750314878494,-16.3459691262151,3.9338136049559));
#46645=CARTESIAN_POINT('Ctrl Pts',(370.866315256099,-16.3401161048869,3.93286983845248));
#46646=CARTESIAN_POINT('Ctrl Pts',(370.98235432207,-16.3342611314631,3.93192575718471));
#46647=CARTESIAN_POINT('Ctrl Pts',(371.098304305053,-16.3284061580393,3.92584214471083));
#46648=CARTESIAN_POINT('Ctrl Pts',(371.213679271971,-16.3225511846155,3.91466140476619));
#46649=CARTESIAN_POINT('Ctrl Pts',(371.329185001595,-16.3166895753313,3.90346799288891));
#46650=CARTESIAN_POINT('Ctrl Pts',(371.444114002938,-16.3108279660472,3.8871659629905));
#46651=CARTESIAN_POINT('Ctrl Pts',(371.557987487129,-16.304966356763,3.86584935828651));
#46652=CARTESIAN_POINT('Ctrl Pts',(371.671937757046,-16.2991007949527,3.84451837963943));
#46653=CARTESIAN_POINT('Ctrl Pts',(371.78483069124,-16.2932352331423,3.8181661868216));
#46654=CARTESIAN_POINT('Ctrl Pts',(371.896201369164,-16.287369671332,3.78693707349024));
#46655=CARTESIAN_POINT('Ctrl Pts',(372.007734898335,-16.2814955326316,3.75566229553574));
#46656=CARTESIAN_POINT('Ctrl Pts',(372.117741337905,-16.2756213939313,3.71949649341316));
#46657=CARTESIAN_POINT('Ctrl Pts',(372.225774415544,-16.269747255231,3.67863257681136));
#46658=CARTESIAN_POINT('Ctrl Pts',(372.253094217225,-16.2682617814497,3.66829875941133));
#46659=CARTESIAN_POINT('Ctrl Pts',(372.280287941014,-16.2667763076684,3.65766472835757));
#46660=CARTESIAN_POINT('Ctrl Pts',(372.307348622577,-16.2652908338872,3.64673406660523));
#46661=CARTESIAN_POINT('Ctrl Pts',(372.414348853888,-16.2594171444966,3.60351330244472));
#46662=CARTESIAN_POINT('Ctrl Pts',(372.519623445852,-16.2535434551061,3.55550726078602));
#46663=CARTESIAN_POINT('Ctrl Pts',(372.622713726984,-16.2476697657155,3.50287441949009));
#46664=CARTESIAN_POINT('Ctrl Pts',(372.725670908878,-16.2418036598097,3.45030953213686));
#46665=CARTESIAN_POINT('Ctrl Pts',(372.826449023692,-16.235937553904,3.39312991089134));
#46666=CARTESIAN_POINT('Ctrl Pts',(372.924608040818,-16.2300714479982,3.33154257539175));
#46667=CARTESIAN_POINT('Ctrl Pts',(373.022666544361,-16.2242113489102,3.27001830453916));
#46668=CARTESIAN_POINT('Ctrl Pts',(373.118110936897,-16.2183512498221,3.20409551531621));
#46669=CARTESIAN_POINT('Ctrl Pts',(373.210525135698,-16.2124911507341,3.13402743298718));
#46670=CARTESIAN_POINT('Ctrl Pts',(373.306273427962,-16.20641963264,3.06143145409861));
#46671=CARTESIAN_POINT('Ctrl Pts',(373.398768351141,-16.2003481145459,2.98438563480101));
#46672=CARTESIAN_POINT('Ctrl Pts',(373.487579009906,-16.1942765964518,2.90322135471013));
#46673=CARTESIAN_POINT('Ctrl Pts',(373.573198630725,-16.188423232855,2.82497337206782));
#46674=CARTESIAN_POINT('Ctrl Pts',(373.65539385672,-16.1825698692583,2.7428980970087));
#46675=CARTESIAN_POINT('Ctrl Pts',(373.733812368177,-16.1767165056615,2.65733335465462));
#46676=CARTESIAN_POINT('Ctrl Pts',(373.812219105358,-16.1708640209276,2.57178145955866));
#46677=CARTESIAN_POINT('Ctrl Pts',(373.886849976465,-16.1650115361937,2.4827414434387));
#46678=CARTESIAN_POINT('Ctrl Pts',(373.957390586312,-16.1591590514598,2.39058689527163));
#46679=CARTESIAN_POINT('Ctrl Pts',(374.027937663785,-16.1533060301316,2.29842389776959));
#46680=CARTESIAN_POINT('Ctrl Pts',(374.094393483355,-16.1474530088034,2.20314612863588));
#46681=CARTESIAN_POINT('Ctrl Pts',(374.156485336937,-16.1415999874752,2.10515847625797));
#46682=CARTESIAN_POINT('Ctrl Pts',(374.218597899351,-16.1357450140514,2.0071381431058));
#46683=CARTESIAN_POINT('Ctrl Pts',(374.276343380626,-16.1298900406276,1.90640647833789));
#46684=CARTESIAN_POINT('Ctrl Pts',(374.329493984012,-16.1240350672038,1.80339480280124));
#46685=CARTESIAN_POINT('Ctrl Pts',(374.38270482678,-16.1181734579196,1.70026637676184));
#46686=CARTESIAN_POINT('Ctrl Pts',(374.431310207849,-16.1123118486355,1.59485314960579));
#46687=CARTESIAN_POINT('Ctrl Pts',(374.475129596472,-16.1064502393513,1.48760843309944));
#46688=CARTESIAN_POINT('Ctrl Pts',(374.51897853283,-16.100584677541,1.38029140069316));
#46689=CARTESIAN_POINT('Ctrl Pts',(374.558034911766,-16.0947191157306,1.27114080783373));
#46690=CARTESIAN_POINT('Ctrl Pts',(374.592167946523,-16.0888535539203,1.16062555386829));
#46691=CARTESIAN_POINT('Ctrl Pts',(374.626350892148,-16.08297941522,1.04994869949578));
#46692=CARTESIAN_POINT('Ctrl Pts',(374.655596021987,-16.0771052765196,0.937903599777784));
#46693=CARTESIAN_POINT('Ctrl Pts',(374.679823511091,-16.0712311378193,0.824969839033651));
#46694=CARTESIAN_POINT('Ctrl Pts',(374.685950247568,-16.069745664038,0.796410734599247));
#46695=CARTESIAN_POINT('Ctrl Pts',(374.691756364132,-16.0682601902568,0.767794825730232));
#46696=CARTESIAN_POINT('Ctrl Pts',(374.697241096136,-16.0667747164755,0.739129906964046));
#46697=CARTESIAN_POINT('Ctrl Pts',(374.718928191924,-16.0609010270849,0.625786385616273));
#46698=CARTESIAN_POINT('Ctrl Pts',(374.735658695976,-16.0550273376944,0.51129878810818));
#46699=CARTESIAN_POINT('Ctrl Pts',(374.747317128308,-16.0491536483038,0.396138452044766));
#46700=CARTESIAN_POINT('Ctrl Pts',(374.758960508509,-16.043287542398,0.281126798793892));
#46701=CARTESIAN_POINT('Ctrl Pts',(374.765544798619,-16.0374214364923,0.165444541575756));
#46702=CARTESIAN_POINT('Ctrl Pts',(374.767005414085,-16.0315553305865,0.0495736688790276));
#46703=CARTESIAN_POINT('Ctrl Pts',(374.7684645339,-16.0256952314985,-0.0661785535205626));
#46704=CARTESIAN_POINT('Ctrl Pts',(374.764810409773,-16.0198351324104,-0.182118596570821));
#46705=CARTESIAN_POINT('Ctrl Pts',(374.756030266475,-16.0139750333223,-0.297759546865992));
#46706=CARTESIAN_POINT('Ctrl Pts',(374.746933355639,-16.0079035152282,-0.417572558827964));
#46707=CARTESIAN_POINT('Ctrl Pts',(374.732333526664,-16.0018319971341,-0.537064040026449));
#46708=CARTESIAN_POINT('Ctrl Pts',(374.712275647986,-15.99576047904,-0.655692261693141));
#46709=CARTESIAN_POINT('Ctrl Pts',(374.692938464919,-15.9899071154433,-0.770058076550187));
#46710=CARTESIAN_POINT('Ctrl Pts',(374.668528780996,-15.9840537518465,-0.883621157184588));
#46711=CARTESIAN_POINT('Ctrl Pts',(374.639139477452,-15.9782003882498,-0.995902308365154));
#46712=CARTESIAN_POINT('Ctrl Pts',(374.609754586613,-15.9723479035159,-1.1081666009087));
#46713=CARTESIAN_POINT('Ctrl Pts',(374.575391667394,-15.966495418782,-1.21914894714273));
#46714=CARTESIAN_POINT('Ctrl Pts',(374.536194212923,-15.9606429340481,-1.32838263218773));
#46715=CARTESIAN_POINT('Ctrl Pts',(374.496993164573,-15.9547899127199,-1.43762633249508));
#46716=CARTESIAN_POINT('Ctrl Pts',(374.452956839356,-15.9489368913917,-1.54512066400708));
#46717=CARTESIAN_POINT('Ctrl Pts',(374.404277630517,-15.9430838700635,-1.65041697413445));
#46718=CARTESIAN_POINT('Ctrl Pts',(374.355582186221,-15.9372288966397,-1.75574840261525));
#46719=CARTESIAN_POINT('Ctrl Pts',(374.302240952471,-15.9313739232158,-1.85887997720267));
#46720=CARTESIAN_POINT('Ctrl Pts',(374.244492880775,-15.925518949792,-1.95938645536516));
#46721=CARTESIAN_POINT('Ctrl Pts',(374.186679359057,-15.9196573405078,-2.06000684471049));
#46722=CARTESIAN_POINT('Ctrl Pts',(374.124449236442,-15.9137957312236,-2.1579958408669));
#46723=CARTESIAN_POINT('Ctrl Pts',(374.05808556693,-15.9079341219395,-2.25295599780995));
#46724=CARTESIAN_POINT('Ctrl Pts',(373.991677147908,-15.9020685601292,-2.34798018708392));
#46725=CARTESIAN_POINT('Ctrl Pts',(373.921129882688,-15.8962029983188,-2.43997114330849));
#46726=CARTESIAN_POINT('Ctrl Pts',(373.846766890326,-15.8903374365085,-2.52856477054929));
#46727=CARTESIAN_POINT('Ctrl Pts',(373.77229516103,-15.8844632978082,-2.61728794340256));
#46728=CARTESIAN_POINT('Ctrl Pts',(373.693996847533,-15.8785891591078,-2.70260356971809));
#46729=CARTESIAN_POINT('Ctrl Pts',(373.612231674436,-15.8727150204075,-2.78418458474306));
#46730=CARTESIAN_POINT('Ctrl Pts',(373.591554596987,-15.8712295466263,-2.80481509162167));
#46731=CARTESIAN_POINT('Ctrl Pts',(373.570655975222,-15.8697440728451,-2.82520697329511));
#46732=CARTESIAN_POINT('Ctrl Pts',(373.549541944429,-15.8682585990639,-2.84535536173276));
#46733=CARTESIAN_POINT('Ctrl Pts',(373.466055274903,-15.8623849096733,-2.92502379943988));
#46734=CARTESIAN_POINT('Ctrl Pts',(373.37892021368,-15.8565112202828,-3.00114738878447));
#46735=CARTESIAN_POINT('Ctrl Pts',(373.28847022665,-15.8506375308922,-3.07337357443036));
#46736=CARTESIAN_POINT('Ctrl Pts',(373.198137019051,-15.8447714249864,-3.14550650928519));
#46737=CARTESIAN_POINT('Ctrl Pts',(373.10449771682,-15.8389053190807,-3.2137517918253));
#46738=CARTESIAN_POINT('Ctrl Pts',(373.007922326767,-15.8330392131749,-3.27779386060109));
#46739=CARTESIAN_POINT('Ctrl Pts',(372.911445828683,-15.8271791140869,-3.34177035111417));
#46740=CARTESIAN_POINT('Ctrl Pts',(372.81203956526,-15.8213190149989,-3.40155196197912));
#46741=CARTESIAN_POINT('Ctrl Pts',(372.71010576808,-15.8154589159109,-3.4568639976836));
#46742=CARTESIAN_POINT('Ctrl Pts',(372.604494432045,-15.8093873978168,-3.51417156544958));
#46743=CARTESIAN_POINT('Ctrl Pts',(372.496170096574,-15.8033158797227,-3.56668068303658));
#46744=CARTESIAN_POINT('Ctrl Pts',(372.385612304205,-15.7972443616286,-3.614135377425));
#46745=CARTESIAN_POINT('Ctrl Pts',(372.279026941672,-15.7913909980318,-3.65988498671914));
#46746=CARTESIAN_POINT('Ctrl Pts',(372.170366272047,-15.7855376344351,-3.70093696388265));
#46747=CARTESIAN_POINT('Ctrl Pts',(372.060083318644,-15.7796842708383,-3.73710958145248));
#46748=CARTESIAN_POINT('Ctrl Pts',(371.949816923855,-15.7738317861044,-3.77327676782547));
#46749=CARTESIAN_POINT('Ctrl Pts',(371.837929122079,-15.7679793013705,-3.80456592260049));
#46750=CARTESIAN_POINT('Ctrl Pts',(371.724889886481,-15.7621268166366,-3.83084461360422));
#46751=CARTESIAN_POINT('Ctrl Pts',(371.611840286703,-15.7562737953084,-3.85712571401107));
#46752=CARTESIAN_POINT('Ctrl Pts',(371.497639445674,-15.7504207739803,-3.87839534386183));
#46753=CARTESIAN_POINT('Ctrl Pts',(371.382768667892,-15.7445677526521,-3.89457195387243));
#46754=CARTESIAN_POINT('Ctrl Pts',(371.267859578487,-15.7387127792283,-3.91075395909494));
#46755=CARTESIAN_POINT('Ctrl Pts',(371.152280516923,-15.7328578058044,-3.92183950926487));
#46756=CARTESIAN_POINT('Ctrl Pts',(371.036518355719,-15.7270028323806,-3.92779886918752));
#46757=CARTESIAN_POINT('Ctrl Pts',(370.920624992975,-15.7211412230964,-3.93376498327917));
#46758=CARTESIAN_POINT('Ctrl Pts',(370.804548529225,-15.7152796138123,-3.93459328970434));
#46759=CARTESIAN_POINT('Ctrl Pts',(370.688776387746,-15.7094180045281,-3.93030618168947));
#46760=CARTESIAN_POINT('Ctrl Pts',(370.572926180261,-15.7035524427178,-3.92601618284617));
#46761=CARTESIAN_POINT('Ctrl Pts',(370.457381114422,-15.6976868809075,-3.91660393457932));
#46762=CARTESIAN_POINT('Ctrl Pts',(370.342622308813,-15.6918213190971,-3.90214357649819));
#46763=CARTESIAN_POINT('Ctrl Pts',(370.227695697683,-15.6859471803968,-3.88766207382693));
#46764=CARTESIAN_POINT('Ctrl Pts',(370.113558046959,-15.6800730416965,-3.86811779903562));
#46765=CARTESIAN_POINT('Ctrl Pts',(370.000679201845,-15.6741989029962,-3.84363572661713));
#46766=CARTESIAN_POINT('Ctrl Pts',(369.972133984676,-15.6727134292148,-3.83744461017511));
#46767=CARTESIAN_POINT('Ctrl Pts',(369.943669184858,-15.6712279554335,-3.83093796731186));
#46768=CARTESIAN_POINT('Ctrl Pts',(369.915292219035,-15.6697424816522,-3.82411831455342));
#46769=CARTESIAN_POINT('Ctrl Pts',(369.803087288063,-15.6638687922616,-3.79715282882214));
#46770=CARTESIAN_POINT('Ctrl Pts',(369.691883293148,-15.6579951028711,-3.76519987490573));
#46771=CARTESIAN_POINT('Ctrl Pts',(369.582157264336,-15.6521214134805,-3.72834854320739));
#46772=CARTESIAN_POINT('Ctrl Pts',(369.472572902136,-15.6462553075748,-3.69154479004025));
#46773=CARTESIAN_POINT('Ctrl Pts',(369.364463099339,-15.640389201669,-3.64985536631524));
#46774=CARTESIAN_POINT('Ctrl Pts',(369.258293608919,-15.6345230957633,-3.60342012279473));
#46775=CARTESIAN_POINT('Ctrl Pts',(369.152232834704,-15.6286629966752,-3.55703242837201));
#46776=CARTESIAN_POINT('Ctrl Pts',(369.048108797119,-15.6228028975872,-3.505908744989));
#46777=CARTESIAN_POINT('Ctrl Pts',(368.946370378527,-15.6169427984991,-3.45023815595173));
#46778=CARTESIAN_POINT('Ctrl Pts',(368.840961469895,-15.610871280405,-3.39255909906695));
#46779=CARTESIAN_POINT('Ctrl Pts',(368.738113993804,-15.6047997623109,-3.32999900198542));
#46780=CARTESIAN_POINT('Ctrl Pts',(368.638303010963,-15.5987282442168,-3.26282206265844));
#46781=CARTESIAN_POINT('Ctrl Pts',(368.542078316503,-15.5928748806201,-3.19805884444795));
#46782=CARTESIAN_POINT('Ctrl Pts',(368.448676035473,-15.5870215170233,-3.12900509834564));
#46783=CARTESIAN_POINT('Ctrl Pts',(368.358494463133,-15.5811681534266,-3.05594298721042));
#46784=CARTESIAN_POINT('Ctrl Pts',(368.268326431253,-15.5753156686927,-2.98289184610529));
#46785=CARTESIAN_POINT('Ctrl Pts',(368.181378467454,-15.5694631839588,-2.90583379666114));
#46786=CARTESIAN_POINT('Ctrl Pts',(368.098016632455,-15.5636106992249,-2.82509196827603));
#46787=CARTESIAN_POINT('Ctrl Pts',(368.014647154295,-15.5577576778967,-2.74434273694954));
#46788=CARTESIAN_POINT('Ctrl Pts',(367.934864755337,-15.5519046565686,-2.6599093427132));
#46789=CARTESIAN_POINT('Ctrl Pts',(367.858998881832,-15.5460516352404,-2.57215202087127));
#46790=CARTESIAN_POINT('Ctrl Pts',(367.783107705592,-15.5401966618165,-2.48436543026701));
#46791=CARTESIAN_POINT('Ctrl Pts',(367.711135922245,-15.5343416883927,-2.39325302004321));
#46792=CARTESIAN_POINT('Ctrl Pts',(367.643372456735,-15.5284867149688,-2.29920779326774));
#46793=CARTESIAN_POINT('Ctrl Pts',(367.57553219004,-15.5226251056847,-2.20505597830778));
#46794=CARTESIAN_POINT('Ctrl Pts',(367.511910002647,-15.5167634964005,-2.10796504773326));
#46795=CARTESIAN_POINT('Ctrl Pts',(367.452751314148,-15.5109018871163,-2.00835672673068));
#46796=CARTESIAN_POINT('Ctrl Pts',(367.393552734511,-15.505036325306,-1.90868123910544));
#46797=CARTESIAN_POINT('Ctrl Pts',(367.338823841448,-15.4991707634956,-1.80648534426908));
#46798=CARTESIAN_POINT('Ctrl Pts',(367.288763153824,-15.4933052016852,-1.7022135217306));
#46799=CARTESIAN_POINT('Ctrl Pts',(367.238629265197,-15.4874310629849,-1.59778922821404));
#46800=CARTESIAN_POINT('Ctrl Pts',(367.19317736665,-15.4815569242846,-1.49128332739846));
#46801=CARTESIAN_POINT('Ctrl Pts',(367.152557148692,-15.4756827855843,-1.38315838375919));
#46802=CARTESIAN_POINT('Ctrl Pts',(367.142284958701,-15.4741973118031,-1.3558153506665));
#46803=CARTESIAN_POINT('Ctrl Pts',(367.132321503048,-15.4727118380218,-1.32836884303118));
#46804=CARTESIAN_POINT('Ctrl Pts',(367.12266868771,-15.4712263642406,-1.30082645734926));
#46805=CARTESIAN_POINT('Ctrl Pts',(367.078037802287,-15.464358107902,-1.17348111646888));
#46806=CARTESIAN_POINT('Ctrl Pts',(367.039929871042,-15.4574898515634,-1.04373804609832));
#46807=CARTESIAN_POINT('Ctrl Pts',(367.008570512254,-15.4506215952247,-0.912220523260835));
#46808=CARTESIAN_POINT('Ctrl Pts',(366.977357634567,-15.4437854208482,-0.781317325219555));
#46809=CARTESIAN_POINT('Ctrl Pts',(366.952830523815,-15.4369492464716,-0.648656316079149));
#46810=CARTESIAN_POINT('Ctrl Pts',(366.935164839185,-15.430113072095,-0.514873550602358));
#46811=CARTESIAN_POINT('Ctrl Pts',(366.917647225344,-15.4233341973793,-0.382212129705779));
#46812=CARTESIAN_POINT('Ctrl Pts',(366.906876582261,-15.4165553226636,-0.248447798149102));
#46813=CARTESIAN_POINT('Ctrl Pts',(366.902976767002,-15.4097764479478,-0.11422024244691));
#46814=CARTESIAN_POINT('Ctrl Pts',(366.901900414615,-15.4079054726576,-0.07717332086797));
#46815=CARTESIAN_POINT('Ctrl Pts',(366.901347173121,-15.4060344973673,-0.0400912217293683));
#46816=CARTESIAN_POINT('Ctrl Pts',(366.90131898798,-15.4041635220771,-0.00298763949216487));
#46817=CARTESIAN_POINT('',(366.901318718745,-14.1541635219903,0.00260925113160348));
#46818=CARTESIAN_POINT('Ctrl Pts',(366.901318987979,-15.404163522035,-0.00298763865733689));
#46819=CARTESIAN_POINT('Ctrl Pts',(366.901230807502,-15.3983099575575,0.113095247154288));
#46820=CARTESIAN_POINT('Ctrl Pts',(366.906286231407,-15.39245639308,0.229234623628663));
#46821=CARTESIAN_POINT('Ctrl Pts',(366.916473529392,-15.3866028286025,0.344941812805038));
#46822=CARTESIAN_POINT('Ctrl Pts',(366.926659429648,-15.3807500672531,0.460633126580709));
#46823=CARTESIAN_POINT('Ctrl Pts',(366.94197576806,-15.3748973059036,0.575891960223361));
#46824=CARTESIAN_POINT('Ctrl Pts',(366.962358825895,-15.3690445445541,0.690233504465105));
#46825=CARTESIAN_POINT('Ctrl Pts',(366.982743993784,-15.3631911773267,0.804586885343415));
#46826=CARTESIAN_POINT('Ctrl Pts',(367.008196851816,-15.3573378100994,0.918022381936605));
#46827=CARTESIAN_POINT('Ctrl Pts',(367.038602447749,-15.351484442872,1.03006483322241));
#46828=CARTESIAN_POINT('Ctrl Pts',(367.069018510601,-15.3456290606631,1.14214585435476));
#46829=CARTESIAN_POINT('Ctrl Pts',(367.104390594125,-15.3397736784542,1.25283247866511));
#46830=CARTESIAN_POINT('Ctrl Pts',(367.144553925521,-15.3339182962453,1.36166484783184));
#46831=CARTESIAN_POINT('Ctrl Pts',(367.184765537014,-15.3280558753168,1.47062804373068));
#46832=CARTESIAN_POINT('Ctrl Pts',(367.229779751747,-15.3221934543884,1.57773214729682));
#46833=CARTESIAN_POINT('Ctrl Pts',(367.279383620603,-15.31633103346,1.68253725121945));
#46834=CARTESIAN_POINT('Ctrl Pts',(367.329021195188,-15.3104646290284,1.78741356999753));
#46835=CARTESIAN_POINT('Ctrl Pts',(367.383254441836,-15.3045982245969,1.88998741450882));
#46836=CARTESIAN_POINT('Ctrl Pts',(367.441825313054,-15.2987318201653,1.98984506052449));
#46837=CARTESIAN_POINT('Ctrl Pts',(367.500489987237,-15.2928560205154,2.08986263148266));
#46838=CARTESIAN_POINT('Ctrl Pts',(367.563505932161,-15.2869802208654,2.18715497353206));
#46839=CARTESIAN_POINT('Ctrl Pts',(367.63057266669,-15.2811044212155,2.28133859384338));
#46840=CARTESIAN_POINT('Ctrl Pts',(367.662509872331,-15.2783063630866,2.32618887127282));
#46841=CARTESIAN_POINT('Ctrl Pts',(367.695365085426,-15.2755083049578,2.37033469463753));
#46842=CARTESIAN_POINT('Ctrl Pts',(367.72910285911,-15.2727102468289,2.41373752515242));
#46843=CARTESIAN_POINT('Ctrl Pts',(367.799925263156,-15.2668365574383,2.50484883641647));
#46844=CARTESIAN_POINT('Ctrl Pts',(367.874879018075,-15.2609628680478,2.59299221037365));
#46845=CARTESIAN_POINT('Ctrl Pts',(367.953686307312,-15.2550891786572,2.6777697617046));
#46846=CARTESIAN_POINT('Ctrl Pts',(368.032391848936,-15.2492230727515,2.76243785725226));
#46847=CARTESIAN_POINT('Ctrl Pts',(368.114940751969,-15.2433569668457,2.84374847229937));
#46848=CARTESIAN_POINT('Ctrl Pts',(368.201013602022,-15.23749086094,2.9213349209912));
#46849=CARTESIAN_POINT('Ctrl Pts',(368.286998314574,-15.231630761852,2.99884192214788));
#46850=CARTESIAN_POINT('Ctrl Pts',(368.376499491537,-15.225770662764,3.07263206734134));
#46851=CARTESIAN_POINT('Ctrl Pts',(368.469159818497,-15.2199105636759,3.14237433651128));
#46852=CARTESIAN_POINT('Ctrl Pts',(368.565163118662,-15.2138390455818,3.2146327476456));
#46853=CARTESIAN_POINT('Ctrl Pts',(368.664557514951,-15.2077675274877,3.28254536113834));
#46854=CARTESIAN_POINT('Ctrl Pts',(368.766906466049,-15.2016960093936,3.34578827127157));
#46855=CARTESIAN_POINT('Ctrl Pts',(368.865577937538,-15.1958426457969,3.40675881310102));
#46856=CARTESIAN_POINT('Ctrl Pts',(368.966994917187,-15.1899892822001,3.46338921298559));
#46857=CARTESIAN_POINT('Ctrl Pts',(369.070736141624,-15.1841359186034,3.51543291025592));
#46858=CARTESIAN_POINT('Ctrl Pts',(369.174461789665,-15.1782834338695,3.56746879334026));
#46859=CARTESIAN_POINT('Ctrl Pts',(369.280510619413,-15.1724309491356,3.61491915795378));
#46860=CARTESIAN_POINT('Ctrl Pts',(369.388437331984,-15.1665784644017,3.65758369942494));
#46861=CARTESIAN_POINT('Ctrl Pts',(369.496373939986,-15.1607254430735,3.70025215266173));
#46862=CARTESIAN_POINT('Ctrl Pts',(369.606188388848,-15.1548724217454,3.73813375857935));
#46863=CARTESIAN_POINT('Ctrl Pts',(369.71741666707,-15.1490194004172,3.77107686747001));
#46864=CARTESIAN_POINT('Ctrl Pts',(369.828682042071,-15.1431644269934,3.80403096352368));
#46865=CARTESIAN_POINT('Ctrl Pts',(369.941361788145,-15.1373094535696,3.83204317013469));
#46866=CARTESIAN_POINT('Ctrl Pts',(370.054978744096,-15.1314544801458,3.85501226366195));
#46867=CARTESIAN_POINT('Ctrl Pts',(370.168724470273,-15.1255928708616,3.87800738970641));
#46868=CARTESIAN_POINT('Ctrl Pts',(370.283409121249,-15.1197312615775,3.89594791252033));
#46869=CARTESIAN_POINT('Ctrl Pts',(370.398547302153,-15.1138696522934,3.9087840854694));
#46870=CARTESIAN_POINT('Ctrl Pts',(370.513763121577,-15.108004090483,3.92162891394418));
#46871=CARTESIAN_POINT('Ctrl Pts',(370.629432668677,-15.1021385286727,3.92936251147359));
#46872=CARTESIAN_POINT('Ctrl Pts',(370.745069151725,-15.0962729668624,3.93198724174949));
#46873=CARTESIAN_POINT('Ctrl Pts',(370.860874723673,-15.0903988281621,3.93461581002482));
#46874=CARTESIAN_POINT('Ctrl Pts',(370.976646723617,-15.0845246894618,3.93212061084049));
#46875=CARTESIAN_POINT('Ctrl Pts',(371.091902011755,-15.0786505507614,3.92455594956598));
#46876=CARTESIAN_POINT('Ctrl Pts',(371.121048192571,-15.07716507698,3.9226429702235));
#46877=CARTESIAN_POINT('Ctrl Pts',(371.150161375778,-15.0756796031986,3.92040605411145));
#46878=CARTESIAN_POINT('Ctrl Pts',(371.179233854668,-15.0741941294172,3.91784659627555));
#46879=CARTESIAN_POINT('Ctrl Pts',(371.294188903319,-15.0683204400266,3.90772628279413));
#46880=CARTESIAN_POINT('Ctrl Pts',(371.408889615562,-15.062446750636,3.89252541571288));
#46881=CARTESIAN_POINT('Ctrl Pts',(371.522851038245,-15.0565730612454,3.872261749046));
#46882=CARTESIAN_POINT('Ctrl Pts',(371.636665326025,-15.0507069553397,3.85202424467645));
#46883=CARTESIAN_POINT('Ctrl Pts',(371.749741819369,-15.0448408494339,3.82673701144267));
#46884=CARTESIAN_POINT('Ctrl Pts',(371.861599231695,-15.0389747435281,3.79646967187226));
#46885=CARTESIAN_POINT('Ctrl Pts',(371.973342103457,-15.0331146444401,3.76623332567197));
#46886=CARTESIAN_POINT('Ctrl Pts',(372.083867980788,-15.027254545352,3.73102712386354));
#46887=CARTESIAN_POINT('Ctrl Pts',(372.192705001393,-15.0213944462639,3.69097187143041));
#46888=CARTESIAN_POINT('Ctrl Pts',(372.305468613403,-15.0153229281698,3.64947151687038));
#46889=CARTESIAN_POINT('Ctrl Pts',(372.416418763014,-15.0092514100757,3.60276569939196));
#46890=CARTESIAN_POINT('Ctrl Pts',(372.52504661651,-15.0031798919816,3.55104565571842));
#46891=CARTESIAN_POINT('Ctrl Pts',(372.629771384418,-14.9973265283849,3.50118395454752));
#46892=CARTESIAN_POINT('Ctrl Pts',(372.732337463077,-14.9914731647881,3.4466623490975));
#46893=CARTESIAN_POINT('Ctrl Pts',(372.832309294742,-14.9856198011914,3.38770116740256));
#46894=CARTESIAN_POINT('Ctrl Pts',(372.932266115973,-14.9797673164574,3.32874883853065));
#46895=CARTESIAN_POINT('Ctrl Pts',(373.029629108948,-14.9739148317235,3.26535846866416));
#46896=CARTESIAN_POINT('Ctrl Pts',(373.123988555321,-14.9680623469896,3.19779565888131));
#46897=CARTESIAN_POINT('Ctrl Pts',(373.218356653188,-14.9622093256614,3.13022665449567));
#46898=CARTESIAN_POINT('Ctrl Pts',(373.30972032108,-14.9563563043332,3.05848469024007));
#46899=CARTESIAN_POINT('Ctrl Pts',(373.39770058151,-14.950503283005,2.98287746786997));
#46900=CARTESIAN_POINT('Ctrl Pts',(373.485710185055,-14.9446483095812,2.90724502903149));
#46901=CARTESIAN_POINT('Ctrl Pts',(373.570333824133,-14.9387933361573,2.82774503781185));
#46902=CARTESIAN_POINT('Ctrl Pts',(373.6512277661,-14.9329383627335,2.74472358221049));
#46903=CARTESIAN_POINT('Ctrl Pts',(373.73221339096,-14.9270767534493,2.66160803245279));
#46904=CARTESIAN_POINT('Ctrl Pts',(373.809460593124,-14.9212151441652,2.57496334833301));
#46905=CARTESIAN_POINT('Ctrl Pts',(373.882664432929,-14.915353534881,2.48517044284681));
#46906=CARTESIAN_POINT('Ctrl Pts',(373.955917634621,-14.9094879730707,2.39531698934497));
#46907=CARTESIAN_POINT('Ctrl Pts',(374.025121798929,-14.9036224112603,2.30231141800824));
#46908=CARTESIAN_POINT('Ctrl Pts',(374.090015017657,-14.8977568494499,2.20656406512561));
#46909=CARTESIAN_POINT('Ctrl Pts',(374.155003126186,-14.8918827107496,2.11067670612951));
#46910=CARTESIAN_POINT('Ctrl Pts',(374.215667493009,-14.8860085720492,2.01203991487935));
#46911=CARTESIAN_POINT('Ctrl Pts',(374.271791836672,-14.8801344333489,1.91108911699985));
#46912=CARTESIAN_POINT('Ctrl Pts',(374.285984766946,-14.8786489595678,1.88556030825338));
#46913=CARTESIAN_POINT('Ctrl Pts',(374.299887602293,-14.8771634857867,1.85988361845331));
#46914=CARTESIAN_POINT('Ctrl Pts',(374.313497337101,-14.8756780120056,1.83406627987418));
#46915=CARTESIAN_POINT('Ctrl Pts',(374.367311383478,-14.869804322615,1.73198233222461));
#46916=CARTESIAN_POINT('Ctrl Pts',(374.416718322612,-14.8639306332244,1.62735788902665));
#46917=CARTESIAN_POINT('Ctrl Pts',(374.461470175623,-14.8580569438339,1.52061008483956));
#46918=CARTESIAN_POINT('Ctrl Pts',(374.506164249788,-14.8521908379281,1.41400010209652));
#46919=CARTESIAN_POINT('Ctrl Pts',(374.54621503178,-14.8463247320224,1.30527258776348));
#46920=CARTESIAN_POINT('Ctrl Pts',(374.581420115924,-14.8404586261167,1.19486971376396));
#46921=CARTESIAN_POINT('Ctrl Pts',(374.61658915051,-14.8345985270286,1.08457989090077));
#46922=CARTESIAN_POINT('Ctrl Pts',(374.646922232174,-14.8287384279406,0.972618512013859));
#46923=CARTESIAN_POINT('Ctrl Pts',(374.672265073252,-14.8228783288526,0.859447576224516));
#46924=CARTESIAN_POINT('Ctrl Pts',(374.69852222622,-14.8168068107585,0.742193691255936));
#46925=CARTESIAN_POINT('Ctrl Pts',(374.719422092635,-14.8107352926643,0.623641742014381));
#46926=CARTESIAN_POINT('Ctrl Pts',(374.734849526619,-14.8046637745702,0.50432297671088));
#46927=CARTESIAN_POINT('Ctrl Pts',(374.749722640572,-14.7988104109735,0.389291430001907));
#46928=CARTESIAN_POINT('Ctrl Pts',(374.759509754418,-14.7929570473767,0.273547668377663));
#46929=CARTESIAN_POINT('Ctrl Pts',(374.764159891538,-14.78710368378,0.157577136353263));
#46930=CARTESIAN_POINT('Ctrl Pts',(374.768809330455,-14.7812511990461,0.0416240169141522));
#46931=CARTESIAN_POINT('Ctrl Pts',(374.768323309732,-14.7753987143122,-0.0745553925209104));
#46932=CARTESIAN_POINT('Ctrl Pts',(374.762702903824,-14.7695462295783,-0.190472817539133));
#46933=CARTESIAN_POINT('Ctrl Pts',(374.757081982601,-14.7636932082501,-0.30640087062888));
#46934=CARTESIAN_POINT('Ctrl Pts',(374.746325760388,-14.7578401869219,-0.422066478868533));
#46935=CARTESIAN_POINT('Ctrl Pts',(374.730487354086,-14.7519871655937,-0.536984376453905));
#46936=CARTESIAN_POINT('Ctrl Pts',(374.714643665369,-14.7461321921699,-0.651940601378014));
#46937=CARTESIAN_POINT('Ctrl Pts',(374.693714478494,-14.740277218746,-0.766148210719741));
#46938=CARTESIAN_POINT('Ctrl Pts',(374.66780427319,-14.7344222453222,-0.879130745645707));
#46939=CARTESIAN_POINT('Ctrl Pts',(374.641864701995,-14.728560636038,-0.992241331762467));
#46940=CARTESIAN_POINT('Ctrl Pts',(374.610932937003,-14.7226990267539,-1.10412366925524));
#46941=CARTESIAN_POINT('Ctrl Pts',(374.575163751701,-14.7168374174697,-1.21431501837412));
#46942=CARTESIAN_POINT('Ctrl Pts',(374.539370446974,-14.7109718556594,-1.32458067032894));
#46943=CARTESIAN_POINT('Ctrl Pts',(374.498733371219,-14.705106293849,-1.43315267745457));
#46944=CARTESIAN_POINT('Ctrl Pts',(374.453455350315,-14.6992407320387,-1.53958850903295));
#46945=CARTESIAN_POINT('Ctrl Pts',(374.40811112184,-14.6933665933384,-1.64617997590203));
#46946=CARTESIAN_POINT('Ctrl Pts',(374.358112582364,-14.687492454638,-1.75062866206103));
#46947=CARTESIAN_POINT('Ctrl Pts',(374.303708375224,-14.6816183159377,-1.85251677613444));
#46948=CARTESIAN_POINT('Ctrl Pts',(374.289950439393,-14.6801328421564,-1.8782826168477));
#46949=CARTESIAN_POINT('Ctrl Pts',(374.275910974734,-14.6786473683752,-1.90388485624279));
#46950=CARTESIAN_POINT('Ctrl Pts',(374.261594429211,-14.6771618945939,-1.92931704799581));
#46951=CARTESIAN_POINT('Ctrl Pts',(374.204985593295,-14.6712882052033,-2.02987809239845));
#46952=CARTESIAN_POINT('Ctrl Pts',(374.143852824281,-14.6654145158128,-2.12811303680021));
#46953=CARTESIAN_POINT('Ctrl Pts',(374.078412211903,-14.6595408264222,-2.2235873699914));
#46954=CARTESIAN_POINT('Ctrl Pts',(374.013056089504,-14.6536747205165,-2.31893843684897));
#46955=CARTESIAN_POINT('Ctrl Pts',(373.943403415844,-14.6478086146107,-2.41153564287199));
#46956=CARTESIAN_POINT('Ctrl Pts',(373.869716025419,-14.641942508705,-2.50096919937757));
#46957=CARTESIAN_POINT('Ctrl Pts',(373.796104089942,-14.636082409617,-2.59031117706091));
#46958=CARTESIAN_POINT('Ctrl Pts',(373.718465916748,-14.6302223105289,-2.67649563197344));
#46959=CARTESIAN_POINT('Ctrl Pts',(373.637106086513,-14.6243622114409,-2.75914246086314));
#46960=CARTESIAN_POINT('Ctrl Pts',(373.552810979214,-14.6182906933468,-2.84477099879153));
#46961=CARTESIAN_POINT('Ctrl Pts',(373.464520862328,-14.6122191752527,-2.92660145977807));
#46962=CARTESIAN_POINT('Ctrl Pts',(373.372619726218,-14.6061476571586,-3.00424909113023));
#46963=CARTESIAN_POINT('Ctrl Pts',(373.284020671374,-14.6002942935618,-3.07910678103333));
#46964=CARTESIAN_POINT('Ctrl Pts',(373.192065967718,-14.5944409299651,-3.15007676361626));
#46965=CARTESIAN_POINT('Ctrl Pts',(373.097135903173,-14.5885875663683,-3.21685303873576));
#46966=CARTESIAN_POINT('Ctrl Pts',(373.002220092059,-14.5827350816344,-3.2836192876222));
#46967=CARTESIAN_POINT('Ctrl Pts',(372.90433014617,-14.5768825969006,-3.3461928434322));
#46968=CARTESIAN_POINT('Ctrl Pts',(372.803876948802,-14.5710301121667,-3.40430991083767));
#46969=CARTESIAN_POINT('Ctrl Pts',(372.703414541224,-14.5651770908385,-3.46243230679772));
#46970=CARTESIAN_POINT('Ctrl Pts',(372.600388772605,-14.5593240695104,-3.5160971951892));
#46971=CARTESIAN_POINT('Ctrl Pts',(372.495236210784,-14.5534710481822,-3.56508614335194));
#46972=CARTESIAN_POINT('Ctrl Pts',(372.390048578553,-14.5476160747584,-3.61409143027529));
#46973=CARTESIAN_POINT('Ctrl Pts',(372.28273311695,-14.5417611013346,-3.65841750156287));
#46974=CARTESIAN_POINT('Ctrl Pts',(372.173746837527,-14.5359061279108,-3.69789385948378));
#46975=CARTESIAN_POINT('Ctrl Pts',(372.064637036156,-14.5300445186266,-3.73741495878573));
#46976=CARTESIAN_POINT('Ctrl Pts',(371.953853026003,-14.5241829093425,-3.77207523320374));
#46977=CARTESIAN_POINT('Ctrl Pts',(371.841867555091,-14.5183213000583,-3.80175388449437));
#46978=CARTESIAN_POINT('Ctrl Pts',(371.729806571553,-14.512455738248,-3.83145254831762));
#46979=CARTESIAN_POINT('Ctrl Pts',(371.616542916712,-14.5065901764376,-3.85616281236564));
#46980=CARTESIAN_POINT('Ctrl Pts',(371.502558406441,-14.5007246146273,-3.87581521270505));
#46981=CARTESIAN_POINT('Ctrl Pts',(371.38840722286,-14.494850475927,-3.89549634967374));
#46982=CARTESIAN_POINT('Ctrl Pts',(371.273533488464,-14.4889763372266,-3.91010481078251));
#46983=CARTESIAN_POINT('Ctrl Pts',(371.158423068542,-14.4831021985263,-3.91962304429951));
#46984=CARTESIAN_POINT('Ctrl Pts',(371.129313522534,-14.481616724745,-3.92203005016975));
#46985=CARTESIAN_POINT('Ctrl Pts',(371.100188832541,-14.4801312509636,-3.92411179532515));
#46986=CARTESIAN_POINT('Ctrl Pts',(371.071056826746,-14.4786457771823,-3.92586852281323));
#46987=CARTESIAN_POINT('Ctrl Pts',(370.955866403654,-14.4727720877917,-3.93281477237915));
#46988=CARTESIAN_POINT('Ctrl Pts',(370.840178153486,-14.4668983984012,-3.9346985245286));
#46989=CARTESIAN_POINT('Ctrl Pts',(370.724474343722,-14.4610247090106,-3.93146580850201));
#46990=CARTESIAN_POINT('Ctrl Pts',(370.608919918447,-14.4551586031048,-3.9282372662155));
#46991=CARTESIAN_POINT('Ctrl Pts',(370.493350382738,-14.449292497199,-3.91990540403812));
#46992=CARTESIAN_POINT('Ctrl Pts',(370.378252028211,-14.4434263912933,-3.9064680932084));
#46993=CARTESIAN_POINT('Ctrl Pts',(370.263271532933,-14.4375662922052,-3.8930445420138));
#46994=CARTESIAN_POINT('Ctrl Pts',(370.148761667057,-14.4317061931172,-3.87452598854489));
#46995=CARTESIAN_POINT('Ctrl Pts',(370.03520695041,-14.4258460940291,-3.8509623167468));
#46996=CARTESIAN_POINT('Ctrl Pts',(369.917555438646,-14.419774575935,-3.82654852142761));
#46997=CARTESIAN_POINT('Ctrl Pts',(369.800929748047,-14.4137030578409,-3.79671871456802));
#46998=CARTESIAN_POINT('Ctrl Pts',(369.685861354147,-14.4076315397468,-3.76158698819103));
#46999=CARTESIAN_POINT('Ctrl Pts',(369.574927459601,-14.4017781761501,-3.7277175728193));
#47000=CARTESIAN_POINT('Ctrl Pts',(369.465441306886,-14.3959248125533,-3.68892081630371));
#47001=CARTESIAN_POINT('Ctrl Pts',(369.357866188026,-14.3900714489565,-3.64535039198334));
#47002=CARTESIAN_POINT('Ctrl Pts',(369.250307221208,-14.3842189642226,-3.60178650961562));
#47003=CARTESIAN_POINT('Ctrl Pts',(369.144659100535,-14.3783664794887,-3.55345053966498));
#47004=CARTESIAN_POINT('Ctrl Pts',(369.041366239032,-14.3725139947548,-3.50054474463156));
#47005=CARTESIAN_POINT('Ctrl Pts',(368.938063906961,-14.3666609734267,-3.44763409884697));
#47006=CARTESIAN_POINT('Ctrl Pts',(368.837117631079,-14.3608079520985,-3.39015298341577));
#47007=CARTESIAN_POINT('Ctrl Pts',(368.738947629641,-14.3549549307703,-3.32834983529698));
#47008=CARTESIAN_POINT('Ctrl Pts',(368.640744886612,-14.3490999573465,-3.26652607463511));
#47009=CARTESIAN_POINT('Ctrl Pts',(368.545320608661,-14.3432449839227,-3.20037763495527));
#47010=CARTESIAN_POINT('Ctrl Pts',(368.453065816677,-14.3373900104989,-3.13019611820774));
#47011=CARTESIAN_POINT('Ctrl Pts',(368.360706465736,-14.3315284012147,-3.0599350597251));
#47012=CARTESIAN_POINT('Ctrl Pts',(368.271524099584,-14.3256667919306,-2.98563205106458));
#47013=CARTESIAN_POINT('Ctrl Pts',(368.185876507134,-14.3198051826464,-2.90761886022269));
#47014=CARTESIAN_POINT('Ctrl Pts',(368.100171161884,-14.3139396208361,-2.82955306451364));
#47015=CARTESIAN_POINT('Ctrl Pts',(368.018005628558,-14.3080740590258,-2.74777239570807));
#47016=CARTESIAN_POINT('Ctrl Pts',(367.939699475211,-14.3022084972155,-2.66264407040617));
#47017=CARTESIAN_POINT('Ctrl Pts',(367.861278819062,-14.2963343585151,-2.57739126661301));
#47018=CARTESIAN_POINT('Ctrl Pts',(367.786729070575,-14.2904602198148,-2.48878135187005));
#47019=CARTESIAN_POINT('Ctrl Pts',(367.716328370803,-14.2845860811144,-2.39721308763126));
#47020=CARTESIAN_POINT('Ctrl Pts',(367.69852518313,-14.2831006073331,-2.37405696846849));
#47021=CARTESIAN_POINT('Ctrl Pts',(367.680987104891,-14.2816151335519,-2.35071179676978));
#47022=CARTESIAN_POINT('Ctrl Pts',(367.663718175582,-14.2801296597706,-2.32718428237578));
#47023=CARTESIAN_POINT('Ctrl Pts',(367.595028837585,-14.2742210009985,-2.23360063515029));
#47024=CARTESIAN_POINT('Ctrl Pts',(367.530372135559,-14.2683123422264,-2.13681774927372));
#47025=CARTESIAN_POINT('Ctrl Pts',(367.470058265088,-14.2624036834543,-2.03721536015079));
#47026=CARTESIAN_POINT('Ctrl Pts',(367.409823572467,-14.2565027813539,-1.93774372541228));
#47027=CARTESIAN_POINT('Ctrl Pts',(367.353920582798,-14.2506018792536,-1.8354602919391));
#47028=CARTESIAN_POINT('Ctrl Pts',(367.302618260149,-14.2447009771533,-1.73077641082656));
#47029=CARTESIAN_POINT('Ctrl Pts',(367.251371377342,-14.2388064518613,-1.6262056563232));
#47030=CARTESIAN_POINT('Ctrl Pts',(367.204715450415,-14.2329119265693,-1.51923997634675));
#47031=CARTESIAN_POINT('Ctrl Pts',(367.162874922437,-14.2270174012773,-1.41031762591654));
#47032=CARTESIAN_POINT('Ctrl Pts',(367.119780629826,-14.2209462446738,-1.29813138286403));
#47033=CARTESIAN_POINT('Ctrl Pts',(367.081795113687,-14.2148750880703,-1.18386972379287));
#47034=CARTESIAN_POINT('Ctrl Pts',(367.049111648607,-14.2088039314667,-1.06803697901003));
#47035=CARTESIAN_POINT('Ctrl Pts',(367.017426479175,-14.2029182144791,-0.955742271722701));
#47036=CARTESIAN_POINT('Ctrl Pts',(366.990724299619,-14.1970324974915,-0.841971478729403));
#47037=CARTESIAN_POINT('Ctrl Pts',(366.969131337325,-14.1911467805039,-0.727201620814089));
#47038=CARTESIAN_POINT('Ctrl Pts',(366.946517890023,-14.1849829040924,-0.607007730852205));
#47039=CARTESIAN_POINT('Ctrl Pts',(366.929508554436,-14.178819027681,-0.485718479073686));
#47040=CARTESIAN_POINT('Ctrl Pts',(366.91818846086,-14.1726551512695,-0.363895015436532));
#47041=CARTESIAN_POINT('Ctrl Pts',(366.906868367283,-14.166491274858,-0.242071551799377));
#47042=CARTESIAN_POINT('Ctrl Pts',(366.901237566177,-14.1603273984465,-0.119714386616033));
#47043=CARTESIAN_POINT('Ctrl Pts',(366.901318718745,-14.154163522035,0.00260925024367697));
#47044=CARTESIAN_POINT('',(366.901318180018,-12.904163522076,0.00160329739904622));
#47045=CARTESIAN_POINT('Ctrl Pts',(366.901318718745,-14.1541635219903,0.0026092511316027));
#47046=CARTESIAN_POINT('Ctrl Pts',(366.901406072305,-14.1475286566482,0.134279778658182));
#47047=CARTESIAN_POINT('Ctrl Pts',(366.908109628326,-14.1408937913061,0.265695130277769));
#47048=CARTESIAN_POINT('Ctrl Pts',(366.921328559004,-14.134258925964,0.396237029214112));
#47049=CARTESIAN_POINT('Ctrl Pts',(366.934605952153,-14.1275947170512,0.527356266988295));
#47050=CARTESIAN_POINT('Ctrl Pts',(366.954456361042,-14.1209305081384,0.657594127909351));
#47051=CARTESIAN_POINT('Ctrl Pts',(366.980727954181,-14.1142662992256,0.786342094762591));
#47052=CARTESIAN_POINT('Ctrl Pts',(367.007149875336,-14.1075639572122,0.915826767086364));
#47053=CARTESIAN_POINT('Ctrl Pts',(367.040066574364,-14.1008616151989,1.04380426788823));
#47054=CARTESIAN_POINT('Ctrl Pts',(367.079275111599,-14.0941592731855,1.16967645465167));
#47055=CARTESIAN_POINT('Ctrl Pts',(367.103739184668,-14.08997736291,1.24821410465263));
#47056=CARTESIAN_POINT('Ctrl Pts',(367.13065178265,-14.0857954526344,1.32593255786291));
#47057=CARTESIAN_POINT('Ctrl Pts',(367.159954398002,-14.0816135423589,1.40269105612235));
#47058=CARTESIAN_POINT('Ctrl Pts',(367.201111297496,-14.0757398529684,1.51050197198495));
#47059=CARTESIAN_POINT('Ctrl Pts',(367.247085747281,-14.0698661635778,1.61667951064501));
#47060=CARTESIAN_POINT('Ctrl Pts',(367.297728111595,-14.0639924741873,1.72076204031903));
#47061=CARTESIAN_POINT('Ctrl Pts',(367.348305091858,-14.0581263682815,1.82471018966914));
#47062=CARTESIAN_POINT('Ctrl Pts',(367.40353782238,-14.0522602623758,1.92656834098912));
#47063=CARTESIAN_POINT('Ctrl Pts',(367.463227776419,-14.04639415647,2.02589256725735));
#47064=CARTESIAN_POINT('Ctrl Pts',(367.522856608706,-14.040534057382,2.12511508678322));
#47065=CARTESIAN_POINT('Ctrl Pts',(367.586933374509,-14.034673958294,2.2218084903306));
#47066=CARTESIAN_POINT('Ctrl Pts',(367.655212889862,-14.028813859206,2.31555190655016));
#47067=CARTESIAN_POINT('Ctrl Pts',(367.725955774359,-14.0227423411119,2.41267737136428));
#47068=CARTESIAN_POINT('Ctrl Pts',(367.801210187543,-14.0166708230177,2.50663556622445));
#47069=CARTESIAN_POINT('Ctrl Pts',(367.880653090131,-14.0105993049236,2.5969893082686));
#47070=CARTESIAN_POINT('Ctrl Pts',(367.957241545739,-14.0047459413269,2.68409656815192));
#47071=CARTESIAN_POINT('Ctrl Pts',(368.03772238303,-13.9988925777302,2.76785360237167));
#47072=CARTESIAN_POINT('Ctrl Pts',(368.121764608661,-13.9930392141334,2.84790166533418));
#47073=CARTESIAN_POINT('Ctrl Pts',(368.205794215636,-13.9871867293995,2.9279377093494));
#47074=CARTESIAN_POINT('Ctrl Pts',(368.293383848627,-13.9813342446656,3.00426560454728));
#47075=CARTESIAN_POINT('Ctrl Pts',(368.384166028363,-13.9754817599318,3.076563835699));
#47076=CARTESIAN_POINT('Ctrl Pts',(368.474956531607,-13.9696287386036,3.14886869562787));
#47077=CARTESIAN_POINT('Ctrl Pts',(368.568939840286,-13.9637757172754,3.21714289965433));
#47078=CARTESIAN_POINT('Ctrl Pts',(368.665716380528,-13.9579226959473,3.28110601057329));
#47079=CARTESIAN_POINT('Ctrl Pts',(368.762525197615,-13.9520677225235,3.34509045442497));
#47080=CARTESIAN_POINT('Ctrl Pts',(368.862128754223,-13.9462127490997,3.40476071842333));
#47081=CARTESIAN_POINT('Ctrl Pts',(368.96410018598,-13.9403577756758,3.45988076053612));
#47082=CARTESIAN_POINT('Ctrl Pts',(369.066187189257,-13.9344961663917,3.51506327413669));
#47083=CARTESIAN_POINT('Ctrl Pts',(369.170647060502,-13.9286345571076,3.5656850760382));
#47084=CARTESIAN_POINT('Ctrl Pts',(369.277030040322,-13.9227729478234,3.61155695895632));
#47085=CARTESIAN_POINT('Ctrl Pts',(369.383484754966,-13.9169073860131,3.65745977362198));
#47086=CARTESIAN_POINT('Ctrl Pts',(369.491864775044,-13.9110418242028,3.6986061453343));
#47087=CARTESIAN_POINT('Ctrl Pts',(369.601703800684,-13.9051762623925,3.73485630211955));
#47088=CARTESIAN_POINT('Ctrl Pts',(369.711703437921,-13.8993021236922,3.77115946552494));
#47089=CARTESIAN_POINT('Ctrl Pts',(369.823165942353,-13.8934279849918,3.80255201393562));
#47090=CARTESIAN_POINT('Ctrl Pts',(369.935613351939,-13.8875538462915,3.82894492247805));
#47091=CARTESIAN_POINT('Ctrl Pts',(369.964049466109,-13.8860683725101,3.8356192581816));
#47092=CARTESIAN_POINT('Ctrl Pts',(369.992548534568,-13.8845828987287,3.84197412459043));
#47093=CARTESIAN_POINT('Ctrl Pts',(370.021102778911,-13.8830974249473,3.84800860743701));
#47094=CARTESIAN_POINT('Ctrl Pts',(370.134008684185,-13.8772237355567,3.87186946470496));
#47095=CARTESIAN_POINT('Ctrl Pts',(370.24815368961,-13.8713500461661,3.89079662734276));
#47096=CARTESIAN_POINT('Ctrl Pts',(370.363068763407,-13.8654763567755,3.90466558047512));
#47097=CARTESIAN_POINT('Ctrl Pts',(370.477835471049,-13.8596102508697,3.91851662748604));
#47098=CARTESIAN_POINT('Ctrl Pts',(370.59336986344,-13.853744144964,3.92732240321013));
#47099=CARTESIAN_POINT('Ctrl Pts',(370.709191281988,-13.8478780390582,3.93100907416539));
#47100=CARTESIAN_POINT('Ctrl Pts',(370.824894100878,-13.8420179399701,3.93469197001656));
#47101=CARTESIAN_POINT('Ctrl Pts',(370.94088295083,-13.8361578408821,3.9332661746027));
#47102=CARTESIAN_POINT('Ctrl Pts',(371.056671253783,-13.830297741794,3.92670955957525));
#47103=CARTESIAN_POINT('Ctrl Pts',(371.176636934551,-13.8242262236999,3.91991639683568));
#47104=CARTESIAN_POINT('Ctrl Pts',(371.296386876134,-13.8181547056058,3.90761515397048));
#47105=CARTESIAN_POINT('Ctrl Pts',(371.415378587673,-13.8120831875117,3.8898402824386));
#47106=CARTESIAN_POINT('Ctrl Pts',(371.53009483192,-13.8062298239149,3.8727040762461));
#47107=CARTESIAN_POINT('Ctrl Pts',(371.644105952384,-13.8003764603181,3.85048088198511));
#47108=CARTESIAN_POINT('Ctrl Pts',(371.756931057686,-13.7945230967214,3.82325435655956));
#47109=CARTESIAN_POINT('Ctrl Pts',(371.869739222679,-13.7886706119874,3.79603191910517));
#47110=CARTESIAN_POINT('Ctrl Pts',(371.981361325085,-13.7828181272535,3.76380774111084));
#47111=CARTESIAN_POINT('Ctrl Pts',(372.091327979127,-13.7769656425196,3.72671632182777));
#47112=CARTESIAN_POINT('Ctrl Pts',(372.201304715634,-13.7711126211914,3.68962150175957));
#47113=CARTESIAN_POINT('Ctrl Pts',(372.309625310551,-13.7652595998632,3.64765868532898));
#47114=CARTESIAN_POINT('Ctrl Pts',(372.415837497496,-13.759406578535,3.60101160992063));
#47115=CARTESIAN_POINT('Ctrl Pts',(372.522085108256,-13.7535516051111,3.55434897681175));
#47116=CARTESIAN_POINT('Ctrl Pts',(372.626222534707,-13.7476966316873,3.50299914422174));
#47117=CARTESIAN_POINT('Ctrl Pts',(372.727820021639,-13.7418416582634,3.44719284900153));
#47118=CARTESIAN_POINT('Ctrl Pts',(372.829532656273,-13.7359800489793,3.39132330451377));
#47119=CARTESIAN_POINT('Ctrl Pts',(372.928699243372,-13.7301184396951,3.33098741526292));
#47120=CARTESIAN_POINT('Ctrl Pts',(373.024916971724,-13.7242568304109,3.26646054652843));
#47121=CARTESIAN_POINT('Ctrl Pts',(373.121199580397,-13.7183912686005,3.20189016685248));
#47122=CARTESIAN_POINT('Ctrl Pts',(373.214529039118,-13.7125257067902,3.1331234249489));
#47123=CARTESIAN_POINT('Ctrl Pts',(373.304535110808,-13.7066601449798,3.06047638454152));
#47124=CARTESIAN_POINT('Ctrl Pts',(373.394672793449,-13.7007860062795,2.98772311634321));
#47125=CARTESIAN_POINT('Ctrl Pts',(373.481477081996,-13.6949118675791,2.91107849826694));
#47126=CARTESIAN_POINT('Ctrl Pts',(373.56461406038,-13.6890377288788,2.83089590433689));
#47127=CARTESIAN_POINT('Ctrl Pts',(373.585638044988,-13.6875522550977,2.81061903532578));
#47128=CARTESIAN_POINT('Ctrl Pts',(373.606427705161,-13.6860667813166,2.7901160779877));
#47129=CARTESIAN_POINT('Ctrl Pts',(373.626978055884,-13.6845813075356,2.76939307294575));
#47130=CARTESIAN_POINT('Ctrl Pts',(373.708235886585,-13.678707618145,2.6874525524144));
#47131=CARTESIAN_POINT('Ctrl Pts',(373.78601962295,-13.6728339287545,2.60179620351885));
#47132=CARTESIAN_POINT('Ctrl Pts',(373.859970367563,-13.6669602393639,2.51275065664625));
#47133=CARTESIAN_POINT('Ctrl Pts',(373.933825634817,-13.6610941334582,2.42382007594017));
#47134=CARTESIAN_POINT('Ctrl Pts',(374.003857490222,-13.6552280275524,2.33150931416387));
#47135=CARTESIAN_POINT('Ctrl Pts',(374.069743321329,-13.6493619216467,2.23618224667331));
#47136=CARTESIAN_POINT('Ctrl Pts',(374.135561686184,-13.6435018225587,2.14095279288542));
#47137=CARTESIAN_POINT('Ctrl Pts',(374.197242237839,-13.6376417234706,2.04271351482894));
#47138=CARTESIAN_POINT('Ctrl Pts',(374.254502603075,-13.6317816243826,1.94186129187677));
#47139=CARTESIAN_POINT('Ctrl Pts',(374.313828791656,-13.6257101062885,1.83737055080101));
#47140=CARTESIAN_POINT('Ctrl Pts',(374.368409543021,-13.6196385881944,1.73007511443216));
#47141=CARTESIAN_POINT('Ctrl Pts',(374.417979717547,-13.6135670701003,1.62044951855945));
#47142=CARTESIAN_POINT('Ctrl Pts',(374.465768796086,-13.6077137065035,1.51476285795727));
#47143=CARTESIAN_POINT('Ctrl Pts',(374.508900984322,-13.6018603429068,1.40691101379008));
#47144=CARTESIAN_POINT('Ctrl Pts',(374.54718588402,-13.5960069793101,1.29734343405811));
#47145=CARTESIAN_POINT('Ctrl Pts',(374.585465035369,-13.5901544945762,1.18779230552955));
#47146=CARTESIAN_POINT('Ctrl Pts',(374.618898209084,-13.5843020098423,1.07652634358177));
#47147=CARTESIAN_POINT('Ctrl Pts',(374.647343967446,-13.5784495251084,0.964012890090213));
#47148=CARTESIAN_POINT('Ctrl Pts',(374.675792333903,-13.5725965037802,0.851489120625622));
#47149=CARTESIAN_POINT('Ctrl Pts',(374.699252274708,-13.5667434824521,0.737718032808258));
#47150=CARTESIAN_POINT('Ctrl Pts',(374.717633007921,-13.5608904611239,0.623179275410707));
#47151=CARTESIAN_POINT('Ctrl Pts',(374.736019871464,-13.5550354877001,0.508602317125604));
#47152=CARTESIAN_POINT('Ctrl Pts',(374.749324093517,-13.5491805142763,0.393257587856447));
#47153=CARTESIAN_POINT('Ctrl Pts',(374.757506589681,-13.5433255408525,0.277631298918333));
#47154=CARTESIAN_POINT('Ctrl Pts',(374.765698359653,-13.5374639315683,0.161873962433356));
#47155=CARTESIAN_POINT('Ctrl Pts',(374.768756788488,-13.5316023222842,0.045834841696479));
#47156=CARTESIAN_POINT('Ctrl Pts',(374.766694900003,-13.525740713,-0.0699982997340179));
#47157=CARTESIAN_POINT('Ctrl Pts',(374.764631621171,-13.5198751511897,-0.185909548302475));
#47158=CARTESIAN_POINT('Ctrl Pts',(374.757441175553,-13.5140095893794,-0.301614129668007));
#47159=CARTESIAN_POINT('Ctrl Pts',(374.745188444935,-13.508144027569,-0.416629589555363));
#47160=CARTESIAN_POINT('Ctrl Pts',(374.732917797818,-13.5022698888687,-0.531813230254458));
#47161=CARTESIAN_POINT('Ctrl Pts',(374.715570154221,-13.4963957501684,-0.646305331517802));
#47162=CARTESIAN_POINT('Ctrl Pts',(374.693261438031,-13.4905216114681,-0.759633733632965));
#47163=CARTESIAN_POINT('Ctrl Pts',(374.687619927899,-13.4890361376867,-0.788292636429524));
#47164=CARTESIAN_POINT('Ctrl Pts',(374.681661404466,-13.4875506639053,-0.81687719919626));
#47165=CARTESIAN_POINT('Ctrl Pts',(374.675388241292,-13.486065190124,-0.84537995830715));
#47166=CARTESIAN_POINT('Ctrl Pts',(374.650583621752,-13.4801915007334,-0.958082286609185));
#47167=CARTESIAN_POINT('Ctrl Pts',(374.620773222898,-13.4743178113429,-1.06987969207614));
#47168=CARTESIAN_POINT('Ctrl Pts',(374.586036953103,-13.4684441219523,-1.18029352095379));
#47169=CARTESIAN_POINT('Ctrl Pts',(374.551345531095,-13.4625780160465,-1.29056479520543));
#47170=CARTESIAN_POINT('Ctrl Pts',(374.511741008482,-13.4567119101408,-1.39945565478447));
#47171=CARTESIAN_POINT('Ctrl Pts',(374.467354261302,-13.450845804235,-1.50649774562634));
#47172=CARTESIAN_POINT('Ctrl Pts',(374.423012965586,-13.444985705147,-1.61343022673085));
#47173=CARTESIAN_POINT('Ctrl Pts',(374.373899343028,-13.439125606059,-1.71851732529531));
#47174=CARTESIAN_POINT('Ctrl Pts',(374.320193817271,-13.4332655069709,-1.82130660880562));
#47175=CARTESIAN_POINT('Ctrl Pts',(374.264550718667,-13.4271939888768,-1.92780429516515));
#47176=CARTESIAN_POINT('Ctrl Pts',(374.20397826595,-13.4211224707827,-2.03183480538675));
#47177=CARTESIAN_POINT('Ctrl Pts',(374.138731480556,-13.4150509526886,-2.13291809020006));
#47178=CARTESIAN_POINT('Ctrl Pts',(374.075829064305,-13.4091975890918,-2.23036937180622));
#47179=CARTESIAN_POINT('Ctrl Pts',(374.008582682789,-13.4033442254951,-2.32508119855126));
#47180=CARTESIAN_POINT('Ctrl Pts',(373.937266793996,-13.3974908618983,-2.41664992726786));
#47181=CARTESIAN_POINT('Ctrl Pts',(373.865961613043,-13.3916383771644,-2.50820490724797));
#47182=CARTESIAN_POINT('Ctrl Pts',(373.790588393545,-13.3857858924305,-2.59661740170089));
#47183=CARTESIAN_POINT('Ctrl Pts',(373.711463171816,-13.3799334076966,-2.68151520892666));
#47184=CARTESIAN_POINT('Ctrl Pts',(373.632330695366,-13.3740803863685,-2.76642080014151));
#47185=CARTESIAN_POINT('Ctrl Pts',(373.549445814526,-13.3682273650403,-2.84781076127858));
#47186=CARTESIAN_POINT('Ctrl Pts',(373.46316236817,-13.3623743437121,-2.92534878539939));
#47187=CARTESIAN_POINT('Ctrl Pts',(373.376850144618,-13.3565193702883,-3.00291266994868));
#47188=CARTESIAN_POINT('Ctrl Pts',(373.287137408791,-13.3506643968645,-3.07662178692235));
#47189=CARTESIAN_POINT('Ctrl Pts',(373.194411539847,-13.3448094234406,-3.14617971361475));
#47190=CARTESIAN_POINT('Ctrl Pts',(373.101580578041,-13.3389478141565,-3.21581647528265));
#47191=CARTESIAN_POINT('Ctrl Pts',(373.005729997663,-13.3330862048723,-3.28129240803352));
#47192=CARTESIAN_POINT('Ctrl Pts',(372.907276730594,-13.3272245955882,-3.34235403461864));
#47193=CARTESIAN_POINT('Ctrl Pts',(372.808757075764,-13.3213590337779,-3.40345683550697));
#47194=CARTESIAN_POINT('Ctrl Pts',(372.707631599127,-13.3154934719675,-3.46013920165507));
#47195=CARTESIAN_POINT('Ctrl Pts',(372.60434088383,-13.3096279101572,-3.51219411068426));
#47196=CARTESIAN_POINT('Ctrl Pts',(372.500899132173,-13.3037537714568,-3.56432513675778));
#47197=CARTESIAN_POINT('Ctrl Pts',(372.39528619845,-13.2978796327565,-3.61181503274264));
#47198=CARTESIAN_POINT('Ctrl Pts',(372.287961685617,-13.2920054940562,-3.65450524812137));
#47199=CARTESIAN_POINT('Ctrl Pts',(372.260821068406,-13.2905200202749,-3.66530090666781));
#47200=CARTESIAN_POINT('Ctrl Pts',(372.233571063781,-13.2890345464936,-3.67578987601278));
#47201=CARTESIAN_POINT('Ctrl Pts',(372.206219230214,-13.2875490727123,-3.68597010457407));
#47202=CARTESIAN_POINT('Ctrl Pts',(372.098067759174,-13.2816753833217,-3.72622359221338));
#47203=CARTESIAN_POINT('Ctrl Pts',(371.987963021316,-13.2758016939311,-3.76178011693721));
#47204=CARTESIAN_POINT('Ctrl Pts',(371.876350552237,-13.2699280045406,-3.79244734362742));
#47205=CARTESIAN_POINT('Ctrl Pts',(371.764882185342,-13.2640618986348,-3.8230749760469));
#47206=CARTESIAN_POINT('Ctrl Pts',(371.651910353161,-13.258195792729,-3.84882575554985));
#47207=CARTESIAN_POINT('Ctrl Pts',(371.537899566436,-13.2523296868233,-3.86955575910637));
#47208=CARTESIAN_POINT('Ctrl Pts',(371.424005525305,-13.2464695877352,-3.89026453540335));
#47209=CARTESIAN_POINT('Ctrl Pts',(371.309075049832,-13.2406094886472,-3.9059626885789));
#47210=CARTESIAN_POINT('Ctrl Pts',(371.193586131983,-13.2347493895592,-3.91655656206796));
#47211=CARTESIAN_POINT('Ctrl Pts',(371.073930637451,-13.2286778714651,-3.92753263834399));
#47212=CARTESIAN_POINT('Ctrl Pts',(370.95367608064,-13.2226063533709,-3.93302906002753));
#47213=CARTESIAN_POINT('Ctrl Pts',(370.833364100265,-13.2165348352768,-3.9329998843574));
#47214=CARTESIAN_POINT('Ctrl Pts',(370.717375025496,-13.2106814716801,-3.93297175699241));
#47215=CARTESIAN_POINT('Ctrl Pts',(370.601333031259,-13.2048281080833,-3.92780827699202));
#47216=CARTESIAN_POINT('Ctrl Pts',(370.485726088358,-13.1989747444866,-3.91752125475633));
#47217=CARTESIAN_POINT('Ctrl Pts',(370.370136503451,-13.1931222597527,-3.90723577708242));
#47218=CARTESIAN_POINT('Ctrl Pts',(370.254982251406,-13.1872697750188,-3.89182832340427));
#47219=CARTESIAN_POINT('Ctrl Pts',(370.140747422524,-13.1814172902849,-3.87136268743423));
#47220=CARTESIAN_POINT('Ctrl Pts',(370.026502119841,-13.1755642689567,-3.85089517504015));
#47221=CARTESIAN_POINT('Ctrl Pts',(369.913176814591,-13.1697112476285,-3.82536863128858));
#47222=CARTESIAN_POINT('Ctrl Pts',(369.801245927554,-13.1638582263003,-3.79489807457216));
#47223=CARTESIAN_POINT('Ctrl Pts',(369.689277709403,-13.1580032528765,-3.76441735533666));
#47224=CARTESIAN_POINT('Ctrl Pts',(369.578705232649,-13.1521482794527,-3.72898945278615));
#47225=CARTESIAN_POINT('Ctrl Pts',(369.469987585543,-13.1462933060288,-3.68877919109973));
#47226=CARTESIAN_POINT('Ctrl Pts',(369.361146720949,-13.1404316967447,-3.64852335624647));
#47227=CARTESIAN_POINT('Ctrl Pts',(369.254165269596,-13.1345700874605,-3.60347448728209));
#47228=CARTESIAN_POINT('Ctrl Pts',(369.149482253146,-13.1287084781764,-3.55384552291017));
#47229=CARTESIAN_POINT('Ctrl Pts',(369.044728648168,-13.122842916366,-3.50418309336308));
#47230=CARTESIAN_POINT('Ctrl Pts',(368.942276928405,-13.1169773545557,-3.44993461158795));
#47231=CARTESIAN_POINT('Ctrl Pts',(368.842539900701,-13.1111117927453,-3.3913580742591));
#47232=CARTESIAN_POINT('Ctrl Pts',(368.742657032999,-13.105237654045,-3.33269588366581));
#47233=CARTESIAN_POINT('Ctrl Pts',(368.645497124884,-13.0993635153446,-3.26969323098247));
#47234=CARTESIAN_POINT('Ctrl Pts',(368.551442562731,-13.0934893766443,-3.20265037243453));
#47235=CARTESIAN_POINT('Ctrl Pts',(368.527657699416,-13.0920039028631,-3.18569632799156));
#47236=CARTESIAN_POINT('Ctrl Pts',(368.504071249485,-13.0905184290819,-3.16848410531235));
#47237=CARTESIAN_POINT('Ctrl Pts',(368.48068903442,-13.0890329553007,-3.15101894365849));
#47238=CARTESIAN_POINT('Ctrl Pts',(368.389135817684,-13.0832165729492,-3.08263398843743));
#47239=CARTESIAN_POINT('Ctrl Pts',(368.300398414984,-13.0774001905977,-3.01013059775965));
#47240=CARTESIAN_POINT('Ctrl Pts',(368.214875700783,-13.0715838082462,-2.93377091982545));
#47241=CARTESIAN_POINT('Ctrl Pts',(368.129463801022,-13.0657749623623,-2.8575101835014));
#47242=CARTESIAN_POINT('Ctrl Pts',(368.047258621431,-13.0599661164783,-2.77740337089595));
#47243=CARTESIAN_POINT('Ctrl Pts',(367.968629026321,-13.0541572705944,-2.69375510159393));
#47244=CARTESIAN_POINT('Ctrl Pts',(367.890079276586,-13.0483543233734,-2.61019177394068));
#47245=CARTESIAN_POINT('Ctrl Pts',(367.815098179366,-13.0425513761524,-2.52309444557834));
#47246=CARTESIAN_POINT('Ctrl Pts',(367.744019929908,-13.0367484289314,-2.43280655728099));
#47247=CARTESIAN_POINT('Ctrl Pts',(367.672992694972,-13.0309496466213,-2.34258347071239));
#47248=CARTESIAN_POINT('Ctrl Pts',(367.605862997561,-13.0251508643112,-2.24917470849674));
#47249=CARTESIAN_POINT('Ctrl Pts',(367.542926173974,-13.0193520820012,-2.15295838644515));
#47250=CARTESIAN_POINT('Ctrl Pts',(367.480012683451,-13.0135554495193,-2.05677773542829));
#47251=CARTESIAN_POINT('Ctrl Pts',(367.421289208297,-13.0077588170375,-1.95779194582016));
#47252=CARTESIAN_POINT('Ctrl Pts',(367.367008575753,-13.0019621845556,-1.85640926909014));
#47253=CARTESIAN_POINT('Ctrl Pts',(367.312734307432,-12.9961662317095,-1.75503847913993));
#47254=CARTESIAN_POINT('Ctrl Pts',(367.262902045014,-12.9903702788635,-1.65127173294188));
#47255=CARTESIAN_POINT('Ctrl Pts',(367.217718930285,-12.9845743260174,-1.54554237424707));
#47256=CARTESIAN_POINT('Ctrl Pts',(367.172529659278,-12.9787775834628,-1.43979860974569));
#47257=CARTESIAN_POINT('Ctrl Pts',(367.131990959828,-12.9729808409082,-1.33209208974943));
#47258=CARTESIAN_POINT('Ctrl Pts',(367.096261725996,-12.9671840983536,-1.22287586847367));
#47259=CARTESIAN_POINT('Ctrl Pts',(367.060498227861,-12.9613817967279,-1.11355490893568));
#47260=CARTESIAN_POINT('Ctrl Pts',(367.029553535441,-12.9555794951022,-1.00272175917924));
#47261=CARTESIAN_POINT('Ctrl Pts',(367.003536554116,-12.9497771934764,-0.890844340166382));
#47262=CARTESIAN_POINT('Ctrl Pts',(366.977506020343,-12.9439718693866,-0.778908643335273));
#47263=CARTESIAN_POINT('Ctrl Pts',(366.956408385523,-12.9381665452968,-0.66592800876549));
#47264=CARTESIAN_POINT('Ctrl Pts',(366.940301024373,-12.9323612212071,-0.552378436057968));
#47265=CARTESIAN_POINT('Ctrl Pts',(366.924169836189,-12.9265473095126,-0.43866089360047));
#47266=CARTESIAN_POINT('Ctrl Pts',(366.913043701887,-12.9207333978182,-0.324373152081675));
#47267=CARTESIAN_POINT('Ctrl Pts',(366.906927960272,-12.9149194861238,-0.209994354062086));
#47268=CARTESIAN_POINT('Ctrl Pts',(366.903156506536,-12.9113341647745,-0.139459270628284));
#47269=CARTESIAN_POINT('Ctrl Pts',(366.901289443427,-12.9077488434253,-0.0688895532719928));
#47270=CARTESIAN_POINT('Ctrl Pts',(366.901318180018,-12.904163522076,0.00160329739904574));
#47271=CARTESIAN_POINT('',(366.901319491282,-11.654163521998,-0.00358956336470628));
#47272=CARTESIAN_POINT('Ctrl Pts',(366.901318180018,-12.904163522035,0.00160329820526979));
#47273=CARTESIAN_POINT('Ctrl Pts',(366.901354639733,-12.8996146273197,0.0910414613838704));
#47274=CARTESIAN_POINT('Ctrl Pts',(366.904441638581,-12.8950657326043,0.180414019458864));
#47275=CARTESIAN_POINT('Ctrl Pts',(366.910567340119,-12.890516837889,0.269575427124204));
#47276=CARTESIAN_POINT('Ctrl Pts',(366.91847705674,-12.8846431484984,0.384703704876417));
#47277=CARTESIAN_POINT('Ctrl Pts',(366.931471275856,-12.8787694591079,0.499675310147441));
#47278=CARTESIAN_POINT('Ctrl Pts',(366.949541564545,-12.8728957697173,0.614005038186002));
#47279=CARTESIAN_POINT('Ctrl Pts',(366.967588522794,-12.8670296638115,0.728187155804904));
#47280=CARTESIAN_POINT('Ctrl Pts',(366.990698453581,-12.8611635579058,0.841728639899142));
#47281=CARTESIAN_POINT('Ctrl Pts',(367.018810994597,-12.855297452,0.954146955020061));
#47282=CARTESIAN_POINT('Ctrl Pts',(367.04689474873,-12.849437352912,1.06645015521839));
#47283=CARTESIAN_POINT('Ctrl Pts',(367.079970824164,-12.843577253824,1.17763207568835));
#47284=CARTESIAN_POINT('Ctrl Pts',(367.117927504507,-12.8377171547359,1.28721862011198));
#47285=CARTESIAN_POINT('Ctrl Pts',(367.157253575284,-12.8316456366418,1.40075879705153));
#47286=CARTESIAN_POINT('Ctrl Pts',(367.201818991622,-12.8255741185477,1.51258586332659));
#47287=CARTESIAN_POINT('Ctrl Pts',(367.251442328755,-12.8195026004536,1.62218740476041));
#47288=CARTESIAN_POINT('Ctrl Pts',(367.299282659727,-12.8136492368569,1.72785087521913));
#47289=CARTESIAN_POINT('Ctrl Pts',(367.351823511469,-12.8077958732601,1.83144558961424));
#47290=CARTESIAN_POINT('Ctrl Pts',(367.408852965359,-12.8019425096634,1.93253183725558));
#47291=CARTESIAN_POINT('Ctrl Pts',(367.465873856469,-12.7960900249295,2.03360290713705));
#47292=CARTESIAN_POINT('Ctrl Pts',(367.527381806715,-12.7902375401956,2.13216589942832));
#47293=CARTESIAN_POINT('Ctrl Pts',(367.593119136315,-12.7843850554617,2.22780606819935));
#47294=CARTESIAN_POINT('Ctrl Pts',(367.658862493145,-12.7785320341335,2.32345500588973));
#47295=CARTESIAN_POINT('Ctrl Pts',(367.72883576616,-12.7726790128053,2.41618024684051));
#47296=CARTESIAN_POINT('Ctrl Pts',(367.802738592021,-12.7668259914772,2.50559697139118));
#47297=CARTESIAN_POINT('Ctrl Pts',(367.876666065902,-12.7609710180533,2.5950435181464));
#47298=CARTESIAN_POINT('Ctrl Pts',(367.954525435603,-12.7551160446295,2.68117903604957));
#47299=CARTESIAN_POINT('Ctrl Pts',(368.03597728144,-12.7492610712057,2.76365320623022));
#47300=CARTESIAN_POINT('Ctrl Pts',(368.117521442481,-12.7433994619215,2.84622085028926));
#47301=CARTESIAN_POINT('Ctrl Pts',(368.202665915875,-12.7375378526374,2.9251185700214));
#47302=CARTESIAN_POINT('Ctrl Pts',(368.291035718006,-12.7316762433532,3.00003416325228));
#47303=CARTESIAN_POINT('Ctrl Pts',(368.379465108544,-12.7258106815429,3.0750002726178));
#47304=CARTESIAN_POINT('Ctrl Pts',(368.471123832607,-12.7199451197325,3.145978656371));
#47305=CARTESIAN_POINT('Ctrl Pts',(368.565606661921,-12.7140795579222,3.21269957052569));
#47306=CARTESIAN_POINT('Ctrl Pts',(368.660227648304,-12.7082054192218,3.27951804702129));
#47307=CARTESIAN_POINT('Ctrl Pts',(368.757680635097,-12.7023312805215,3.34206640715481));
#47308=CARTESIAN_POINT('Ctrl Pts',(368.857534432652,-12.6964571418212,3.40012004319746));
#47309=CARTESIAN_POINT('Ctrl Pts',(368.882785827929,-12.6949716680399,3.4148008600198));
#47310=CARTESIAN_POINT('Ctrl Pts',(368.908190650798,-12.6934861942586,3.42919447683107));
#47311=CARTESIAN_POINT('Ctrl Pts',(368.933741728072,-12.6920007204774,3.44329774961458));
#47312=CARTESIAN_POINT('Ctrl Pts',(369.034772855911,-12.6861270310868,3.49906328702451));
#47313=CARTESIAN_POINT('Ctrl Pts',(369.138428687797,-12.6802533416962,3.55047134344653));
#47314=CARTESIAN_POINT('Ctrl Pts',(369.244296930802,-12.6743796523057,3.59726597102029));
#47315=CARTESIAN_POINT('Ctrl Pts',(369.350028487959,-12.6685135463999,3.64400018233366));
#47316=CARTESIAN_POINT('Ctrl Pts',(369.457966401305,-12.6626474404942,3.68613264456638));
#47317=CARTESIAN_POINT('Ctrl Pts',(369.567672469534,-12.6567813345884,3.72345249358408));
#47318=CARTESIAN_POINT('Ctrl Pts',(369.677266200147,-12.6509212355004,3.76073412755182));
#47319=CARTESIAN_POINT('Ctrl Pts',(369.788624095465,-12.6450611364124,3.79321281834872));
#47320=CARTESIAN_POINT('Ctrl Pts',(369.901287206112,-12.6392010373243,3.8207254300133));
#47321=CARTESIAN_POINT('Ctrl Pts',(370.018014944766,-12.6331295192302,3.84923063394046));
#47322=CARTESIAN_POINT('Ctrl Pts',(370.136143442146,-12.6270580011361,3.87240448109303));
#47323=CARTESIAN_POINT('Ctrl Pts',(370.255143760507,-12.620986483042,3.89012163952816));
#47324=CARTESIAN_POINT('Ctrl Pts',(370.369868302326,-12.6151331194453,3.9072022063015));
#47325=CARTESIAN_POINT('Ctrl Pts',(370.485402649207,-12.6092797558485,3.91921139624782));
#47326=CARTESIAN_POINT('Ctrl Pts',(370.601262425706,-12.6034263922518,3.92608891490046));
#47327=CARTESIAN_POINT('Ctrl Pts',(370.717104806249,-12.5975739075178,3.93296540091682));
#47328=CARTESIAN_POINT('Ctrl Pts',(370.833272106946,-12.5917214227839,3.93471172321431));
#47329=CARTESIAN_POINT('Ctrl Pts',(370.949276122877,-12.58586893805,3.93131957442261));
#47330=CARTESIAN_POINT('Ctrl Pts',(371.065290774818,-12.5800159167219,3.92792711461641));
#47331=CARTESIAN_POINT('Ctrl Pts',(371.181141699241,-12.5741628953937,3.91939525923755));
#47332=CARTESIAN_POINT('Ctrl Pts',(371.296342699342,-12.5683098740655,3.90576779155772));
#47333=CARTESIAN_POINT('Ctrl Pts',(371.411582121201,-12.5624549006417,3.89213577885425));
#47334=CARTESIAN_POINT('Ctrl Pts',(371.526170777654,-12.5565999272179,3.87340482300706));
#47335=CARTESIAN_POINT('Ctrl Pts',(371.639630290366,-12.5507449537941,3.84967022984889));
#47336=CARTESIAN_POINT('Ctrl Pts',(371.753218394861,-12.5448833445099,3.82590873657798));
#47337=CARTESIAN_POINT('Ctrl Pts',(371.865674396715,-12.5390217352258,3.79713237170308));
#47338=CARTESIAN_POINT('Ctrl Pts',(371.976532667806,-12.5331601259416,3.7634869891297));
#47339=CARTESIAN_POINT('Ctrl Pts',(372.087465691444,-12.5272945641313,3.72981891922774));
#47340=CARTESIAN_POINT('Ctrl Pts',(372.196798450375,-12.5214290023209,3.69127543104097));
#47341=CARTESIAN_POINT('Ctrl Pts',(372.30408459851,-12.5155634405106,3.64805081028907));
#47342=CARTESIAN_POINT('Ctrl Pts',(372.411527625307,-12.5096893018102,3.60476298454009));
#47343=CARTESIAN_POINT('Ctrl Pts',(372.516917694174,-12.5038151631099,3.55678053593144));
#47344=CARTESIAN_POINT('Ctrl Pts',(372.619832313464,-12.4979410244096,3.50434403451963));
#47345=CARTESIAN_POINT('Ctrl Pts',(372.645857740589,-12.4964555506283,3.49108369934473));
#47346=CARTESIAN_POINT('Ctrl Pts',(372.671725005849,-12.494970076847,3.47753874390132));
#47347=CARTESIAN_POINT('Ctrl Pts',(372.697427578647,-12.4934846030657,3.46371349147598));
#47348=CARTESIAN_POINT('Ctrl Pts',(372.799057732646,-12.4876109136751,3.40904727015657));
#47349=CARTESIAN_POINT('Ctrl Pts',(372.898449138204,-12.4817372242845,3.34981325754317));
#47350=CARTESIAN_POINT('Ctrl Pts',(372.995163212408,-12.475863534894,3.28621915484824));
#47351=CARTESIAN_POINT('Ctrl Pts',(373.091752419657,-12.4699974289882,3.22270715811428));
#47352=CARTESIAN_POINT('Ctrl Pts',(373.185670827716,-12.4641313230825,3.15484649101718));
#47353=CARTESIAN_POINT('Ctrl Pts',(373.276503692705,-12.4582652171767,3.08289106610005));
#47354=CARTESIAN_POINT('Ctrl Pts',(373.367243545997,-12.4524051180887,3.01100932262141));
#47355=CARTESIAN_POINT('Ctrl Pts',(373.454903818918,-12.4465450190006,2.93504141652364));
#47356=CARTESIAN_POINT('Ctrl Pts',(373.539098626219,-12.4406849199126,2.8552845690121));
#47357=CARTESIAN_POINT('Ctrl Pts',(373.626330990088,-12.4346134018185,2.77265027639684));
#47358=CARTESIAN_POINT('Ctrl Pts',(373.709842737651,-12.4285418837244,2.68594873601789));
#47359=CARTESIAN_POINT('Ctrl Pts',(373.78924180931,-12.4224703656303,2.59555647477553));
#47360=CARTESIAN_POINT('Ctrl Pts',(373.86578800887,-12.4166170020335,2.50841207971925));
#47361=CARTESIAN_POINT('Ctrl Pts',(373.938511693713,-12.4107636384368,2.41783795750291));
#47362=CARTESIAN_POINT('Ctrl Pts',(374.00709961339,-12.40491027484,2.32420844640899));
#47363=CARTESIAN_POINT('Ctrl Pts',(374.075677234821,-12.3990577901061,2.23059299347107));
#47364=CARTESIAN_POINT('Ctrl Pts',(374.140120081728,-12.3932053053722,2.13392339703328));
#47365=CARTESIAN_POINT('Ctrl Pts',(374.20015651283,-12.3873528206383,2.03460539601675));
#47366=CARTESIAN_POINT('Ctrl Pts',(374.260198448467,-12.3814997993102,1.93527828887301));
#47367=CARTESIAN_POINT('Ctrl Pts',(374.31583295143,-12.375646777982,1.83330264802732));
#47368=CARTESIAN_POINT('Ctrl Pts',(374.366833241234,-12.3697937566538,1.72911076379621));
#47369=CARTESIAN_POINT('Ctrl Pts',(374.417850540619,-12.36393878323,1.62488412955958));
#47370=CARTESIAN_POINT('Ctrl Pts',(374.464230371951,-12.3580838098062,1.51844015302638));
#47371=CARTESIAN_POINT('Ctrl Pts',(374.505793488026,-12.3522288363823,1.41023248546386));
#47372=CARTESIAN_POINT('Ctrl Pts',(374.547403710553,-12.3463672270982,1.30190217840889));
#47373=CARTESIAN_POINT('Ctrl Pts',(374.58418617351,-12.340505617814,1.19180457649481));
#47374=CARTESIAN_POINT('Ctrl Pts',(374.616011017644,-12.3346440085299,1.08041001947475));
#47375=CARTESIAN_POINT('Ctrl Pts',(374.647857321504,-12.3287784467195,0.968940348286817));
#47376=CARTESIAN_POINT('Ctrl Pts',(374.674739254403,-12.3229128849092,0.856172381466526));
#47377=CARTESIAN_POINT('Ctrl Pts',(374.696578107696,-12.3170473230988,0.742586511273045));
#47378=CARTESIAN_POINT('Ctrl Pts',(374.718448894749,-12.3111731843985,0.628834550678589));
#47379=CARTESIAN_POINT('Ctrl Pts',(374.735261825353,-12.3052990456982,0.51426270704055));
#47380=CARTESIAN_POINT('Ctrl Pts',(374.746990015676,-12.2994249069978,0.399356418719132));
#47381=CARTESIAN_POINT('Ctrl Pts',(374.749955883545,-12.2979394332166,0.370298494262374));
#47382=CARTESIAN_POINT('Ctrl Pts',(374.752596841717,-12.2964539594353,0.341219179107541));
#47383=CARTESIAN_POINT('Ctrl Pts',(374.754912982785,-12.2949684856541,0.312126304660852));
#47384=CARTESIAN_POINT('Ctrl Pts',(374.764071201122,-12.2890947962635,0.197090610234631));
#47385=CARTESIAN_POINT('Ctrl Pts',(374.768177421767,-12.2832211068729,0.0814599105867828));
#47386=CARTESIAN_POINT('Ctrl Pts',(374.76716841771,-12.2773474174824,-0.03428465281692));
#47387=CARTESIAN_POINT('Ctrl Pts',(374.766160716373,-12.2714813115766,-0.149879779115507));
#47388=CARTESIAN_POINT('Ctrl Pts',(374.760050927563,-12.2656152056709,-0.265588067461628));
#47389=CARTESIAN_POINT('Ctrl Pts',(374.748827579379,-12.2597490997651,-0.380923356911745));
#47390=CARTESIAN_POINT('Ctrl Pts',(374.73761572376,-12.2538890006771,-0.496140544494782));
#47391=CARTESIAN_POINT('Ctrl Pts',(374.721300763818,-12.248028901589,-0.610985084145689));
#47392=CARTESIAN_POINT('Ctrl Pts',(374.699923264801,-12.242168802501,-0.724971587018397));
#47393=CARTESIAN_POINT('Ctrl Pts',(374.67777451439,-12.2360972844069,-0.843070462869916));
#47394=CARTESIAN_POINT('Ctrl Pts',(374.650191042279,-12.2300257663128,-0.96024776933949));
#47395=CARTESIAN_POINT('Ctrl Pts',(374.617276707743,-12.2239542482187,-1.07596993685671));
#47396=CARTESIAN_POINT('Ctrl Pts',(374.58554501155,-12.2181008846219,-1.1875341144122));
#47397=CARTESIAN_POINT('Ctrl Pts',(374.548859067127,-12.2122475210252,-1.29774549056792));
#47398=CARTESIAN_POINT('Ctrl Pts',(374.507363617822,-12.2063941574284,-1.4061379061707));
#47399=CARTESIAN_POINT('Ctrl Pts',(374.465874398919,-12.2005416726945,-1.51451404701703));
#47400=CARTESIAN_POINT('Ctrl Pts',(374.41957725867,-12.1946891879606,-1.62107138462301));
#47401=CARTESIAN_POINT('Ctrl Pts',(374.368665883355,-12.1888367032267,-1.72536170176207));
#47402=CARTESIAN_POINT('Ctrl Pts',(374.31774984015,-12.1829836818985,-1.82966158092295));
#47403=CARTESIAN_POINT('Ctrl Pts',(374.26221890212,-12.1771306605703,-1.93169365513127));
#47404=CARTESIAN_POINT('Ctrl Pts',(374.202313386353,-12.1712776392422,-2.03103301027451));
#47405=CARTESIAN_POINT('Ctrl Pts',(374.142387890939,-12.1654226658183,-2.13040549701116));
#47406=CARTESIAN_POINT('Ctrl Pts',(374.078085129855,-12.1595676923945,-2.22708312530035));
#47407=CARTESIAN_POINT('Ctrl Pts',(374.009689138205,-12.1537127189707,-2.32066934364151));
#47408=CARTESIAN_POINT('Ctrl Pts',(373.941215628484,-12.1478511096865,-2.41436162994045));
#47409=CARTESIAN_POINT('Ctrl Pts',(373.868639872644,-12.1419895004024,-2.50495517933917));
#47410=CARTESIAN_POINT('Ctrl Pts',(373.792286702936,-12.1361278911182,-2.592085894436));
#47411=CARTESIAN_POINT('Ctrl Pts',(373.715882047724,-12.1302623293079,-2.67927536241393));
#47412=CARTESIAN_POINT('Ctrl Pts',(373.635695191791,-12.1243967674975,-2.76299704892786));
#47413=CARTESIAN_POINT('Ctrl Pts',(373.552087143815,-12.1185312056872,-2.84292438927202));
#47414=CARTESIAN_POINT('Ctrl Pts',(373.468356840368,-12.1126570669868,-2.92296860299122));
#47415=CARTESIAN_POINT('Ctrl Pts',(373.381195670678,-12.1067829282865,-2.99920712664242));
#47416=CARTESIAN_POINT('Ctrl Pts',(373.29099697843,-12.1009087895862,-3.07135420877801));
#47417=CARTESIAN_POINT('Ctrl Pts',(373.268187201665,-12.0994233158049,-3.08959902804002));
#47418=CARTESIAN_POINT('Ctrl Pts',(373.245183313492,-12.0979378420236,-3.10758241923529));
#47419=CARTESIAN_POINT('Ctrl Pts',(373.221991944898,-12.0964523682424,-3.12530021469079));
#47420=CARTESIAN_POINT('Ctrl Pts',(373.130291305428,-12.0905786788518,-3.19535788147928));
#47421=CARTESIAN_POINT('Ctrl Pts',(373.035351942402,-12.0847049894612,-3.26149287295327));
#47422=CARTESIAN_POINT('Ctrl Pts',(372.937543886807,-12.0788313000706,-3.32339122759574));
#47423=CARTESIAN_POINT('Ctrl Pts',(372.8398621106,-12.0729651941649,-3.38520966564726));
#47424=CARTESIAN_POINT('Ctrl Pts',(372.739319353292,-12.0670990882591,-3.44280212578014));
#47425=CARTESIAN_POINT('Ctrl Pts',(372.636317920711,-12.0612329823534,-3.49589541559476));
#47426=CARTESIAN_POINT('Ctrl Pts',(372.533421960285,-12.0553728832653,-3.54893433855698));
#47427=CARTESIAN_POINT('Ctrl Pts',(372.428072697452,-12.0495127841773,-3.59748306692355));
#47428=CARTESIAN_POINT('Ctrl Pts',(372.320699999074,-12.0436526850892,-3.64131255407982));
#47429=CARTESIAN_POINT('Ctrl Pts',(372.209453538694,-12.0375811669951,-3.68672330914158));
#47430=CARTESIAN_POINT('Ctrl Pts',(372.096035265976,-12.031509648901,-3.72706763338565));
#47431=CARTESIAN_POINT('Ctrl Pts',(371.980949846715,-12.0254381308069,-3.76214354743448));
#47432=CARTESIAN_POINT('Ctrl Pts',(371.869999538542,-12.0195847672102,-3.79595915585957));
#47433=CARTESIAN_POINT('Ctrl Pts',(371.757500254915,-12.0137314036134,-3.82487830411396));
#47434=CARTESIAN_POINT('Ctrl Pts',(371.643922179774,-12.0078780400167,-3.84876991185897));
#47435=CARTESIAN_POINT('Ctrl Pts',(371.530361158,-12.0020255552828,-3.87265793235948));
#47436=CARTESIAN_POINT('Ctrl Pts',(371.415722070971,-11.9961730705489,-3.89151982828963));
#47437=CARTESIAN_POINT('Ctrl Pts',(371.300486558315,-11.990320585815,-3.9052753729275));
#47438=CARTESIAN_POINT('Ctrl Pts',(371.185240480109,-11.9844675644868,-3.91903217876412));
#47439=CARTESIAN_POINT('Ctrl Pts',(371.069398277824,-11.9786145431586,-3.92768165363101));
#47440=CARTESIAN_POINT('Ctrl Pts',(370.953447288301,-11.9727615218304,-3.93119538788117));
#47441=CARTESIAN_POINT('Ctrl Pts',(370.837457626884,-11.9669065484066,-3.93471029402956));
#47442=CARTESIAN_POINT('Ctrl Pts',(370.721359518816,-11.9610515749828,-3.933086041091));
#47443=CARTESIAN_POINT('Ctrl Pts',(370.605640167566,-11.955196601559,-3.92634633165261));
#47444=CARTESIAN_POINT('Ctrl Pts',(370.489789663294,-11.9493349922748,-3.91959898361925));
#47445=CARTESIAN_POINT('Ctrl Pts',(370.374319185319,-11.9434733829907,-3.90772463123533));
#47446=CARTESIAN_POINT('Ctrl Pts',(370.259710782196,-11.9376117737065,-3.89079885292523));
#47447=CARTESIAN_POINT('Ctrl Pts',(370.145025097785,-11.9317462118962,-3.87386166143853));
#47448=CARTESIAN_POINT('Ctrl Pts',(370.031203050367,-11.9258806500858,-3.851866339692));
#47449=CARTESIAN_POINT('Ctrl Pts',(369.918714761065,-11.9200150882755,-3.82493921227891));
#47450=CARTESIAN_POINT('Ctrl Pts',(369.806061986295,-11.9141409495752,-3.79797271080122));
#47451=CARTESIAN_POINT('Ctrl Pts',(369.694747257532,-11.9082668108748,-3.76606012471631));
#47452=CARTESIAN_POINT('Ctrl Pts',(369.585223929312,-11.9023926721745,-3.72937707522931));
#47453=CARTESIAN_POINT('Ctrl Pts',(369.557527267587,-11.9009071983932,-3.72010053086942));
#47454=CARTESIAN_POINT('Ctrl Pts',(369.529945056278,-11.899421724612,-3.71051915052861));
#47455=CARTESIAN_POINT('Ctrl Pts',(369.502484392234,-11.8979362508307,-3.70063624694272));
#47456=CARTESIAN_POINT('Ctrl Pts',(369.393902596252,-11.8920625614401,-3.6615584074867));
#47457=CARTESIAN_POINT('Ctrl Pts',(369.286861312276,-11.8861888720496,-3.61763252361588));
#47458=CARTESIAN_POINT('Ctrl Pts',(369.181824961949,-11.880315182659,-3.5689993337471));
#47459=CARTESIAN_POINT('Ctrl Pts',(369.076924223419,-11.8744490767533,-3.52042893389528));
#47460=CARTESIAN_POINT('Ctrl Pts',(368.97402364223,-11.8685829708475,-3.46716348634993));
#47461=CARTESIAN_POINT('Ctrl Pts',(368.873570877915,-11.8627168649417,-3.40939295165821));
#47462=CARTESIAN_POINT('Ctrl Pts',(368.773220975951,-11.8568567658537,-3.35168157325814));
#47463=CARTESIAN_POINT('Ctrl Pts',(368.675314261174,-11.8509966667657,-3.28947448839703));
#47464=CARTESIAN_POINT('Ctrl Pts',(368.580276238164,-11.8451365676777,-3.22300874922444));
#47465=CARTESIAN_POINT('Ctrl Pts',(368.4818094601,-11.8390650495835,-3.15414507781506));
#47466=CARTESIAN_POINT('Ctrl Pts',(368.386422683485,-11.8329935314894,-3.08070985512133));
#47467=CARTESIAN_POINT('Ctrl Pts',(368.294559217302,-11.8269220133953,-3.00301766083049));
#47468=CARTESIAN_POINT('Ctrl Pts',(368.205996478874,-11.8210686497986,-2.92811700917058));
#47469=CARTESIAN_POINT('Ctrl Pts',(368.120708560026,-11.8152152862018,-2.8492603236528));
#47470=CARTESIAN_POINT('Ctrl Pts',(368.03906049978,-11.8093619226051,-2.76677164363374));
#47471=CARTESIAN_POINT('Ctrl Pts',(367.957424698715,-11.8035094378712,-2.6842953490124));
#47472=CARTESIAN_POINT('Ctrl Pts',(367.87942796014,-11.7976569531373,-2.5981884377652));
#47473=CARTESIAN_POINT('Ctrl Pts',(367.805398800622,-11.7918044684034,-2.50881214378072));
#47474=CARTESIAN_POINT('Ctrl Pts',(367.731362853623,-11.7859514470752,-2.41942765519019));
#47475=CARTESIAN_POINT('Ctrl Pts',(367.661295472383,-11.780098425747,-2.3267735061631));
#47476=CARTESIAN_POINT('Ctrl Pts',(367.595484719689,-11.7742454044189,-2.2312438085323));
#47477=CARTESIAN_POINT('Ctrl Pts',(367.529652017837,-11.7683904309951,-2.13568224990259));
#47478=CARTESIAN_POINT('Ctrl Pts',(367.468079001734,-11.7625354575713,-2.0372435756811));
#47479=CARTESIAN_POINT('Ctrl Pts',(367.411009871542,-11.7566804841475,-1.93635003616424));
#47480=CARTESIAN_POINT('Ctrl Pts',(367.353876060822,-11.7508188748633,-1.83534214677945));
#47481=CARTESIAN_POINT('Ctrl Pts',(367.301256527959,-11.7449572655792,-1.73187419865204));
#47482=CARTESIAN_POINT('Ctrl Pts',(367.253349086919,-11.739095656295,-1.62639223274904));
#47483=CARTESIAN_POINT('Ctrl Pts',(367.205409341539,-11.7332300944847,-1.52083913958189));
#47484=CARTESIAN_POINT('Ctrl Pts',(367.162188168537,-11.7273645326743,-1.41326970683518));
#47485=CARTESIAN_POINT('Ctrl Pts',(367.123834273497,-11.721498970864,-1.30414746274167));
#47486=CARTESIAN_POINT('Ctrl Pts',(367.085424295656,-11.7156248321637,-1.19486565516319));
#47487=CARTESIAN_POINT('Ctrl Pts',(367.05189591899,-11.7097506934633,-1.08402689863707));
#47488=CARTESIAN_POINT('Ctrl Pts',(367.023347335428,-11.703876554763,-0.972107356462185));
#47489=CARTESIAN_POINT('Ctrl Pts',(367.016127864704,-11.7023910809817,-0.943804731345743));
#47490=CARTESIAN_POINT('Ctrl Pts',(367.009226594706,-11.7009056072004,-0.915433025326923));
#47491=CARTESIAN_POINT('Ctrl Pts',(367.002644588985,-11.6994201334191,-0.886999997809972));
#47492=CARTESIAN_POINT('Ctrl Pts',(366.96759754733,-11.6915104682349,-0.735603365530406));
#47493=CARTESIAN_POINT('Ctrl Pts',(366.941511575413,-11.6836008030508,-0.582060497872048));
#47494=CARTESIAN_POINT('Ctrl Pts',(366.924595479983,-11.6756911378667,-0.427270364268486));
#47495=CARTESIAN_POINT('Ctrl Pts',(366.909248719815,-11.6685152659228,-0.286840377529521));
#47496=CARTESIAN_POINT('Ctrl Pts',(366.901448903756,-11.6613393939789,-0.145383673730004));
#47497=CARTESIAN_POINT('Ctrl Pts',(366.901319491283,-11.654163522035,-0.00358956409668104));
#47498=CARTESIAN_POINT('',(366.90131788919,-10.4041635220097,0.00053189028649518));
#47499=CARTESIAN_POINT('Ctrl Pts',(366.901319491282,-11.654163521998,-0.00358956336471676));
#47500=CARTESIAN_POINT('Ctrl Pts',(366.901215182272,-11.6483796262582,0.110699313728239));
#47501=CARTESIAN_POINT('Ctrl Pts',(366.906096752376,-11.6425957305185,0.225131833427297));
#47502=CARTESIAN_POINT('Ctrl Pts',(366.915974982574,-11.6368118347788,0.339231702561064));
#47503=CARTESIAN_POINT('Ctrl Pts',(366.925845835326,-11.6310322586764,0.453246357493513));
#47504=CARTESIAN_POINT('Ctrl Pts',(366.940705892319,-11.625252682574,0.566928433969708));
#47505=CARTESIAN_POINT('Ctrl Pts',(366.960513867979,-11.6194731064716,0.679802680118736));
#47506=CARTESIAN_POINT('Ctrl Pts',(366.980314074705,-11.6136957971903,0.792632655595791));
#47507=CARTESIAN_POINT('Ctrl Pts',(367.005058271152,-11.607918487909,0.904655012256961));
#47508=CARTESIAN_POINT('Ctrl Pts',(367.034653522482,-11.6021411786277,1.01540138550626));
#47509=CARTESIAN_POINT('Ctrl Pts',(367.064244769121,-11.5963646511048,1.12613277307442));
#47510=CARTESIAN_POINT('Ctrl Pts',(367.098685656149,-11.5905881235819,1.23558810989203));
#47511=CARTESIAN_POINT('Ctrl Pts',(367.137832716529,-11.5848115960591,1.34331181569878));
#47512=CARTESIAN_POINT('Ctrl Pts',(367.176984536858,-11.5790343661599,1.45104861978714));
#47513=CARTESIAN_POINT('Ctrl Pts',(367.220843521669,-11.5732571362606,1.55705297529893));
#47514=CARTESIAN_POINT('Ctrl Pts',(367.2692174786,-11.5674799063614,1.66088781043613));
#47515=CARTESIAN_POINT('Ctrl Pts',(367.317639838785,-11.5616968957335,1.76482654329352));
#47516=CARTESIAN_POINT('Ctrl Pts',(367.370586012797,-11.5559138851055,1.86659103486682));
#47517=CARTESIAN_POINT('Ctrl Pts',(367.427817094876,-11.5501308744776,1.96576742860724));
#47518=CARTESIAN_POINT('Ctrl Pts',(367.485077457007,-11.5443449051976,2.06499456208419));
#47519=CARTESIAN_POINT('Ctrl Pts',(367.546626862797,-11.5385589359176,2.16163060370046));
#47520=CARTESIAN_POINT('Ctrl Pts',(367.612183253346,-11.5327729666377,2.25529102784255));
#47521=CARTESIAN_POINT('Ctrl Pts',(367.677845415416,-11.5269776620242,2.34910256777101));
#47522=CARTESIAN_POINT('Ctrl Pts',(367.747527215841,-11.5211823574107,2.43992856443434));
#47523=CARTESIAN_POINT('Ctrl Pts',(367.820906340132,-11.5153870527972,2.52741766488383));
#47524=CARTESIAN_POINT('Ctrl Pts',(367.88203355878,-11.5105593738673,2.60029895672426));
#47525=CARTESIAN_POINT('Ctrl Pts',(367.945725724977,-11.5057316949374,2.67086518134212));
#47526=CARTESIAN_POINT('Ctrl Pts',(368.011778274973,-11.5009040160074,2.73893397678839));
#47527=CARTESIAN_POINT('Ctrl Pts',(368.092142393581,-11.4950303266169,2.82175119960785));
#47528=CARTESIAN_POINT('Ctrl Pts',(368.176288405315,-11.4891566372263,2.90116636477388));
#47529=CARTESIAN_POINT('Ctrl Pts',(368.263896635884,-11.4832829478357,2.97681436529831));
#47530=CARTESIAN_POINT('Ctrl Pts',(368.351391755996,-11.47741684193,3.05236469714728));
#47531=CARTESIAN_POINT('Ctrl Pts',(368.442339895635,-11.4715507360242,3.1241572692397));
#47532=CARTESIAN_POINT('Ctrl Pts',(368.536383445241,-11.4656846301184,3.19186253723573));
#47533=CARTESIAN_POINT('Ctrl Pts',(368.630330695451,-11.4598245310304,3.25949847589982));
#47534=CARTESIAN_POINT('Ctrl Pts',(368.727366717613,-11.4539644319424,3.32305519551668));
#47535=CARTESIAN_POINT('Ctrl Pts',(368.827100131096,-11.4481043328543,3.38224274941558));
#47536=CARTESIAN_POINT('Ctrl Pts',(368.930431698608,-11.4420328147602,3.44356565523069));
#47537=CARTESIAN_POINT('Ctrl Pts',(369.036658621759,-11.4359612966661,3.50019788883464));
#47538=CARTESIAN_POINT('Ctrl Pts',(369.145311546712,-11.429889778572,3.55186524189249));
#47539=CARTESIAN_POINT('Ctrl Pts',(369.250060485239,-11.4240364149752,3.60167614566354));
#47540=CARTESIAN_POINT('Ctrl Pts',(369.357063684405,-11.4181830513785,3.6468726203118));
#47541=CARTESIAN_POINT('Ctrl Pts',(369.465875437462,-11.4123296877817,3.68725566712477));
#47542=CARTESIAN_POINT('Ctrl Pts',(369.574670852801,-11.4064772030478,3.72763265055916));
#47543=CARTESIAN_POINT('Ctrl Pts',(369.685273894864,-11.4006247183139,3.76319749948658));
#47544=CARTESIAN_POINT('Ctrl Pts',(369.797220025612,-11.39477223358,3.79379982286389));
#47545=CARTESIAN_POINT('Ctrl Pts',(369.909176420316,-11.3889192122518,3.82440495206331));
#47546=CARTESIAN_POINT('Ctrl Pts',(370.022475749958,-11.3830661909237,3.85004654227254));
#47547=CARTESIAN_POINT('Ctrl Pts',(370.136640198579,-11.3772131695955,3.87062461241202));
#47548=CARTESIAN_POINT('Ctrl Pts',(370.25084272325,-11.3713581961716,3.89120954573541));
#47549=CARTESIAN_POINT('Ctrl Pts',(370.365910534263,-11.3655032227478,3.90672752767336));
#47550=CARTESIAN_POINT('Ctrl Pts',(370.481358261021,-11.3596482493239,3.91713013905234));
#47551=CARTESIAN_POINT('Ctrl Pts',(370.596936832949,-11.3537866400398,3.92754454045511));
#47552=CARTESIAN_POINT('Ctrl Pts',(370.712895768338,-11.3479250307556,3.93283196250993));
#47553=CARTESIAN_POINT('Ctrl Pts',(370.828747143433,-11.3420634214715,3.93299605481526));
#47554=CARTESIAN_POINT('Ctrl Pts',(370.944676637962,-11.3361978596611,3.93316025776924));
#47555=CARTESIAN_POINT('Ctrl Pts',(371.060498016033,-11.3303322978508,3.92819426955597));
#47556=CARTESIAN_POINT('Ctrl Pts',(371.175727665805,-11.3244667360404,3.91815369018025));
#47557=CARTESIAN_POINT('Ctrl Pts',(371.291125809587,-11.3185925973401,3.90809842901487));
#47558=CARTESIAN_POINT('Ctrl Pts',(371.405930090223,-11.3127184586397,3.89295382146471));
#47559=CARTESIAN_POINT('Ctrl Pts',(371.519666207819,-11.3068443199394,3.87282669801451));
#47560=CARTESIAN_POINT('Ctrl Pts',(371.548428215201,-11.3053588461582,3.86773687707201));
#47561=CARTESIAN_POINT('Ctrl Pts',(371.577121987322,-11.303873372377,3.86232867299253));
#47562=CARTESIAN_POINT('Ctrl Pts',(371.605740016327,-11.3023878985958,3.8566043154922));
#47563=CARTESIAN_POINT('Ctrl Pts',(371.718898131588,-11.2965142092052,3.83396972015762));
#47564=CARTESIAN_POINT('Ctrl Pts',(371.831247671338,-11.2906405198146,3.80631288254161));
#47565=CARTESIAN_POINT('Ctrl Pts',(371.942308534838,-11.2847668304241,3.77370449948818));
#47566=CARTESIAN_POINT('Ctrl Pts',(372.053226008329,-11.2789007245183,3.74113821692072));
#47567=CARTESIAN_POINT('Ctrl Pts',(372.162857721535,-11.2730346186126,3.70363321764507));
#47568=CARTESIAN_POINT('Ctrl Pts',(372.27073289222,-11.2671685127068,3.66131135465771));
#47569=CARTESIAN_POINT('Ctrl Pts',(372.378497600105,-11.2613084136188,3.61903282871878));
#47570=CARTESIAN_POINT('Ctrl Pts',(372.484508960866,-11.2554483145307,3.57194740002706));
#47571=CARTESIAN_POINT('Ctrl Pts',(372.588311158879,-11.2495882154427,3.52022676595114));
#47572=CARTESIAN_POINT('Ctrl Pts',(372.695858303384,-11.2435166973486,3.46664016939151));
#47573=CARTESIAN_POINT('Ctrl Pts',(372.801033439052,-11.2374451792545,3.40807772474959));
#47574=CARTESIAN_POINT('Ctrl Pts',(372.903351705287,-11.2313736611604,3.34478518279101));
#47575=CARTESIAN_POINT('Ctrl Pts',(373.001993594445,-11.2255202975636,3.28376679244709));
#47576=CARTESIAN_POINT('Ctrl Pts',(373.097979998734,-11.2196669339668,3.21835260328277));
#47577=CARTESIAN_POINT('Ctrl Pts',(373.190902076107,-11.2138135703701,3.14880926708155));
#47578=CARTESIAN_POINT('Ctrl Pts',(373.283810201543,-11.2079610856362,3.07927637257826));
#47579=CARTESIAN_POINT('Ctrl Pts',(373.37365458423,-11.2021086009023,3.00561581126896));
#47580=CARTESIAN_POINT('Ctrl Pts',(373.460057018905,-11.1962561161684,2.92813640969929));
#47581=CARTESIAN_POINT('Ctrl Pts',(373.546467375524,-11.1904030948402,2.8506499043089));
#47582=CARTESIAN_POINT('Ctrl Pts',(373.629434849181,-11.184550073512,2.7693441384577));
#47583=CARTESIAN_POINT('Ctrl Pts',(373.708616396416,-11.1786970521839,2.68456642395035));
#47584=CARTESIAN_POINT('Ctrl Pts',(373.787824352227,-11.17284207876,2.59976043443776));
#47585=CARTESIAN_POINT('Ctrl Pts',(373.863243588983,-11.1669871053362,2.51148049548327));
#47586=CARTESIAN_POINT('Ctrl Pts',(373.934570295656,-11.1611321319124,2.4201082193142));
#47587=CARTESIAN_POINT('Ctrl Pts',(374.00597784199,-11.1552705226282,2.3286323844066));
#47588=CARTESIAN_POINT('Ctrl Pts',(374.073283345994,-11.1494089133441,2.234057542831));
#47589=CARTESIAN_POINT('Ctrl Pts',(374.136225366349,-11.1435473040599,2.13679567922817));
#47590=CARTESIAN_POINT('Ctrl Pts',(374.19920982897,-11.1376817422495,2.03946823123608));
#47591=CARTESIAN_POINT('Ctrl Pts',(374.257824740736,-11.1318161804392,1.9394505089267));
#47592=CARTESIAN_POINT('Ctrl Pts',(374.311854652188,-11.1259506186288,1.83717903641679));
#47593=CARTESIAN_POINT('Ctrl Pts',(374.365963568622,-11.1200764799285,1.73475801793067));
#47594=CARTESIAN_POINT('Ctrl Pts',(374.415473928492,-11.1142023412282,1.63007704422646));
#47595=CARTESIAN_POINT('Ctrl Pts',(374.460218379809,-11.1083282025278,1.5235925870489));
#47596=CARTESIAN_POINT('Ctrl Pts',(374.471533521088,-11.1068427287466,1.49666440620109));
#47597=CARTESIAN_POINT('Ctrl Pts',(374.482544131535,-11.1053572549653,1.46962096545237));
#47598=CARTESIAN_POINT('Ctrl Pts',(374.493248014717,-11.1038717811841,1.4424697824612));
#47599=CARTESIAN_POINT('Ctrl Pts',(374.53557207717,-11.0979980917935,1.33511170082433));
#47600=CARTESIAN_POINT('Ctrl Pts',(374.573237573548,-11.092124402403,1.22571046622616));
#47601=CARTESIAN_POINT('Ctrl Pts',(374.606043643788,-11.0862507130124,1.11470783651795));
#47602=CARTESIAN_POINT('Ctrl Pts',(374.638807358309,-11.0803846071066,1.00384852163303));
#47603=CARTESIAN_POINT('Ctrl Pts',(374.666724007546,-11.0745185012009,0.891392315905275));
#47604=CARTESIAN_POINT('Ctrl Pts',(374.689640769999,-11.0686523952951,0.7778008790112));
#47605=CARTESIAN_POINT('Ctrl Pts',(374.712534065979,-11.0627922962071,0.664325758300855));
#47606=CARTESIAN_POINT('Ctrl Pts',(374.730437577704,-11.056932197119,0.549718121236184));
#47607=CARTESIAN_POINT('Ctrl Pts',(374.743248481834,-11.0510720980309,0.434454072040985));
#47608=CARTESIAN_POINT('Ctrl Pts',(374.756521574159,-11.0450005799368,0.315031558910803));
#47609=CARTESIAN_POINT('Ctrl Pts',(374.764327533741,-11.0389290618427,0.1949048088503));
#47610=CARTESIAN_POINT('Ctrl Pts',(374.76661001934,-11.0328575437486,0.0746144778491838));
#47611=CARTESIAN_POINT('Ctrl Pts',(374.768810493406,-11.0270041801519,-0.0413537254252988));
#47612=CARTESIAN_POINT('Ctrl Pts',(374.765877579626,-11.0211508165552,-0.157473508275035));
#47613=CARTESIAN_POINT('Ctrl Pts',(374.757813710422,-11.0152974529584,-0.273256763051596));
#47614=CARTESIAN_POINT('Ctrl Pts',(374.74975105198,-11.0094449682245,-0.389022633362168));
#47615=CARTESIAN_POINT('Ctrl Pts',(374.736558998648,-11.0035924834906,-0.504451664033412));
#47616=CARTESIAN_POINT('Ctrl Pts',(374.718292031124,-10.9977399987567,-0.619058628406891));
#47617=CARTESIAN_POINT('Ctrl Pts',(374.700023388765,-10.9918869774286,-0.733676100700433));
#47618=CARTESIAN_POINT('Ctrl Pts',(374.676678972271,-10.9860339561004,-0.847470948845424));
#47619=CARTESIAN_POINT('Ctrl Pts',(374.648364663355,-10.9801809347722,-0.959966629697134));
#47620=CARTESIAN_POINT('Ctrl Pts',(374.62004091107,-10.9743259613484,-1.07249983003061));
#47621=CARTESIAN_POINT('Ctrl Pts',(374.586744071174,-10.9684709879246,-1.18373260104513));
#47622=CARTESIAN_POINT('Ctrl Pts',(374.548630116569,-10.9626160145008,-1.29320277233124));
#47623=CARTESIAN_POINT('Ctrl Pts',(374.510472964692,-10.9567544052166,-1.40279701399576));
#47624=CARTESIAN_POINT('Ctrl Pts',(374.467487937032,-10.9508927959325,-1.51062427829115));
#47625=CARTESIAN_POINT('Ctrl Pts',(374.419879497689,-10.9450311866483,-1.61624153323157));
#47626=CARTESIAN_POINT('Ctrl Pts',(374.372238955626,-10.939165624838,-1.72193000666273));
#47627=CARTESIAN_POINT('Ctrl Pts',(374.319968979865,-10.9333000630276,-1.82540513551587));
#47628=CARTESIAN_POINT('Ctrl Pts',(374.263319587847,-10.9274345012173,-1.92624923204487));
#47629=CARTESIAN_POINT('Ctrl Pts',(374.206587360523,-10.921560362517,-2.02724078737673));
#47630=CARTESIAN_POINT('Ctrl Pts',(374.145463153846,-10.9156862238166,-2.12559328276021));
#47631=CARTESIAN_POINT('Ctrl Pts',(374.080239821498,-10.9098120851163,-2.22091863333134));
#47632=CARTESIAN_POINT('Ctrl Pts',(374.063745905526,-10.908326611335,-2.24502485829247));
#47633=CARTESIAN_POINT('Ctrl Pts',(374.046990046694,-10.9068411375538,-2.26893766709365));
#47634=CARTESIAN_POINT('Ctrl Pts',(374.029977371444,-10.9053556637725,-2.29265113866268));
#47635=CARTESIAN_POINT('Ctrl Pts',(373.962707809783,-10.8994819743819,-2.38641621760609));
#47636=CARTESIAN_POINT('Ctrl Pts',(373.89119591768,-10.8936082849913,-2.4773742795736));
#47637=CARTESIAN_POINT('Ctrl Pts',(373.815704019572,-10.8877345956008,-2.56511705914373));
#47638=CARTESIAN_POINT('Ctrl Pts',(373.740309588596,-10.881868489695,-2.65274655454223));
#47639=CARTESIAN_POINT('Ctrl Pts',(373.660945637523,-10.8760023837893,-2.73716871266042));
#47640=CARTESIAN_POINT('Ctrl Pts',(373.577917256613,-10.8701362778835,-2.81800484629181));
#47641=CARTESIAN_POINT('Ctrl Pts',(373.494973895707,-10.8642761787954,-2.89875820475259));
#47642=CARTESIAN_POINT('Ctrl Pts',(373.408373862918,-10.8584160797074,-2.97593255623467));
#47643=CARTESIAN_POINT('Ctrl Pts',(373.318461490852,-10.8525559806193,-3.04918339685073));
#47644=CARTESIAN_POINT('Ctrl Pts',(373.225305285526,-10.8464844625252,-3.12507696068391));
#47645=CARTESIAN_POINT('Ctrl Pts',(373.128593519723,-10.8404129444311,-3.19675822351067));
#47646=CARTESIAN_POINT('Ctrl Pts',(373.028749967792,-10.834341426337,-3.26388674658822));
#47647=CARTESIAN_POINT('Ctrl Pts',(372.932493874474,-10.8284880627402,-3.3286032881839));
#47648=CARTESIAN_POINT('Ctrl Pts',(372.833327549274,-10.8226346991435,-3.38908837641804));
#47649=CARTESIAN_POINT('Ctrl Pts',(372.731662471519,-10.8167813355467,-3.4450794474769));
#47650=CARTESIAN_POINT('Ctrl Pts',(372.630012658433,-10.8109288508128,-3.50106211166493));
#47651=CARTESIAN_POINT('Ctrl Pts',(372.525865200583,-10.8050763660789,-3.5525519011026));
#47652=CARTESIAN_POINT('Ctrl Pts',(372.419657372243,-10.799223881345,-3.5993315503625));
#47653=CARTESIAN_POINT('Ctrl Pts',(372.313439806072,-10.7933708600168,-3.64611548868808));
#47654=CARTESIAN_POINT('Ctrl Pts',(372.205161871994,-10.7875178386886,-3.68818826180301));
#47655=CARTESIAN_POINT('Ctrl Pts',(372.095281412437,-10.7816648173604,-3.72538050436962));
#47656=CARTESIAN_POINT('Ctrl Pts',(371.985364305624,-10.7758098439366,-3.76258515126731));
#47657=CARTESIAN_POINT('Ctrl Pts',(371.873844001681,-10.7699548705128,-3.79490589851871));
#47658=CARTESIAN_POINT('Ctrl Pts',(371.76119342042,-10.764099897089,-3.82222326440183));
#47659=CARTESIAN_POINT('Ctrl Pts',(371.648415164195,-10.7582382878048,-3.84957159101047));
#47660=CARTESIAN_POINT('Ctrl Pts',(371.53450447554,-10.7523766785207,-3.871905120476));
#47661=CARTESIAN_POINT('Ctrl Pts',(371.419944479641,-10.7465150692365,-3.88915549373279));
#47662=CARTESIAN_POINT('Ctrl Pts',(371.305307235095,-10.7406495074261,-3.906417499043));
#47663=CARTESIAN_POINT('Ctrl Pts',(371.190020221328,-10.7347839456158,-3.91858947974213));
#47664=CARTESIAN_POINT('Ctrl Pts',(371.074569961465,-10.7289183838054,-3.92565509494733));
#47665=CARTESIAN_POINT('Ctrl Pts',(370.958950885005,-10.7230442451051,-3.93273104181488));
#47666=CARTESIAN_POINT('Ctrl Pts',(370.84316849755,-10.7171701064047,-3.93468571446806));
#47667=CARTESIAN_POINT('Ctrl Pts',(370.727707668622,-10.7112959677044,-3.93155481565997));
#47668=CARTESIAN_POINT('Ctrl Pts',(370.698509509899,-10.7098104939232,-3.93076306246374));
#47669=CARTESIAN_POINT('Ctrl Pts',(370.669331878578,-10.708325020142,-3.92964634388684));
#47670=CARTESIAN_POINT('Ctrl Pts',(370.640182529275,-10.7068395463608,-3.92820575784862));
#47671=CARTESIAN_POINT('Ctrl Pts',(370.524923528467,-10.7009658569702,-3.92250955840308));
#47672=CARTESIAN_POINT('Ctrl Pts',(370.40972347837,-10.6950921675796,-3.91172678479583));
#47673=CARTESIAN_POINT('Ctrl Pts',(370.295067656193,-10.689218478189,-3.89585654574217));
#47674=CARTESIAN_POINT('Ctrl Pts',(370.180559865454,-10.6833523722833,-3.88000679665806));
#47675=CARTESIAN_POINT('Ctrl Pts',(370.066595310801,-10.6774862663775,-3.85908270064177));
#47676=CARTESIAN_POINT('Ctrl Pts',(369.953657598398,-10.6716201604718,-3.83313533749715));
#47677=CARTESIAN_POINT('Ctrl Pts',(369.840835532773,-10.6657600613837,-3.80721454412178));
#47678=CARTESIAN_POINT('Ctrl Pts',(369.729038618192,-10.6598999622957,-3.77628080694585));
#47679=CARTESIAN_POINT('Ctrl Pts',(369.618743009953,-10.6540398632076,-3.74043671252538));
#47680=CARTESIAN_POINT('Ctrl Pts',(369.504468187795,-10.6479683451135,-3.7032994449518));
#47681=CARTESIAN_POINT('Ctrl Pts',(369.391805492076,-10.6418968270194,-3.66089088357027));
#47682=CARTESIAN_POINT('Ctrl Pts',(369.281270728248,-10.6358253089253,-3.61338257420974));
#47683=CARTESIAN_POINT('Ctrl Pts',(369.174707566821,-10.6299719453285,-3.5675812763722));
#47684=CARTESIAN_POINT('Ctrl Pts',(369.070122464476,-10.6241185817318,-3.51704057673404));
#47685=CARTESIAN_POINT('Ctrl Pts',(368.967959122503,-10.618265218135,-3.46196390626234));
#47686=CARTESIAN_POINT('Ctrl Pts',(368.865811120013,-10.6124127334011,-3.40689550536733));
#47687=CARTESIAN_POINT('Ctrl Pts',(368.76608451845,-10.6065602486672,-3.34729268384378));
#47688=CARTESIAN_POINT('Ctrl Pts',(368.669198938201,-10.6007077639333,-3.2834051050409));
#47689=CARTESIAN_POINT('Ctrl Pts',(368.572304474845,-10.5948547426051,-3.21951166860491));
#47690=CARTESIAN_POINT('Ctrl Pts',(368.478251895547,-10.589001721277,-3.15133292138021));
#47691=CARTESIAN_POINT('Ctrl Pts',(368.387431720063,-10.5831486999488,-3.07916177739079));
#47692=CARTESIAN_POINT('Ctrl Pts',(368.296581254297,-10.577293726525,-3.00696656293146));
#47693=CARTESIAN_POINT('Ctrl Pts',(368.208965659316,-10.5714387531012,-2.930776560893));
#47694=CARTESIAN_POINT('Ctrl Pts',(368.124941710878,-10.5655837796774,-2.85092439732906));
#47695=CARTESIAN_POINT('Ctrl Pts',(368.040822532086,-10.5597221703933,-2.77098173159402));
#47696=CARTESIAN_POINT('Ctrl Pts',(367.960303424295,-10.5538605611091,-2.68736890477402));
#47697=CARTESIAN_POINT('Ctrl Pts',(367.883703736922,-10.547998951825,-2.60045483265561));
#47698=CARTESIAN_POINT('Ctrl Pts',(367.807052397818,-10.5421333900146,-2.51348215373961));
#47699=CARTESIAN_POINT('Ctrl Pts',(367.734326000261,-10.5362678282043,-2.42320411789578));
#47700=CARTESIAN_POINT('Ctrl Pts',(367.665802024439,-10.5304022663939,-2.33002069577421));
#47701=CARTESIAN_POINT('Ctrl Pts',(367.597177849757,-10.5245281276936,-2.23670101663513));
#47702=CARTESIAN_POINT('Ctrl Pts',(367.53276858954,-10.5186539889932,-2.14046781452422));
#47703=CARTESIAN_POINT('Ctrl Pts',(367.472807094867,-10.5127798502929,-2.0417478839095));
#47704=CARTESIAN_POINT('Ctrl Pts',(367.457643811743,-10.5112943765116,-2.01678322507226));
#47705=CARTESIAN_POINT('Ctrl Pts',(367.442764727678,-10.5098089027304,-1.99165964874772));
#47706=CARTESIAN_POINT('Ctrl Pts',(367.428173123932,-10.5083234289491,-1.96638426639313));
#47707=CARTESIAN_POINT('Ctrl Pts',(367.368141660461,-10.5022120263512,-1.86239856207889));
#47708=CARTESIAN_POINT('Ctrl Pts',(367.312793417312,-10.4961006237533,-1.75551901299763));
#47709=CARTESIAN_POINT('Ctrl Pts',(367.262405685373,-10.4899892211554,-1.64618725094086));
#47710=CARTESIAN_POINT('Ctrl Pts',(367.212102004518,-10.4838880129041,-1.53703786369272));
#47711=CARTESIAN_POINT('Ctrl Pts',(367.166742509801,-10.4777868046528,-1.42544473910998));
#47712=CARTESIAN_POINT('Ctrl Pts',(367.126559598673,-10.4716855964015,-1.3118756518083));
#47713=CARTESIAN_POINT('Ctrl Pts',(367.086459358382,-10.4655969405508,-1.19854021735285));
#47714=CARTESIAN_POINT('Ctrl Pts',(367.051514595037,-10.4595082847,-1.0832372664709));
#47715=CARTESIAN_POINT('Ctrl Pts',(367.02191005392,-10.4534196288493,-0.966455261149849));
#47716=CARTESIAN_POINT('Ctrl Pts',(366.992341577382,-10.4473383902664,-0.849815520959467));
#47717=CARTESIAN_POINT('Ctrl Pts',(366.968100460896,-10.4412571516836,-0.731700666398687));
#47718=CARTESIAN_POINT('Ctrl Pts',(366.949322268095,-10.4351759131007,-0.612615951090308));
#47719=CARTESIAN_POINT('Ctrl Pts',(366.93057115913,-10.4291034455039,-0.493702991971166));
#47720=CARTESIAN_POINT('Ctrl Pts',(366.917267326928,-10.423030977907,-0.373823320364159));
#47721=CARTESIAN_POINT('Ctrl Pts',(366.909495549282,-10.4169585103101,-0.253493357862614));
#47722=CARTESIAN_POINT('Ctrl Pts',(366.904037043204,-10.4126935142184,-0.168979638918359));
#47723=CARTESIAN_POINT('Ctrl Pts',(366.901306424284,-10.4084285181267,-0.084244080169046));
#47724=CARTESIAN_POINT('Ctrl Pts',(366.90131788919,-10.404163522035,0.000531889783890909));
#47725=CARTESIAN_POINT('',(366.901319257773,-9.15416352206362,0.0033238806608616));
#47726=CARTESIAN_POINT('Ctrl Pts',(366.90131788919,-10.4041635220097,0.000531890286507496));
#47727=CARTESIAN_POINT('Ctrl Pts',(366.901334546036,-10.397967106677,0.123698971514546));
#47728=CARTESIAN_POINT('Ctrl Pts',(366.90714118116,-10.3917706913442,0.24673041215044));
#47729=CARTESIAN_POINT('Ctrl Pts',(366.918674138795,-10.3855742760115,0.369084409932434));
#47730=CARTESIAN_POINT('Ctrl Pts',(366.930425787995,-10.3792603623053,0.493758522643907));
#47731=CARTESIAN_POINT('Ctrl Pts',(366.948123041569,-10.3729464485991,0.617728875741365));
#47732=CARTESIAN_POINT('Ctrl Pts',(366.971644572484,-10.366632534893,0.740435092533959));
#47733=CARTESIAN_POINT('Ctrl Pts',(366.994835326488,-10.3604074120428,0.861415725079769));
#47734=CARTESIAN_POINT('Ctrl Pts',(367.023687438356,-10.3541822891927,0.981167248159586));
#47735=CARTESIAN_POINT('Ctrl Pts',(367.058034653411,-10.3479571663425,1.09916977524578));
#47736=CARTESIAN_POINT('Ctrl Pts',(367.093116725923,-10.3415988572083,1.21969696224078));
#47737=CARTESIAN_POINT('Ctrl Pts',(367.133931549207,-10.3352405480742,1.33839911611543));
#47738=CARTESIAN_POINT('Ctrl Pts',(367.180251034586,-10.32888223894,1.45474557394974));
#47739=CARTESIAN_POINT('Ctrl Pts',(367.226570519964,-10.3225239298058,1.57109203178405));
#47740=CARTESIAN_POINT('Ctrl Pts',(367.278394451635,-10.3161656206716,1.68508249127342));
#47741=CARTESIAN_POINT('Ctrl Pts',(367.335446269933,-10.3098073115375,1.79621453163071));
#47742=CARTESIAN_POINT('Ctrl Pts',(367.388149693561,-10.3039336221469,1.89887627276736));
#47743=CARTESIAN_POINT('Ctrl Pts',(367.445463080222,-10.2980599327563,1.99938744358157));
#47744=CARTESIAN_POINT('Ctrl Pts',(367.507187193913,-10.2921862433658,2.09730555138536));
#47745=CARTESIAN_POINT('Ctrl Pts',(367.568831615974,-10.28632013746,2.19509723771302));
#47746=CARTESIAN_POINT('Ctrl Pts',(367.634875221945,-10.2804540315542,2.29030217257284));
#47747=CARTESIAN_POINT('Ctrl Pts',(367.705072114982,-10.2745879256485,2.38250081000885));
#47748=CARTESIAN_POINT('Ctrl Pts',(367.775197127294,-10.2687278265604,2.47460503721481));
#47749=CARTESIAN_POINT('Ctrl Pts',(367.849466718492,-10.2628677274724,2.56370876344987));
#47750=CARTESIAN_POINT('Ctrl Pts',(367.927591136577,-10.2570076283843,2.64942046393696));
#47751=CARTESIAN_POINT('Ctrl Pts',(368.008534105435,-10.2509361102902,2.73822444703758));
#47752=CARTESIAN_POINT('Ctrl Pts',(368.093615058581,-10.2448645921961,2.82338664814203));
#47753=CARTESIAN_POINT('Ctrl Pts',(368.182465071594,-10.238793074102,2.90450784549792));
#47754=CARTESIAN_POINT('Ctrl Pts',(368.268122632632,-10.2329397105052,2.98271429340253));
#47755=CARTESIAN_POINT('Ctrl Pts',(368.357282732902,-10.2270863469085,3.05716483048702));
#47756=CARTESIAN_POINT('Ctrl Pts',(368.449577121972,-10.2212329833117,3.1275390716518));
#47757=CARTESIAN_POINT('Ctrl Pts',(368.54185765335,-10.2153804985778,3.19790274636107));
#47758=CARTESIAN_POINT('Ctrl Pts',(368.637271209345,-10.2095280138439,3.2641910916806));
#47759=CARTESIAN_POINT('Ctrl Pts',(368.735417345211,-10.20367552911,3.32612472067188));
#47760=CARTESIAN_POINT('Ctrl Pts',(368.833572479761,-10.1978225077818,3.38806402814545));
#47761=CARTESIAN_POINT('Ctrl Pts',(368.934460342818,-10.1919694864536,3.44564760508858));
#47762=CARTESIAN_POINT('Ctrl Pts',(369.037653081194,-10.1861164651254,3.49864040692185));
#47763=CARTESIAN_POINT('Ctrl Pts',(369.140880236341,-10.1802614917016,3.55165088287785));
#47764=CARTESIAN_POINT('Ctrl Pts',(369.246413428055,-10.1744065182777,3.60006735054566));
#47765=CARTESIAN_POINT('Ctrl Pts',(369.353802532841,-10.1685515448539,3.64370187942303));
#47766=CARTESIAN_POINT('Ctrl Pts',(369.461313349384,-10.1626899355697,3.68738586243426));
#47767=CARTESIAN_POINT('Ctrl Pts',(369.570683894368,-10.1568283262856,3.72627693362464));
#47768=CARTESIAN_POINT('Ctrl Pts',(369.681446409961,-10.1509667170014,3.76023622067938));
#47769=CARTESIAN_POINT('Ctrl Pts',(369.792283613532,-10.145101155191,3.79421840673072));
#47770=CARTESIAN_POINT('Ctrl Pts',(369.904514257726,-10.1392355933807,3.82326208351196));
#47771=CARTESIAN_POINT('Ctrl Pts',(370.017659551262,-10.1333700315704,3.84727932672379));
#47772=CARTESIAN_POINT('Ctrl Pts',(370.130970290967,-10.12749589287,3.87133168903586));
#47773=CARTESIAN_POINT('Ctrl Pts',(370.24519794324,-10.1216217541697,3.89034288170131));
#47774=CARTESIAN_POINT('Ctrl Pts',(370.359857675873,-10.1157476154693,3.90427669871234));
#47775=CARTESIAN_POINT('Ctrl Pts',(370.38885325042,-10.1142621416881,3.90780033356294));
#47776=CARTESIAN_POINT('Ctrl Pts',(370.417876454481,-10.112776667907,3.91099952969392));
#47777=CARTESIAN_POINT('Ctrl Pts',(370.446919456317,-10.1112911941258,3.91387422920996));
#47778=CARTESIAN_POINT('Ctrl Pts',(370.561757950213,-10.1054175047352,3.92524103504811));
#47779=CARTESIAN_POINT('Ctrl Pts',(370.677288407797,-10.0995438153447,3.93156820814741));
#47780=CARTESIAN_POINT('Ctrl Pts',(370.793030991257,-10.0936701259541,3.93278328859206));
#47781=CARTESIAN_POINT('Ctrl Pts',(370.908624140169,-10.0878040200484,3.9339968002537));
#47782=CARTESIAN_POINT('Ctrl Pts',(371.024428460962,-10.0819379141426,3.93011134058086));
#47783=CARTESIAN_POINT('Ctrl Pts',(371.139958102859,-10.0760718082369,3.92110609876892));
#47784=CARTESIAN_POINT('Ctrl Pts',(371.255369443875,-10.0702117091488,3.91211007820986));
#47785=CARTESIAN_POINT('Ctrl Pts',(371.370506256012,-10.0643516100608,3.89800473537644));
#47786=CARTESIAN_POINT('Ctrl Pts',(371.484882460614,-10.0584915109728,3.87882130184055));
#47787=CARTESIAN_POINT('Ctrl Pts',(371.603385097744,-10.0524199928787,3.85894577378706));
#47788=CARTESIAN_POINT('Ctrl Pts',(371.721070757523,-10.0463484747846,3.83361882040846));
#47789=CARTESIAN_POINT('Ctrl Pts',(371.837403973344,-10.0402769566905,3.8029340298805));
#47790=CARTESIAN_POINT('Ctrl Pts',(371.949557243748,-10.0344235930937,3.77335176839896));
#47791=CARTESIAN_POINT('Ctrl Pts',(372.060453152648,-10.028570229497,3.7387901807376));
#47792=CARTESIAN_POINT('Ctrl Pts',(372.169622845867,-10.0227168659003,3.69938502681498));
#47793=CARTESIAN_POINT('Ctrl Pts',(372.278776147624,-10.0168643811664,3.65998578944362));
#47794=CARTESIAN_POINT('Ctrl Pts',(372.386203360558,-10.0110118964325,3.61574457207803));
#47795=CARTESIAN_POINT('Ctrl Pts',(372.491452628727,-10.0051594116986,3.56684641326465));
#47796=CARTESIAN_POINT('Ctrl Pts',(372.59671154684,-9.99930639037042,3.51794377114663));
#47797=CARTESIAN_POINT('Ctrl Pts',(372.699791748524,-9.99345336904225,3.46438351287105));
#47798=CARTESIAN_POINT('Ctrl Pts',(372.800263780691,-9.98760034771409,3.40639774692813));
#47799=CARTESIAN_POINT('Ctrl Pts',(372.90076932222,-9.98174537429027,3.34839264161242));
#47800=CARTESIAN_POINT('Ctrl Pts',(372.99866460689,-9.97589040086647,3.28595930008741));
#47801=CARTESIAN_POINT('Ctrl Pts',(373.093547698998,-9.97003542744265,3.21937408574433));
#47802=CARTESIAN_POINT('Ctrl Pts',(373.188538328904,-9.96417381815851,3.1527134056134));
#47803=CARTESIAN_POINT('Ctrl Pts',(373.280509613871,-9.95831220887437,3.08189169799638));
#47804=CARTESIAN_POINT('Ctrl Pts',(373.369091282435,-9.95245059959023,3.00722673946687));
#47805=CARTESIAN_POINT('Ctrl Pts',(373.457732682269,-9.94658503777989,2.93251143380745));
#47806=CARTESIAN_POINT('Ctrl Pts',(373.542979611424,-9.94071947596956,2.85394799621234));
#47807=CARTESIAN_POINT('Ctrl Pts',(373.624498629115,-9.93485391415923,2.77189109415366));
#47808=CARTESIAN_POINT('Ctrl Pts',(373.706136847603,-9.92897977545891,2.68971420477846));
#47809=CARTESIAN_POINT('Ctrl Pts',(373.784035998702,-9.92310563675859,2.60403396056645));
#47810=CARTESIAN_POINT('Ctrl Pts',(373.857902826068,-9.91723149805827,2.51523814220289));
#47811=CARTESIAN_POINT('Ctrl Pts',(373.876582540825,-9.91574602427691,2.49278312934004));
#47812=CARTESIAN_POINT('Ctrl Pts',(373.895004605402,-9.91426055049554,2.4701290178639));
#47813=CARTESIAN_POINT('Ctrl Pts',(373.91316472549,-9.91277507671417,2.44728235746109));
#47814=CARTESIAN_POINT('Ctrl Pts',(373.984971381404,-9.90690138732361,2.35694472343385));
#47815=CARTESIAN_POINT('Ctrl Pts',(374.052918314477,-9.90102769793304,2.26329359404956));
#47816=CARTESIAN_POINT('Ctrl Pts',(374.116684511433,-9.89515400854247,2.16669289957718));
#47817=CARTESIAN_POINT('Ctrl Pts',(374.180368380238,-9.88928790263671,2.07021692567662));
#47818=CARTESIAN_POINT('Ctrl Pts',(374.239882021702,-9.88342179673096,1.9707993015303));
#47819=CARTESIAN_POINT('Ctrl Pts',(374.294944564018,-9.8775556908252,1.86883700962394));
#47820=CARTESIAN_POINT('Ctrl Pts',(374.349950722991,-9.87169559173716,1.76697912580552));
#47821=CARTESIAN_POINT('Ctrl Pts',(374.400514653648,-9.86583549264912,1.66258211855848));
#47822=CARTESIAN_POINT('Ctrl Pts',(374.446399092259,-9.85997539356108,1.55607137452421));
#47823=CARTESIAN_POINT('Ctrl Pts',(374.493938936736,-9.85390387546697,1.4457179658352));
#47824=CARTESIAN_POINT('Ctrl Pts',(374.536455014542,-9.84783235737286,1.33309580010779));
#47825=CARTESIAN_POINT('Ctrl Pts',(374.573735687013,-9.84176083927875,1.21870556917476));
#47826=CARTESIAN_POINT('Ctrl Pts',(374.60967683513,-9.835907475682,1.10842547065745));
#47827=CARTESIAN_POINT('Ctrl Pts',(374.640752188752,-9.83005411208525,0.996502602799251));
#47828=CARTESIAN_POINT('Ctrl Pts',(374.666821657699,-9.82420074848849,0.883404544185893));
#47829=CARTESIAN_POINT('Ctrl Pts',(374.692887212402,-9.81834826375459,0.770323466865458));
#47830=CARTESIAN_POINT('Ctrl Pts',(374.713948284152,-9.81249577902068,0.656067952120754));
#47831=CARTESIAN_POINT('Ctrl Pts',(374.729915406888,-9.80664329428677,0.541118009202179));
#47832=CARTESIAN_POINT('Ctrl Pts',(374.745883993595,-9.80079027295859,0.426157526917199));
#47833=CARTESIAN_POINT('Ctrl Pts',(374.756757645998,-9.79493725163042,0.310502899127331));
#47834=CARTESIAN_POINT('Ctrl Pts',(374.762498596077,-9.78908423030223,0.194640826852297));
#47835=CARTESIAN_POINT('Ctrl Pts',(374.768241460874,-9.78322925687841,0.078740112338653));
#47836=CARTESIAN_POINT('Ctrl Pts',(374.768848198966,-9.77737428345458,-0.0373677718189149));
#47837=CARTESIAN_POINT('Ctrl Pts',(374.764333147511,-9.77151931003076,-0.153195256672398));
#47838=CARTESIAN_POINT('Ctrl Pts',(374.759812978826,-9.7656577007466,-0.269154017102489));
#47839=CARTESIAN_POINT('Ctrl Pts',(374.750159450483,-9.75979609146244,-0.384831330863294));
#47840=CARTESIAN_POINT('Ctrl Pts',(374.735438864949,-9.75393448217828,-0.499743786234178));
#47841=CARTESIAN_POINT('Ctrl Pts',(374.720708353216,-9.74806892036794,-0.614733727917623));
#47842=CARTESIAN_POINT('Ctrl Pts',(374.70090405118,-9.74220335855759,-0.72895737817487));
#47843=CARTESIAN_POINT('Ctrl Pts',(374.676143227281,-9.73633779674725,-0.841942275486847));
#47844=CARTESIAN_POINT('Ctrl Pts',(374.651346196984,-9.73046365804691,-0.955092384430067));
#47845=CARTESIAN_POINT('Ctrl Pts',(374.621578286132,-9.72458951934657,-1.06699972768164));
#47846=CARTESIAN_POINT('Ctrl Pts',(374.587006372825,-9.71871538064623,-1.17720766003844));
#47847=CARTESIAN_POINT('Ctrl Pts',(374.578263700341,-9.71722990686499,-1.20507744697278));
#47848=CARTESIAN_POINT('Ctrl Pts',(374.569214049117,-9.71574443308375,-1.23283866169124));
#47849=CARTESIAN_POINT('Ctrl Pts',(374.559860594919,-9.71425895930251,-1.26048414500367));
#47850=CARTESIAN_POINT('Ctrl Pts',(374.522876243273,-9.70838526991194,-1.36979673205813));
#47851=CARTESIAN_POINT('Ctrl Pts',(374.481015143014,-9.70251158052137,-1.47766224106919));
#47852=CARTESIAN_POINT('Ctrl Pts',(374.434409083254,-9.6966378911308,-1.58361363200077));
#47853=CARTESIAN_POINT('Ctrl Pts',(374.387863196296,-9.69077178522504,-1.68942822973297));
#47854=CARTESIAN_POINT('Ctrl Pts',(374.336584697648,-9.68490567931928,-1.79333324928324));
#47855=CARTESIAN_POINT('Ctrl Pts',(374.28075491153,-9.67903957341352,-1.89487746388453));
#47856=CARTESIAN_POINT('Ctrl Pts',(374.224982294401,-9.67317947432548,-1.99631769850368));
#47857=CARTESIAN_POINT('Ctrl Pts',(374.164667857709,-9.66731937523744,-2.095401576769));
#47858=CARTESIAN_POINT('Ctrl Pts',(374.100040434264,-9.6614592761494,-2.19169911796409));
#47859=CARTESIAN_POINT('Ctrl Pts',(374.03308140082,-9.6553877580553,-2.29147085475558));
#47860=CARTESIAN_POINT('Ctrl Pts',(373.961492481339,-9.64931623996119,-2.38825099575935));
#47861=CARTESIAN_POINT('Ctrl Pts',(373.885579679766,-9.64324472186708,-2.48159026954188));
#47862=CARTESIAN_POINT('Ctrl Pts',(373.812394485822,-9.63739135827033,-2.57157578862253));
#47863=CARTESIAN_POINT('Ctrl Pts',(373.735191066436,-9.63153799467359,-2.65836310329154));
#47864=CARTESIAN_POINT('Ctrl Pts',(373.654286387342,-9.62568463107683,-2.74158101587052));
#47865=CARTESIAN_POINT('Ctrl Pts',(373.573393855814,-9.61983214634293,-2.82478643355997));
#47866=CARTESIAN_POINT('Ctrl Pts',(373.488801457496,-9.61397966160902,-2.90442321865074));
#47867=CARTESIAN_POINT('Ctrl Pts',(373.400864047524,-9.60812717687512,-2.98015597452925));
#47868=CARTESIAN_POINT('Ctrl Pts',(373.312918574873,-9.60227415554695,-3.05589567408463));
#47869=CARTESIAN_POINT('Ctrl Pts',(373.221627793962,-9.59642113421877,-3.12773036324287));
#47870=CARTESIAN_POINT('Ctrl Pts',(373.127380209077,-9.5905681128906,-3.19536445999062));
#47871=CARTESIAN_POINT('Ctrl Pts',(373.033101190801,-9.58471313946678,-3.26302111401576));
#47872=CARTESIAN_POINT('Ctrl Pts',(372.935863743112,-9.57885816604297,-3.32647414910033));
#47873=CARTESIAN_POINT('Ctrl Pts',(372.836085346331,-9.57300319261915,-3.38547129710759));
#47874=CARTESIAN_POINT('Ctrl Pts',(372.736193863554,-9.56714158333499,-3.44453531080426));
#47875=CARTESIAN_POINT('Ctrl Pts',(372.633756039528,-9.56127997405084,-3.49913314718231));
#47876=CARTESIAN_POINT('Ctrl Pts',(372.529214032112,-9.55541836476668,-3.54905845863237));
#47877=CARTESIAN_POINT('Ctrl Pts',(372.424601531253,-9.54955280295634,-3.59901743508659));
#47878=CARTESIAN_POINT('Ctrl Pts',(372.317882401114,-9.543687241146,-3.64429745186442));
#47879=CARTESIAN_POINT('Ctrl Pts',(372.209517227151,-9.53782167933565,-3.68474092467185));
#47880=CARTESIAN_POINT('Ctrl Pts',(372.100993596725,-9.53194754063532,-3.72524353575592));
#47881=CARTESIAN_POINT('Ctrl Pts',(371.990819510435,-9.52607340193499,-3.76089536180038));
#47882=CARTESIAN_POINT('Ctrl Pts',(371.879469157034,-9.52019926323466,-3.79158908007496));
#47883=CARTESIAN_POINT('Ctrl Pts',(371.851310470467,-9.51871378945339,-3.79935102034784));
#47884=CARTESIAN_POINT('Ctrl Pts',(371.823076601891,-9.51722831567212,-3.80679614594573));
#47885=CARTESIAN_POINT('Ctrl Pts',(371.794775288842,-9.51574284189085,-3.8139232444251));
#47886=CARTESIAN_POINT('Ctrl Pts',(371.682869495356,-9.50986915250028,-3.84210439662827));
#47887=CARTESIAN_POINT('Ctrl Pts',(371.5695359611,-9.50399546310971,-3.86540310393339));
#47888=CARTESIAN_POINT('Ctrl Pts',(371.455238587611,-9.49812177371915,-3.88367692291827));
#47889=CARTESIAN_POINT('Ctrl Pts',(371.34108878277,-9.49225566781339,-3.90192714868608));
#47890=CARTESIAN_POINT('Ctrl Pts',(371.22597801765,-9.48638956190764,-3.91516532321926));
#47891=CARTESIAN_POINT('Ctrl Pts',(371.11038375923,-9.48052345600188,-3.92329920035943));
#47892=CARTESIAN_POINT('Ctrl Pts',(370.994907867858,-9.47466335691384,-3.93142474851303));
#47893=CARTESIAN_POINT('Ctrl Pts',(370.878949877639,-9.4688032578258,-3.93445636685655));
#47894=CARTESIAN_POINT('Ctrl Pts',(370.762995157184,-9.46294315873777,-3.93235324875953));
#47895=CARTESIAN_POINT('Ctrl Pts',(370.642857054951,-9.45687164064366,-3.93017425495955));
#47896=CARTESIAN_POINT('Ctrl Pts',(370.522722908879,-9.45080012254955,-3.92248295906194));
#47897=CARTESIAN_POINT('Ctrl Pts',(370.403136132927,-9.44472860445545,-3.9092929442652));
#47898=CARTESIAN_POINT('Ctrl Pts',(370.287846205406,-9.4388752408587,-3.8965768572413));
#47899=CARTESIAN_POINT('Ctrl Pts',(370.173065435921,-9.43302187726194,-3.87875044681709));
#47900=CARTESIAN_POINT('Ctrl Pts',(370.059277574931,-9.4271685136652,-3.85587883199449));
#47901=CARTESIAN_POINT('Ctrl Pts',(369.945506798805,-9.42131602893129,-3.83301065126789));
#47902=CARTESIAN_POINT('Ctrl Pts',(369.83272903968,-9.41546354419739,-3.80509885377092));
#47903=CARTESIAN_POINT('Ctrl Pts',(369.721418504306,-9.40961105946348,-3.77225980536563));
#47904=CARTESIAN_POINT('Ctrl Pts',(369.61009776325,-9.4037580381353,-3.73941774606053));
#47905=CARTESIAN_POINT('Ctrl Pts',(369.500244909649,-9.39790501680713,-3.70164765469679));
#47906=CARTESIAN_POINT('Ctrl Pts',(369.392318935258,-9.39205199547895,-3.65911575665266));
#47907=CARTESIAN_POINT('Ctrl Pts',(369.284356965469,-9.38619702205512,-3.61656967339911));
#47908=CARTESIAN_POINT('Ctrl Pts',(369.178323536939,-9.38034204863129,-3.56925877688493));
#47909=CARTESIAN_POINT('Ctrl Pts',(369.074656952618,-9.37448707520746,-3.51739712214563));
#47910=CARTESIAN_POINT('Ctrl Pts',(368.970872875539,-9.36862546592331,-3.46547668888213));
#47911=CARTESIAN_POINT('Ctrl Pts',(368.869461366498,-9.36276385663915,-3.40899538788337));
#47912=CARTESIAN_POINT('Ctrl Pts',(368.770835518993,-9.35690224735499,-3.34821290486675));
#47913=CARTESIAN_POINT('Ctrl Pts',(368.672143167354,-9.35103668554464,-3.28738943577538));
#47914=CARTESIAN_POINT('Ctrl Pts',(368.576240558479,-9.34517112373429,-3.22225924102581));
#47915=CARTESIAN_POINT('Ctrl Pts',(368.483509799443,-9.33930556192394,-3.15312392624795));
#47916=CARTESIAN_POINT('Ctrl Pts',(368.390643445294,-9.33343142322361,-3.08388751868344));
#47917=CARTESIAN_POINT('Ctrl Pts',(368.300958516057,-9.32755728452328,-3.0106345633989));
#47918=CARTESIAN_POINT('Ctrl Pts',(368.214802258098,-9.32168314582295,-2.9337053442518));
#47919=CARTESIAN_POINT('Ctrl Pts',(368.193014746972,-9.3201976720417,-2.91425120060883));
#47920=CARTESIAN_POINT('Ctrl Pts',(368.171452700821,-9.31871219826044,-2.89456213268467));
#47921=CARTESIAN_POINT('Ctrl Pts',(368.150121333064,-9.31722672447919,-2.87464398511513));
#47922=CARTESIAN_POINT('Ctrl Pts',(368.067026222552,-9.31144014719931,-2.79705399218618));
#47923=CARTESIAN_POINT('Ctrl Pts',(367.987139937561,-9.30565356991942,-2.71571004166305));
#47924=CARTESIAN_POINT('Ctrl Pts',(367.910828487414,-9.29986699263954,-2.63091218553541));
#47925=CARTESIAN_POINT('Ctrl Pts',(367.83076645626,-9.29379601469888,-2.54194665564336));
#47926=CARTESIAN_POINT('Ctrl Pts',(367.754640001564,-9.28772503675821,-2.44917930045951));
#47927=CARTESIAN_POINT('Ctrl Pts',(367.682832597279,-9.28165405881755,-2.35300439471732));
#47928=CARTESIAN_POINT('Ctrl Pts',(367.614559204841,-9.27588186493941,-2.26156275095226));
#47929=CARTESIAN_POINT('Ctrl Pts',(367.550190192005,-9.27010967106127,-2.1670413479476));
#47930=CARTESIAN_POINT('Ctrl Pts',(367.490016455998,-9.26433747718313,-2.06981573201827));
#47931=CARTESIAN_POINT('Ctrl Pts',(367.429879896641,-9.25856884949261,-1.97265018420083));
#47932=CARTESIAN_POINT('Ctrl Pts',(367.373933687928,-9.25280022180208,-1.87278410441214));
#47933=CARTESIAN_POINT('Ctrl Pts',(367.32242625392,-9.24703159411156,-1.77062316564955));
#47934=CARTESIAN_POINT('Ctrl Pts',(367.270937320453,-9.24126503840821,-1.6684989212562));
#47935=CARTESIAN_POINT('Ctrl Pts',(367.223884184249,-9.23549848270486,-1.56408183673553));
#47936=CARTESIAN_POINT('Ctrl Pts',(367.181469579154,-9.22973192700151,-1.45780262265575));
#47937=CARTESIAN_POINT('Ctrl Pts',(367.139059240161,-9.22396595130408,-1.35153409824537));
#47938=CARTESIAN_POINT('Ctrl Pts',(367.101286660911,-9.21819997560666,-1.24340421338312));
#47939=CARTESIAN_POINT('Ctrl Pts',(367.068306294295,-9.21243399990924,-1.13386328012323));
#47940=CARTESIAN_POINT('Ctrl Pts',(367.035307369128,-9.20666477961016,-1.024260706525));
#47941=CARTESIAN_POINT('Ctrl Pts',(367.007106164992,-9.20089555931108,-0.913245907654856));
#47942=CARTESIAN_POINT('Ctrl Pts',(366.983807043069,-9.19512633901201,-0.801283658189311));
#47943=CARTESIAN_POINT('Ctrl Pts',(366.9605002699,-9.18935522414678,-0.689284641209677));
#47944=CARTESIAN_POINT('Ctrl Pts',(366.942098854974,-9.18358410928155,-0.576337974633217));
#47945=CARTESIAN_POINT('Ctrl Pts',(366.928655620417,-9.17781299441632,-0.462916324213755));
#47946=CARTESIAN_POINT('Ctrl Pts',(366.915198115606,-9.17203575340115,-0.349374274520911));
#47947=CARTESIAN_POINT('Ctrl Pts',(366.906709328686,-9.16625851238598,-0.235356659343858));
#47948=CARTESIAN_POINT('Ctrl Pts',(366.903190035608,-9.16048127137082,-0.121338705950509));
#47949=CARTESIAN_POINT('Ctrl Pts',(366.901907185002,-9.15837535493508,-0.079776949847682));
#47950=CARTESIAN_POINT('Ctrl Pts',(366.901284152064,-9.15626943849936,-0.0382151271236437));
#47951=CARTESIAN_POINT('Ctrl Pts',(366.901319257773,-9.15416352206362,0.00332388066085588));
#47952=CARTESIAN_POINT('',(366.901318679092,-7.90416352198934,-0.00254877927961847));
#47953=CARTESIAN_POINT('Ctrl Pts',(366.901319257774,-9.15416352203497,0.00332388122593332));
#47954=CARTESIAN_POINT('Ctrl Pts',(366.901468264492,-9.14522492907225,0.179636804359732));
#47955=CARTESIAN_POINT('Ctrl Pts',(366.9134762834,-9.13628633610951,0.355464946286474));
#47956=CARTESIAN_POINT('Ctrl Pts',(366.937130866369,-9.12734774314678,0.529549421191803));
#47957=CARTESIAN_POINT('Ctrl Pts',(366.94474980792,-9.12446869778703,0.585620561445061));
#47958=CARTESIAN_POINT('Ctrl Pts',(366.953576681388,-9.12158965242729,0.641511085305567));
#47959=CARTESIAN_POINT('Ctrl Pts',(366.963603491617,-9.11871060706754,0.697179554237403));
#47960=CARTESIAN_POINT('Ctrl Pts',(366.984059705919,-9.11283691767697,0.810751677804974));
#47961=CARTESIAN_POINT('Ctrl Pts',(367.009552771227,-9.10696322828641,0.923611871718653));
#47962=CARTESIAN_POINT('Ctrl Pts',(367.040021228329,-9.10108953889585,1.03527876550764));
#47963=CARTESIAN_POINT('Ctrl Pts',(367.070450347791,-9.09522343299009,1.14680148684608));
#47964=CARTESIAN_POINT('Ctrl Pts',(367.10584197666,-9.08935732708435,1.25713357699809));
#47965=CARTESIAN_POINT('Ctrl Pts',(367.146083329971,-9.08349122117859,1.36580199936962));
#47966=CARTESIAN_POINT('Ctrl Pts',(367.186283476648,-9.07763112209055,1.47435914666115));
#47967=CARTESIAN_POINT('Ctrl Pts',(367.231323327252,-9.07177102300251,1.58125562959267));
#47968=CARTESIAN_POINT('Ctrl Pts',(367.281039974081,-9.06591092391447,1.68603241771641));
#47969=CARTESIAN_POINT('Ctrl Pts',(367.332550284105,-9.05983940582036,1.79458931332146));
#47970=CARTESIAN_POINT('Ctrl Pts',(367.389081099068,-9.05376788772626,1.90087024314777));
#47971=CARTESIAN_POINT('Ctrl Pts',(367.450396029607,-9.04769636963215,2.00438571429015));
#47972=CARTESIAN_POINT('Ctrl Pts',(367.509507865691,-9.0418430060354,2.10418179182689));
#47973=CARTESIAN_POINT('Ctrl Pts',(367.573065711195,-9.03598964243865,2.20140733490711));
#47974=CARTESIAN_POINT('Ctrl Pts',(367.640810818989,-9.0301362788419,2.2956484535508));
#47975=CARTESIAN_POINT('Ctrl Pts',(367.708545755083,-9.02428379410799,2.3898754222077));
#47976=CARTESIAN_POINT('Ctrl Pts',(367.780466462285,-9.01843130937409,2.48111852204744));
#47977=CARTESIAN_POINT('Ctrl Pts',(367.856271437838,-9.01257882464019,2.56899368387861));
#47978=CARTESIAN_POINT('Ctrl Pts',(367.93208336369,-9.00672580331202,2.65687690268219));
#47979=CARTESIAN_POINT('Ctrl Pts',(368.011779995979,-9.00087278198384,2.74139125677391));
#47980=CARTESIAN_POINT('Ctrl Pts',(368.095020678199,-8.99501976065567,2.82218709282411));
#47981=CARTESIAN_POINT('Ctrl Pts',(368.178289122796,-8.98916478723183,2.90300987584619));
#47982=CARTESIAN_POINT('Ctrl Pts',(368.265103671397,-8.983309813808,2.98011138715295));
#47983=CARTESIAN_POINT('Ctrl Pts',(368.355088619603,-8.97745484038416,3.05318053956148));
#47984=CARTESIAN_POINT('Ctrl Pts',(368.445175554188,-8.97159323110001,3.12633250646872));
#47985=CARTESIAN_POINT('Ctrl Pts',(368.538439739366,-8.96573162181585,3.19544273213369));
#47986=CARTESIAN_POINT('Ctrl Pts',(368.634474289843,-8.95987001253169,3.26024190768866));
#47987=CARTESIAN_POINT('Ctrl Pts',(368.730573597122,-8.95400445072135,3.3250847778036));
#47988=CARTESIAN_POINT('Ctrl Pts',(368.829446637963,-8.948138888911,3.38561059421203));
#47989=CARTESIAN_POINT('Ctrl Pts',(368.930661108447,-8.94227332710066,3.44159555992084));
#47990=CARTESIAN_POINT('Ctrl Pts',(369.032023579312,-8.93639918840032,3.49766238938069));
#47991=CARTESIAN_POINT('Ctrl Pts',(369.135733944158,-8.93052504969999,3.54917493361567));
#47992=CARTESIAN_POINT('Ctrl Pts',(369.241339030983,-8.92465091099966,3.59595710095255));
#47993=CARTESIAN_POINT('Ctrl Pts',(369.268044833424,-8.9231654372184,3.60778754734726));
#47994=CARTESIAN_POINT('Ctrl Pts',(369.294871725698,-8.92167996343715,3.61931573371251));
#47995=CARTESIAN_POINT('Ctrl Pts',(369.321812233735,-8.92019448965589,3.63053931957986));
#47996=CARTESIAN_POINT('Ctrl Pts',(369.428337288725,-8.91432080026535,3.67491833054907));
#47997=CARTESIAN_POINT('Ctrl Pts',(369.536994628475,-8.9084471108748,3.71467889225625));
#47998=CARTESIAN_POINT('Ctrl Pts',(369.64734643598,-8.90257342148426,3.74961169384846));
#47999=CARTESIAN_POINT('Ctrl Pts',(369.757555768934,-8.89670731557853,3.78449939391202));
#48000=CARTESIAN_POINT('Ctrl Pts',(369.869454828706,-8.8908412096728,3.81457160588909));
#48001=CARTESIAN_POINT('Ctrl Pts',(369.982584977134,-8.88497510376707,3.83966666623377));
#48002=CARTESIAN_POINT('Ctrl Pts',(370.09559928173,-8.87911500467905,3.86473602955636));
#48003=CARTESIAN_POINT('Ctrl Pts',(370.209841766562,-8.87325490559103,3.8848382897476));
#48004=CARTESIAN_POINT('Ctrl Pts',(370.324838390928,-8.86739480650302,3.89986149465579));
#48005=CARTESIAN_POINT('Ctrl Pts',(370.443983831153,-8.8613232884089,3.91542670252374));
#48006=CARTESIAN_POINT('Ctrl Pts',(370.563938422951,-8.85525177031479,3.92553931799925));
#48007=CARTESIAN_POINT('Ctrl Pts',(370.684162692671,-8.84918025222068,3.93013262215912));
#48008=CARTESIAN_POINT('Ctrl Pts',(370.800067208299,-8.84332688862395,3.93456088522963));
#48009=CARTESIAN_POINT('Ctrl Pts',(370.916221907645,-8.83747352502722,3.93385962051807));
#48010=CARTESIAN_POINT('Ctrl Pts',(371.032138726429,-8.8316201614305,3.92802188157401));
#48011=CARTESIAN_POINT('Ctrl Pts',(371.148038140694,-8.82576767669662,3.92218501914681));
#48012=CARTESIAN_POINT('Ctrl Pts',(371.263699332905,-8.81991519196274,3.9112132367454));
#48013=CARTESIAN_POINT('Ctrl Pts',(371.378636119195,-8.81406270722886,3.89515168194138));
#48014=CARTESIAN_POINT('Ctrl Pts',(371.493583443644,-8.80820968590071,3.87908865450844));
#48015=CARTESIAN_POINT('Ctrl Pts',(371.607805820948,-8.80235666457257,3.85793498417039));
#48016=CARTESIAN_POINT('Ctrl Pts',(371.720824761537,-8.79650364324442,3.83178737686651));
#48017=CARTESIAN_POINT('Ctrl Pts',(371.833881396125,-8.79064866982062,3.80563104883061));
#48018=CARTESIAN_POINT('Ctrl Pts',(371.945733393598,-8.78479369639682,3.77447756498198));
#48019=CARTESIAN_POINT('Ctrl Pts',(372.055915672024,-8.77893872297303,3.7384739893574));
#48020=CARTESIAN_POINT('Ctrl Pts',(372.166222827911,-8.7730771136889,3.70242960830435));
#48021=CARTESIAN_POINT('Ctrl Pts',(372.274856094681,-8.76721550440477,3.66152429227753));
#48022=CARTESIAN_POINT('Ctrl Pts',(372.38136859359,-8.76135389512064,3.61595395528367));
#48023=CARTESIAN_POINT('Ctrl Pts',(372.48795291466,-8.75548833331032,3.5703528898769));
#48024=CARTESIAN_POINT('Ctrl Pts',(372.592413248969,-8.7496227715,3.52008071851767));
#48025=CARTESIAN_POINT('Ctrl Pts',(372.694327182081,-8.74375720968968,3.4653793871041));
#48026=CARTESIAN_POINT('Ctrl Pts',(372.796390138358,-8.73788307098938,3.41059806892765));
#48027=CARTESIAN_POINT('Ctrl Pts',(372.895898908682,-8.73200893228908,3.35137487567747));
#48028=CARTESIAN_POINT('Ctrl Pts',(372.992459852983,-8.72613479358878,3.28799515037324));
#48029=CARTESIAN_POINT('Ctrl Pts',(373.016878539431,-8.72464931980726,3.27196745252298));
#48030=CARTESIAN_POINT('Ctrl Pts',(373.041108878354,-8.72316384602574,3.25567414389969));
#48031=CARTESIAN_POINT('Ctrl Pts',(373.065144851275,-8.72167837224423,3.2391202362318));
#48032=CARTESIAN_POINT('Ctrl Pts',(373.160185127915,-8.71580468285365,3.17366468053539));
#48033=CARTESIAN_POINT('Ctrl Pts',(373.252500417247,-8.70993099346308,3.10391364395067));
#48034=CARTESIAN_POINT('Ctrl Pts',(373.341677488955,-8.7040573040725,3.03012155814021));
#48035=CARTESIAN_POINT('Ctrl Pts',(373.430739424686,-8.69819119816673,2.95642474484502));
#48036=CARTESIAN_POINT('Ctrl Pts',(373.516670884969,-8.69232509226097,2.87869751895253));
#48037=CARTESIAN_POINT('Ctrl Pts',(373.599087390548,-8.68645898635521,2.79723763836516));
#48038=CARTESIAN_POINT('Ctrl Pts',(373.681419502674,-8.68059888726716,2.71586117165772));
#48039=CARTESIAN_POINT('Ctrl Pts',(373.760243527249,-8.67473878817911,2.6307599416109));
#48040=CARTESIAN_POINT('Ctrl Pts',(373.835208408026,-8.66887868909106,2.54227159802004));
#48041=CARTESIAN_POINT('Ctrl Pts',(373.91287785068,-8.66280717099696,2.4505907968669));
#48042=CARTESIAN_POINT('Ctrl Pts',(373.986404085922,-8.65673565290285,2.35527415710136));
#48043=CARTESIAN_POINT('Ctrl Pts',(374.055438595521,-8.65066413480875,2.25673883370292));
#48044=CARTESIAN_POINT('Ctrl Pts',(374.12199264002,-8.64481077121198,2.1617439632214));
#48045=CARTESIAN_POINT('Ctrl Pts',(374.184371929043,-8.63895740761523,2.06375809560105));
#48046=CARTESIAN_POINT('Ctrl Pts',(374.242306041148,-8.63310404401846,1.96318758934822));
#48047=CARTESIAN_POINT('Ctrl Pts',(374.30023145464,-8.62725155928455,1.86263218341846));
#48048=CARTESIAN_POINT('Ctrl Pts',(374.353712812143,-8.62139907455064,1.75949326839322));
#48049=CARTESIAN_POINT('Ctrl Pts',(374.402524486615,-8.61554658981672,1.65420386331987));
#48050=CARTESIAN_POINT('Ctrl Pts',(374.451340636463,-8.60969356848854,1.54890480462174));
#48051=CARTESIAN_POINT('Ctrl Pts',(374.495486078387,-8.60384054716035,1.4414552387634));
#48052=CARTESIAN_POINT('Ctrl Pts',(374.534782681401,-8.59798752583217,1.33230966949345));
#48053=CARTESIAN_POINT('Ctrl Pts',(374.574092390591,-8.59213255240833,1.22312769806832));
#48054=CARTESIAN_POINT('Ctrl Pts',(374.6085499053,-8.58627757898449,1.11224898697031));
#48055=CARTESIAN_POINT('Ctrl Pts',(374.638026679255,-8.58042260556066,1.00014407300846));
#48056=CARTESIAN_POINT('Ctrl Pts',(374.667536861347,-8.57456099627649,0.887912102526002));
#48057=CARTESIAN_POINT('Ctrl Pts',(374.692054930424,-8.56869938699233,0.774451555122436));
#48058=CARTESIAN_POINT('Ctrl Pts',(374.711503257349,-8.56283777770817,0.660244153358279));
#48059=CARTESIAN_POINT('Ctrl Pts',(374.730964698422,-8.55697221589781,0.545959740704368));
#48060=CARTESIAN_POINT('Ctrl Pts',(374.745349539085,-8.55110665408746,0.430927879829411));
#48061=CARTESIAN_POINT('Ctrl Pts',(374.754632093489,-8.54524109227711,0.315634690071573));
#48062=CARTESIAN_POINT('Ctrl Pts',(374.763928221264,-8.53936695357677,0.200172913392809));
#48063=CARTESIAN_POINT('Ctrl Pts',(374.76810715806,-8.53349281487642,0.0844494564905184));
#48064=CARTESIAN_POINT('Ctrl Pts',(374.76719528383,-8.52761867617608,-0.0310502146323147));
#48065=CARTESIAN_POINT('Ctrl Pts',(374.766964685724,-8.52613320239491,-0.0602581959107494));
#48066=CARTESIAN_POINT('Ctrl Pts',(374.766408787816,-8.52464772861374,-0.0894518974122133));
#48067=CARTESIAN_POINT('Ctrl Pts',(374.765528538828,-8.52316225483257,-0.11862354485694));
#48068=CARTESIAN_POINT('Ctrl Pts',(374.762047959628,-8.51728856544201,-0.233970714408904));
#48069=CARTESIAN_POINT('Ctrl Pts',(374.753480612594,-8.51141487605144,-0.349356676786575));
#48070=CARTESIAN_POINT('Ctrl Pts',(374.739816282563,-8.50554118666087,-0.464296261488693));
#48071=CARTESIAN_POINT('Ctrl Pts',(374.726169594465,-8.49967508075512,-0.579087448388813));
#48072=CARTESIAN_POINT('Ctrl Pts',(374.707439058521,-8.49380897484937,-0.693432997206952));
#48073=CARTESIAN_POINT('Ctrl Pts',(374.683666453169,-8.48794286894362,-0.806848409615465));
#48074=CARTESIAN_POINT('Ctrl Pts',(374.659918190663,-8.48208276985558,-0.920147686086541));
#48075=CARTESIAN_POINT('Ctrl Pts',(374.631138212665,-8.47622267076755,-1.03251831869128));
#48076=CARTESIAN_POINT('Ctrl Pts',(374.597419938021,-8.47036257167951,-1.14348226894711));
#48077=CARTESIAN_POINT('Ctrl Pts',(374.562485184951,-8.4642910535854,-1.2584495453789));
#48078=CARTESIAN_POINT('Ctrl Pts',(374.522249136021,-8.4582195354913,-1.37190627480284));
#48079=CARTESIAN_POINT('Ctrl Pts',(374.476873394784,-8.45214801739719,-1.48333345093183));
#48080=CARTESIAN_POINT('Ctrl Pts',(374.433128040193,-8.44629465380044,-1.59075695957209));
#48081=CARTESIAN_POINT('Ctrl Pts',(374.384606152586,-8.44044129020369,-1.69629383642295));
#48082=CARTESIAN_POINT('Ctrl Pts',(374.331502600168,-8.43458792660694,-1.79949655341166));
#48083=CARTESIAN_POINT('Ctrl Pts',(374.27840702107,-8.42873544187304,-1.90268377485972));
#48084=CARTESIAN_POINT('Ctrl Pts',(374.220731333986,-8.42288295713914,-2.00353716603838));
#48085=CARTESIAN_POINT('Ctrl Pts',(374.158717093655,-8.41703047240523,-2.10163238703123));
#48086=CARTESIAN_POINT('Ctrl Pts',(374.096697167452,-8.41117745107706,-2.19973660203876));
#48087=CARTESIAN_POINT('Ctrl Pts',(374.030338118017,-8.40532442974889,-2.29508179491122));
#48088=CARTESIAN_POINT('Ctrl Pts',(373.959925301916,-8.39947140842071,-2.38727188997809));
#48089=CARTESIAN_POINT('Ctrl Pts',(373.889489001781,-8.39361643499689,-2.47949273222214));
#48090=CARTESIAN_POINT('Ctrl Pts',(373.814996497208,-8.38776146157306,-2.56855605608216));
#48091=CARTESIAN_POINT('Ctrl Pts',(373.73677349781,-8.38190648814923,-2.65409876063602));
#48092=CARTESIAN_POINT('Ctrl Pts',(373.65846184269,-8.37604487886508,-2.73973841685784));
#48093=CARTESIAN_POINT('Ctrl Pts',(373.576411532798,-8.37018326958093,-2.82184918457374));
#48094=CARTESIAN_POINT('Ctrl Pts',(373.490985279885,-8.36432166029678,-2.90010468502701));
#48095=CARTESIAN_POINT('Ctrl Pts',(373.405501423424,-8.35845609848644,-2.97841295373893));
#48096=CARTESIAN_POINT('Ctrl Pts',(373.31663740699,-8.3525905366761,-3.05286051407759));
#48097=CARTESIAN_POINT('Ctrl Pts',(373.224787795936,-8.34672497486576,-3.12316225210772));
#48098=CARTESIAN_POINT('Ctrl Pts',(373.132803878223,-8.34085083616543,-3.19356678852152));
#48099=CARTESIAN_POINT('Ctrl Pts',(373.037825990666,-8.3349766974651,-3.25981316853759));
#48100=CARTESIAN_POINT('Ctrl Pts',(372.940276374979,-8.32910255876476,-3.32166038370065));
#48101=CARTESIAN_POINT('Ctrl Pts',(372.915607669681,-8.32761708498348,-3.33730053475203));
#48102=CARTESIAN_POINT('Ctrl Pts',(372.890774615676,-8.3261316112022,-3.35265959262464));
#48103=CARTESIAN_POINT('Ctrl Pts',(372.865784260062,-8.32464613742092,-3.36773414002491));
#48104=CARTESIAN_POINT('Ctrl Pts',(372.766970273246,-8.31877244803035,-3.42734017969275));
#48105=CARTESIAN_POINT('Ctrl Pts',(372.665366103292,-8.31289875863979,-3.48269279839185));
#48106=CARTESIAN_POINT('Ctrl Pts',(372.561373905041,-8.30702506924922,-3.53352039669837));
#48107=CARTESIAN_POINT('Ctrl Pts',(372.457515970487,-8.30115896334346,-3.58428237180044));
#48108=CARTESIAN_POINT('Ctrl Pts',(372.35127650684,-8.2952928574377,-3.6305307650198));
#48109=CARTESIAN_POINT('Ctrl Pts',(372.243085290337,-8.28942675153194,-3.67203803195589));
#48110=CARTESIAN_POINT('Ctrl Pts',(372.135004860261,-8.2835666524439,-3.71350279597942));
#48111=CARTESIAN_POINT('Ctrl Pts',(372.024977036089,-8.27770655335586,-3.750235943319));
#48112=CARTESIAN_POINT('Ctrl Pts',(371.913454160552,-8.27184645426782,-3.78205682535393));
#48113=CARTESIAN_POINT('Ctrl Pts',(371.797907794091,-8.26577493617372,-3.8150257322176));
#48114=CARTESIAN_POINT('Ctrl Pts',(371.680756869227,-8.25970341807961,-3.84272103666929));
#48115=CARTESIAN_POINT('Ctrl Pts',(371.56252511784,-8.2536318999855,-3.86499717719948));
#48116=CARTESIAN_POINT('Ctrl Pts',(371.448541527769,-8.24777853638875,-3.88647291819778));
#48117=CARTESIAN_POINT('Ctrl Pts',(371.333553885218,-8.241925172792,-3.90291213998364));
#48118=CARTESIAN_POINT('Ctrl Pts',(371.218043891446,-8.23607180919525,-3.91423598261404));
#48119=CARTESIAN_POINT('Ctrl Pts',(371.10255124111,-8.23021932446134,-3.92555812500758));
#48120=CARTESIAN_POINT('Ctrl Pts',(370.986536806563,-8.22436683972744,-3.93176637513341));
#48121=CARTESIAN_POINT('Ctrl Pts',(370.870488113088,-8.21851435499353,-3.9328336746297));
#48122=CARTESIAN_POINT('Ctrl Pts',(370.754428779506,-8.21266133366535,-3.93390107198302));
#48123=CARTESIAN_POINT('Ctrl Pts',(370.638335593902,-8.20680831233718,-3.92982657789512));
#48124=CARTESIAN_POINT('Ctrl Pts',(370.522696076278,-8.200955291009,-3.92063526333846));
#48125=CARTESIAN_POINT('Ctrl Pts',(370.407017990641,-8.19510031758518,-3.91144088330089));
#48126=CARTESIAN_POINT('Ctrl Pts',(370.291794285475,-8.18924534416136,-3.89712632209612));
#48127=CARTESIAN_POINT('Ctrl Pts',(370.177506647615,-8.18339037073754,-3.87776843560651));
#48128=CARTESIAN_POINT('Ctrl Pts',(370.063089479396,-8.17752876145338,-3.85838860943898));
#48129=CARTESIAN_POINT('Ctrl Pts',(369.949610903571,-8.17166715216923,-3.83395411830563));
#48130=CARTESIAN_POINT('Ctrl Pts',(369.837541808259,-8.16580554288508,-3.80459281871059));
#48131=CARTESIAN_POINT('Ctrl Pts',(369.725397143934,-8.15993998107473,-3.77521172057556));
#48132=CARTESIAN_POINT('Ctrl Pts',(369.61466424628,-8.15407441926437,-3.74089732076272));
#48133=CARTESIAN_POINT('Ctrl Pts',(369.505796596407,-8.14820885745402,-3.70182661265816));
#48134=CARTESIAN_POINT('Ctrl Pts',(369.396769755327,-8.14233471875369,-3.66269877359569));
#48135=CARTESIAN_POINT('Ctrl Pts',(369.289613986171,-8.13646058005336,-3.61880090204676));
#48136=CARTESIAN_POINT('Ctrl Pts',(369.184760711482,-8.13058644135303,-3.57035715806267));
#48137=CARTESIAN_POINT('Ctrl Pts',(369.158245030057,-8.12910096757177,-3.55810652605933));
#48138=CARTESIAN_POINT('Ctrl Pts',(369.131876458437,-8.12761549379052,-3.5455654072616));
#48139=CARTESIAN_POINT('Ctrl Pts',(369.105661688502,-8.12613002000926,-3.53273787085453));
#48140=CARTESIAN_POINT('Ctrl Pts',(369.002006263555,-8.1202563306187,-3.4820167033375));
#48141=CARTESIAN_POINT('Ctrl Pts',(368.900412436809,-8.11438264122813,-3.4266451030718));
#48142=CARTESIAN_POINT('Ctrl Pts',(368.801326447354,-8.10850895183756,-3.366813767297));
#48143=CARTESIAN_POINT('Ctrl Pts',(368.702368387222,-8.10264284593182,-3.30705967939769));
#48144=CARTESIAN_POINT('Ctrl Pts',(368.605912075792,-8.09677674002607,-3.24285751824571));
#48145=CARTESIAN_POINT('Ctrl Pts',(368.512381706195,-8.09091063412032,-3.17444507420126));
#48146=CARTESIAN_POINT('Ctrl Pts',(368.418947110506,-8.08505053503229,-3.10610268362794));
#48147=CARTESIAN_POINT('Ctrl Pts',(368.328432828584,-8.07919043594426,-3.03355882810736));
#48148=CARTESIAN_POINT('Ctrl Pts',(368.241235880182,-8.07333033685623,-2.95709568345119));
#48149=CARTESIAN_POINT('Ctrl Pts',(368.15089306481,-8.06725881876212,-2.87787392297609));
#48150=CARTESIAN_POINT('Ctrl Pts',(368.064111852556,-8.06118730066801,-2.79444496945922));
#48151=CARTESIAN_POINT('Ctrl Pts',(367.981298479933,-8.0551157825739,-2.70717000863017));
#48152=CARTESIAN_POINT('Ctrl Pts',(367.901460657971,-8.04926241897715,-2.62303090689219));
#48153=CARTESIAN_POINT('Ctrl Pts',(367.825310756227,-8.04340905538041,-2.53531774700873));
#48154=CARTESIAN_POINT('Ctrl Pts',(367.753176176164,-8.03755569178366,-2.44439255560225));
#48155=CARTESIAN_POINT('Ctrl Pts',(367.681052426865,-8.03170320704976,-2.35348101630726));
#48156=CARTESIAN_POINT('Ctrl Pts',(367.612943057185,-8.02585072231586,-2.25935872800847));
#48157=CARTESIAN_POINT('Ctrl Pts',(367.54913509657,-8.01999823758195,-2.16242069343169));
#48158=CARTESIAN_POINT('Ctrl Pts',(367.485321285622,-8.01414521625378,-2.06547377093875));
#48159=CARTESIAN_POINT('Ctrl Pts',(367.425809894898,-8.00829219492561,-1.96571093407117));
#48160=CARTESIAN_POINT('Ctrl Pts',(367.370844146293,-8.00243917359744,-1.86355544092471));
#48161=CARTESIAN_POINT('Ctrl Pts',(367.31586006555,-7.99658420017363,-1.76136587694856));
#48162=CARTESIAN_POINT('Ctrl Pts',(367.265424837196,-7.99072922674982,-1.65678243353877));
#48163=CARTESIAN_POINT('Ctrl Pts',(367.219735005643,-7.98487425332601,-1.5502515402271));
#48164=CARTESIAN_POINT('Ctrl Pts',(367.173993390536,-7.97901264404186,-1.44359990783109));
#48165=CARTESIAN_POINT('Ctrl Pts',(367.133008069927,-7.97315103475771,-1.33499680003515));
#48166=CARTESIAN_POINT('Ctrl Pts',(367.096926877922,-7.96728942547356,-1.22490722004983));
#48167=CARTESIAN_POINT('Ctrl Pts',(367.060821356105,-7.96142386366322,-1.11474340585235));
#48168=CARTESIAN_POINT('Ctrl Pts',(367.02962665854,-7.95555830185289,-1.00309152050772));
#48169=CARTESIAN_POINT('Ctrl Pts',(367.003439892718,-7.94969274004256,-0.89042857754718));
#48170=CARTESIAN_POINT('Ctrl Pts',(366.977214835422,-7.94381860134222,-0.777600893731445));
#48171=CARTESIAN_POINT('Ctrl Pts',(366.956012399741,-7.93794446264189,-0.663759606355969));
#48172=CARTESIAN_POINT('Ctrl Pts',(366.93987810049,-7.93207032394156,-0.549388762467624));
#48173=CARTESIAN_POINT('Ctrl Pts',(366.935797999604,-7.93058485016024,-0.520466243165588));
#48174=CARTESIAN_POINT('Ctrl Pts',(366.932041746676,-7.92909937637892,-0.491509865734178));
#48175=CARTESIAN_POINT('Ctrl Pts',(366.928609550068,-7.9276139025976,-0.462527459354826));
#48176=CARTESIAN_POINT('Ctrl Pts',(366.910548798985,-7.91979710907673,-0.310017540125761));
#48177=CARTESIAN_POINT('Ctrl Pts',(366.901418401507,-7.91198031555585,-0.156429518548803));
#48178=CARTESIAN_POINT('Ctrl Pts',(366.901318679092,-7.90416352203497,-0.00254878017787867));
#48179=CARTESIAN_POINT('',(366.901318248747,-6.65416352207208,-0.00176385594813664));
#48180=CARTESIAN_POINT('Ctrl Pts',(366.901318679092,-7.90416352198934,-0.00254877927963419));
#48181=CARTESIAN_POINT('Ctrl Pts',(366.901244822297,-7.89837421657266,0.11141899917109));
#48182=CARTESIAN_POINT('Ctrl Pts',(366.90612887188,-7.89258491115597,0.225581876613283));
#48183=CARTESIAN_POINT('Ctrl Pts',(366.915995242575,-7.88679560573928,0.339465637256839));
#48184=CARTESIAN_POINT('Ctrl Pts',(366.92585045942,-7.88101284508428,0.453220653255002));
#48185=CARTESIAN_POINT('Ctrl Pts',(366.940676765202,-7.87523008442928,0.566696759134401));
#48186=CARTESIAN_POINT('Ctrl Pts',(366.960446549786,-7.86944732377427,0.679418960879135));
#48187=CARTESIAN_POINT('Ctrl Pts',(366.980439020439,-7.86359942633309,0.793410861024053));
#48188=CARTESIAN_POINT('Ctrl Pts',(367.005487042511,-7.85775152889191,0.906631326792071));
#48189=CARTESIAN_POINT('Ctrl Pts',(367.035507950599,-7.85190363145073,1.01859330633901));
#48190=CARTESIAN_POINT('Ctrl Pts',(367.06515506273,-7.84612854727743,1.12916122627897));
#48191=CARTESIAN_POINT('Ctrl Pts',(367.099651809084,-7.84035346310412,1.23850140015343));
#48192=CARTESIAN_POINT('Ctrl Pts',(367.138867230103,-7.83457837893082,1.3461551515598));
#48193=CARTESIAN_POINT('Ctrl Pts',(367.178074621549,-7.82880447723762,1.4537868602711));
#48194=CARTESIAN_POINT('Ctrl Pts',(367.221998622053,-7.82303057554442,1.55973243314473));
#48195=CARTESIAN_POINT('Ctrl Pts',(367.270458937297,-7.81725667385122,1.66355000747509));
#48196=CARTESIAN_POINT('Ctrl Pts',(367.318921802855,-7.81148246829584,1.76737304539593));
#48197=CARTESIAN_POINT('Ctrl Pts',(367.371921276813,-7.80570826274047,1.86906747704612));
#48198=CARTESIAN_POINT('Ctrl Pts',(367.429229990094,-7.79993405718509,1.96821382079431));
#48199=CARTESIAN_POINT('Ctrl Pts',(367.487817207028,-7.7940310345185,2.06957202649772));
#48200=CARTESIAN_POINT('Ctrl Pts',(367.55090799828,-7.7881280118519,2.16826669130543));
#48201=CARTESIAN_POINT('Ctrl Pts',(367.618212020707,-7.78222498918531,2.26387991599553));
#48202=CARTESIAN_POINT('Ctrl Pts',(367.684140814576,-7.77644258346037,2.35753946789875));
#48203=CARTESIAN_POINT('Ctrl Pts',(367.754111989783,-7.77066017773543,2.44824200439943));
#48204=CARTESIAN_POINT('Ctrl Pts',(367.827811982307,-7.76487777201049,2.53562841286821));
#48205=CARTESIAN_POINT('Ctrl Pts',(367.903817970326,-7.75891444087307,2.62574905043641));
#48206=CARTESIAN_POINT('Ctrl Pts',(367.98378961237,-7.75295110973564,2.71234227090173));
#48207=CARTESIAN_POINT('Ctrl Pts',(368.067343253147,-7.74698777859822,2.79505645068774));
#48208=CARTESIAN_POINT('Ctrl Pts',(368.150896893925,-7.7410244474608,2.87777063047374));
#48209=CARTESIAN_POINT('Ctrl Pts',(368.238032121945,-7.73506111632337,2.95660549728913));
#48210=CARTESIAN_POINT('Ctrl Pts',(368.328330781215,-7.72909778518595,3.03125680121685));
#48211=CARTESIAN_POINT('Ctrl Pts',(368.417272056605,-7.72322409579538,3.10478593481145));
#48212=CARTESIAN_POINT('Ctrl Pts',(368.509600375792,-7.71735040640482,3.17451972307166));
#48213=CARTESIAN_POINT('Ctrl Pts',(368.60495804359,-7.71147671701425,3.24013021948005));
#48214=CARTESIAN_POINT('Ctrl Pts',(368.70019259568,-7.70561061110848,3.30565600657383));
#48215=CARTESIAN_POINT('Ctrl Pts',(368.798448381085,-7.69974450520272,3.36706885657954));
#48216=CARTESIAN_POINT('Ctrl Pts',(368.899333887231,-7.69387839929696,3.42408032197673));
#48217=CARTESIAN_POINT('Ctrl Pts',(369.000116087903,-7.68801830020892,3.48103340835951));
#48218=CARTESIAN_POINT('Ctrl Pts',(369.103522295566,-7.68215820112089,3.53359387280054));
#48219=CARTESIAN_POINT('Ctrl Pts',(369.209131760855,-7.67629810203285,3.5815163220582));
#48220=CARTESIAN_POINT('Ctrl Pts',(369.318551374717,-7.67022658393875,3.63116770395649));
#48221=CARTESIAN_POINT('Ctrl Pts',(369.430335852678,-7.66415506584464,3.67583983813451));
#48222=CARTESIAN_POINT('Ctrl Pts',(369.543988661728,-7.65808354775054,3.71531150478304));
#48223=CARTESIAN_POINT('Ctrl Pts',(369.653557834519,-7.65223018415378,3.75336492290394));
#48224=CARTESIAN_POINT('Ctrl Pts',(369.764862964019,-7.64637682055703,3.78658500868895));
#48225=CARTESIAN_POINT('Ctrl Pts',(369.877439249627,-7.64052345696027,3.81482271383333));
#48226=CARTESIAN_POINT('Ctrl Pts',(369.989998632285,-7.63467097222637,3.84305617918127));
#48227=CARTESIAN_POINT('Ctrl Pts',(370.103828390928,-7.62881848749247,3.86630865087886));
#48228=CARTESIAN_POINT('Ctrl Pts',(370.218450323905,-7.62296600275858,3.88448145655638));
#48229=CARTESIAN_POINT('Ctrl Pts',(370.333082766174,-7.6171129814304,3.90265592843621));
#48230=CARTESIAN_POINT('Ctrl Pts',(370.44850711909,-7.61125996010222,3.91574974375619));
#48231=CARTESIAN_POINT('Ctrl Pts',(370.564237497149,-7.60540693877404,3.92371579007229));
#48232=CARTESIAN_POINT('Ctrl Pts',(370.680006473524,-7.59955196535024,3.93168449321864));
#48233=CARTESIAN_POINT('Ctrl Pts',(370.796081266048,-7.59369699192644,3.93452199832942));
#48234=CARTESIAN_POINT('Ctrl Pts',(370.911974120306,-7.58784201850264,3.93223327184222));
#48235=CARTESIAN_POINT('Ctrl Pts',(371.027998324229,-7.58198040921848,3.92994195137751));
#48236=CARTESIAN_POINT('Ctrl Pts',(371.143839765021,-7.57611879993433,3.92251281121623));
#48237=CARTESIAN_POINT('Ctrl Pts',(371.259013846276,-7.57025719065017,3.91000285338588));
#48238=CARTESIAN_POINT('Ctrl Pts',(371.374265590259,-7.56439162883983,3.89748445999912));
#48239=CARTESIAN_POINT('Ctrl Pts',(371.488848671303,-7.5585260670295,3.87987848954137));
#48240=CARTESIAN_POINT('Ctrl Pts',(371.602288461927,-7.55266050521916,3.85729311100003));
#48241=CARTESIAN_POINT('Ctrl Pts',(371.715894129348,-7.54678636651883,3.83467470709581));
#48242=CARTESIAN_POINT('Ctrl Pts',(371.82835277023,-7.5409122278185,3.80706246196675));
#48243=CARTESIAN_POINT('Ctrl Pts',(371.939204617298,-7.53503808911817,3.77461444899661));
#48244=CARTESIAN_POINT('Ctrl Pts',(371.967237239752,-7.53355261533688,3.76640887623419));
#48245=CARTESIAN_POINT('Ctrl Pts',(371.995167208274,-7.53206714155559,3.75789429531113));
#48246=CARTESIAN_POINT('Ctrl Pts',(372.022987303979,-7.5305816677743,3.74907374385212));
#48247=CARTESIAN_POINT('Ctrl Pts',(372.132990323247,-7.52470797838373,3.71419653485905));
#48248=CARTESIAN_POINT('Ctrl Pts',(372.241640232704,-7.51883428899316,3.67441567358135));
#48249=CARTESIAN_POINT('Ctrl Pts',(372.348467546356,-7.51296059960259,3.62985395116504));
#48250=CARTESIAN_POINT('Ctrl Pts',(372.45515693591,-7.50709449369683,3.58534976211875));
#48251=CARTESIAN_POINT('Ctrl Pts',(372.560028031468,-7.50122838779108,3.53607714469605));
#48252=CARTESIAN_POINT('Ctrl Pts',(372.662626205627,-7.49536228188532,3.48220871984077));
#48253=CARTESIAN_POINT('Ctrl Pts',(372.765119320562,-7.48950218279727,3.42839545556629));
#48254=CARTESIAN_POINT('Ctrl Pts',(372.865343779956,-7.48364208370923,3.36999593549378));
#48255=CARTESIAN_POINT('Ctrl Pts',(372.96286528571,-7.47778198462119,3.30723068860612));
#48256=CARTESIAN_POINT('Ctrl Pts',(373.063905144909,-7.47171046652708,3.24220101480127));
#48257=CARTESIAN_POINT('Ctrl Pts',(373.162042918496,-7.46563894843298,3.17248482958958));
#48258=CARTESIAN_POINT('Ctrl Pts',(373.256823538462,-7.45956743033887,3.09837944819387));
#48259=CARTESIAN_POINT('Ctrl Pts',(373.348198615005,-7.45371406674212,3.02693673237523));
#48260=CARTESIAN_POINT('Ctrl Pts',(373.436453283101,-7.44786070314537,2.95141508308361));
#48261=CARTESIAN_POINT('Ctrl Pts',(373.521210323463,-7.44200733954862,2.87212427540538));
#48262=CARTESIAN_POINT('Ctrl Pts',(373.605954637841,-7.43615485481471,2.79284537297504));
#48263=CARTESIAN_POINT('Ctrl Pts',(373.687202067072,-7.43030237008081,2.70979871960328));
#48264=CARTESIAN_POINT('Ctrl Pts',(373.764610458325,-7.4244498853469,2.62333266066084));
#48265=CARTESIAN_POINT('Ctrl Pts',(373.842025946888,-7.41859686401873,2.53685867394186));
#48266=CARTESIAN_POINT('Ctrl Pts',(373.915601422169,-7.41274384269055,2.44696496624825));
#48267=CARTESIAN_POINT('Ctrl Pts',(373.985033892059,-7.40689082136238,2.35403429087817));
#48268=CARTESIAN_POINT('Ctrl Pts',(374.054489519017,-7.40103584793857,2.26107262133317));
#48269=CARTESIAN_POINT('Ctrl Pts',(374.119799145844,-7.39518087451475,2.16507230082107));
#48270=CARTESIAN_POINT('Ctrl Pts',(374.180702529568,-7.38932590109093,2.06644588555593));
#48271=CARTESIAN_POINT('Ctrl Pts',(374.241674939455,-7.38346429180678,1.96770768991714));
#48272=CARTESIAN_POINT('Ctrl Pts',(374.298230921501,-7.37760268252263,1.86633781064785));
#48273=CARTESIAN_POINT('Ctrl Pts',(374.350155670638,-7.37174107323848,1.76277435925264));
#48274=CARTESIAN_POINT('Ctrl Pts',(374.402115433015,-7.36587551142814,1.65914107426153));
#48275=CARTESIAN_POINT('Ctrl Pts',(374.449437575916,-7.36000994961779,1.553311648068));
#48276=CARTESIAN_POINT('Ctrl Pts',(374.49195569452,-7.35414438780745,1.44574355330403));
#48277=CARTESIAN_POINT('Ctrl Pts',(374.534535985041,-7.34827024910712,1.33801816760284));
#48278=CARTESIAN_POINT('Ctrl Pts',(374.572298097598,-7.34239611040679,1.22854942847895));
#48279=CARTESIAN_POINT('Ctrl Pts',(374.605125618281,-7.33652197170647,1.11780937506639));
#48280=CARTESIAN_POINT('Ctrl Pts',(374.613427162348,-7.33503649792519,1.08980502340337));
#48281=CARTESIAN_POINT('Ctrl Pts',(374.621413394761,-7.33355102414392,1.06171941638111));
#48282=CARTESIAN_POINT('Ctrl Pts',(374.629082954632,-7.33206555036264,1.03356026681246));
#48283=CARTESIAN_POINT('Ctrl Pts',(374.659409045212,-7.32619186097207,0.922216599792636));
#48284=CARTESIAN_POINT('Ctrl Pts',(374.684881024598,-7.3203181715815,0.809351645022848));
#48285=CARTESIAN_POINT('Ctrl Pts',(374.705347562333,-7.31444448219092,0.695426481516768));
#48286=CARTESIAN_POINT('Ctrl Pts',(374.725787675845,-7.30857837628516,0.581648406099501));
#48287=CARTESIAN_POINT('Ctrl Pts',(374.741235127104,-7.30271227037939,0.466813247019476));
#48288=CARTESIAN_POINT('Ctrl Pts',(374.751588513005,-7.29684616447362,0.35139661070802));
#48289=CARTESIAN_POINT('Ctrl Pts',(374.761931297171,-7.29098606538559,0.236098159562184));
#48290=CARTESIAN_POINT('Ctrl Pts',(374.767190354854,-7.28512596629757,0.120219824582055));
#48291=CARTESIAN_POINT('Ctrl Pts',(374.76731556116,-7.27926586720954,0.00424610072738966));
#48292=CARTESIAN_POINT('Ctrl Pts',(374.767445284623,-7.27319434911543,-0.115911690505665));
#48293=CARTESIAN_POINT('Ctrl Pts',(374.762063647564,-7.26712283102132,-0.236171438832659));
#48294=CARTESIAN_POINT('Ctrl Pts',(374.751173789599,-7.26105131292722,-0.355989569624242));
#48295=CARTESIAN_POINT('Ctrl Pts',(374.740675212935,-7.25519794933046,-0.471502539220447));
#48296=CARTESIAN_POINT('Ctrl Pts',(374.725057473366,-7.2493445857337,-0.586604633741704));
#48297=CARTESIAN_POINT('Ctrl Pts',(374.704376383168,-7.24349122213694,-0.700810940842099));
#48298=CARTESIAN_POINT('Ctrl Pts',(374.683698398167,-7.23763873740303,-0.815000100249708));
#48299=CARTESIAN_POINT('Ctrl Pts',(374.657958647785,-7.23178625266912,-0.928293333247853));
#48300=CARTESIAN_POINT('Ctrl Pts',(374.627264365069,-7.22593376793521,-1.04021428478964));
#48301=CARTESIAN_POINT('Ctrl Pts',(374.5965672681,-7.22008074660703,-1.15214549797992));
#48302=CARTESIAN_POINT('Ctrl Pts',(374.560914845037,-7.21422772527886,-1.26270378114107));
#48303=CARTESIAN_POINT('Ctrl Pts',(374.520464471577,-7.20837470395068,-1.37142703342242));
#48304=CARTESIAN_POINT('Ctrl Pts',(374.480000607137,-7.20251973052685,-1.48018654700817));
#48305=CARTESIAN_POINT('Ctrl Pts',(374.434735754339,-7.19666475710302,-1.5871094257381));
#48306=CARTESIAN_POINT('Ctrl Pts',(374.384875507219,-7.19080978367919,-1.69175333475488));
#48307=CARTESIAN_POINT('Ctrl Pts',(374.334958749914,-7.18494817439503,-1.79651584420155));
#48308=CARTESIAN_POINT('Ctrl Pts',(374.280436380666,-7.17908656511086,-1.89899385540377));
#48309=CARTESIAN_POINT('Ctrl Pts',(374.221560100138,-7.1732249558267,-1.998769361562));
#48310=CARTESIAN_POINT('Ctrl Pts',(374.162644118903,-7.16735939401636,-2.09861214707661));
#48311=CARTESIAN_POINT('Ctrl Pts',(374.099368605355,-7.16149383220602,-2.1957484535869));
#48312=CARTESIAN_POINT('Ctrl Pts',(374.032027767701,-7.15562827039568,-2.28979044955066));
#48313=CARTESIAN_POINT('Ctrl Pts',(373.964588461226,-7.14975413169534,-2.38396995797791));
#48314=CARTESIAN_POINT('Ctrl Pts',(373.893072221089,-7.143879992995,-2.47504580212331));
#48315=CARTESIAN_POINT('Ctrl Pts',(373.817812596392,-7.13800585429467,-2.56266426156235));
#48316=CARTESIAN_POINT('Ctrl Pts',(373.798780665929,-7.13652038051344,-2.58482153957156));
#48317=CARTESIAN_POINT('Ctrl Pts',(373.779509522504,-7.13503490673222,-2.60675790802626));
#48318=CARTESIAN_POINT('Ctrl Pts',(373.760004909503,-7.13354943295099,-2.62846804217276));
#48319=CARTESIAN_POINT('Ctrl Pts',(373.682882014504,-7.12767574356043,-2.71431175494352));
#48320=CARTESIAN_POINT('Ctrl Pts',(373.601849309627,-7.12180205416987,-2.79690122454613));
#48321=CARTESIAN_POINT('Ctrl Pts',(373.517212205502,-7.11592836477931,-2.87585933148935));
#48322=CARTESIAN_POINT('Ctrl Pts',(373.43268437583,-7.11006225887357,-2.95471549609863));
#48323=CARTESIAN_POINT('Ctrl Pts',(373.344561700769,-7.10419615296782,-3.02994934254657));
#48324=CARTESIAN_POINT('Ctrl Pts',(373.253188864547,-7.09833004706208,-3.10121783023713));
#48325=CARTESIAN_POINT('Ctrl Pts',(373.161909592945,-7.09246994797402,-3.17241333990454));
#48326=CARTESIAN_POINT('Ctrl Pts',(373.067387103929,-7.08660984888597,-3.2396513148576));
#48327=CARTESIAN_POINT('Ctrl Pts',(372.970001349233,-7.08074974979792,-3.30262698542776));
#48328=CARTESIAN_POINT('Ctrl Pts',(372.86910213868,-7.07467823170381,-3.36787467452141));
#48329=CARTESIAN_POINT('Ctrl Pts',(372.765129491823,-7.0686067136097,-3.4285463960289));
#48330=CARTESIAN_POINT('Ctrl Pts',(372.658541880706,-7.0625351955156,-3.48435011122001));
#48331=CARTESIAN_POINT('Ctrl Pts',(372.555784047638,-7.05668183191886,-3.53814875432692));
#48332=CARTESIAN_POINT('Ctrl Pts',(372.450596329222,-7.05082846832213,-3.58742298538895));
#48333=CARTESIAN_POINT('Ctrl Pts',(372.343416457472,-7.0449751047254,-3.63195682830301));
#48334=CARTESIAN_POINT('Ctrl Pts',(372.236252678418,-7.0391226199915,-3.67648398461054));
#48335=CARTESIAN_POINT('Ctrl Pts',(372.127097722202,-7.03327013525759,-3.71627200952119));
#48336=CARTESIAN_POINT('Ctrl Pts',(372.016410005761,-7.02741765052369,-3.75115277520263));
#48337=CARTESIAN_POINT('Ctrl Pts',(371.905712140743,-7.02156462919553,-3.7860367389819));
#48338=CARTESIAN_POINT('Ctrl Pts',(371.793481630196,-7.01571160786736,-3.81601242493306));
#48339=CARTESIAN_POINT('Ctrl Pts',(371.680192095955,-7.0098585865392,-3.8409615678219));
#48340=CARTESIAN_POINT('Ctrl Pts',(371.566864777465,-7.00400361311539,-3.86591903173173));
#48341=CARTESIAN_POINT('Ctrl Pts',(371.452478136207,-6.99814863969157,-3.88584653022729));
#48342=CARTESIAN_POINT('Ctrl Pts',(371.337515324113,-6.99229366626776,-3.90067703165623));
#48343=CARTESIAN_POINT('Ctrl Pts',(371.222422216439,-6.98643205698361,-3.91552434155363));
#48344=CARTESIAN_POINT('Ctrl Pts',(371.106752044528,-6.98057044769946,-3.92526307136814));
#48345=CARTESIAN_POINT('Ctrl Pts',(370.990992512098,-6.97470883841532,-3.92987812168097));
#48346=CARTESIAN_POINT('Ctrl Pts',(370.875154922165,-6.968843276605,-3.93449628395611));
#48347=CARTESIAN_POINT('Ctrl Pts',(370.759228263849,-6.96297771479469,-3.93398388900972));
#48348=CARTESIAN_POINT('Ctrl Pts',(370.643697928103,-6.95711215298438,-3.92837791513835));
#48349=CARTESIAN_POINT('Ctrl Pts',(370.52799865867,-6.95123801428405,-3.9227637439582));
#48350=CARTESIAN_POINT('Ctrl Pts',(370.412697278174,-6.94536387558372,-3.91204116750302));
#48351=CARTESIAN_POINT('Ctrl Pts',(370.298271840804,-6.9394897368834,-3.89629871449412));
#48352=CARTESIAN_POINT('Ctrl Pts',(370.269335515701,-6.93800426310204,-3.89231770512544));
#48353=CARTESIAN_POINT('Ctrl Pts',(370.240455143008,-6.93651878932069,-3.88801592605633));
#48354=CARTESIAN_POINT('Ctrl Pts',(370.211638310701,-6.93503331553933,-3.8833953169004));
#48355=CARTESIAN_POINT('Ctrl Pts',(370.097694110331,-6.92915962614875,-3.86512503618736));
#48356=CARTESIAN_POINT('Ctrl Pts',(369.984364930911,-6.92328593675816,-3.84180515537915));
#48357=CARTESIAN_POINT('Ctrl Pts',(369.872133234915,-6.91741224736758,-3.81348787336344));
#48358=CARTESIAN_POINT('Ctrl Pts',(369.760046440583,-6.91154614146182,-3.78520715161916));
#48359=CARTESIAN_POINT('Ctrl Pts',(369.649054708751,-6.90568003555606,-3.75194195995776));
#48360=CARTESIAN_POINT('Ctrl Pts',(369.539633155722,-6.8998139296503,-3.71379597367104));
#48361=CARTESIAN_POINT('Ctrl Pts',(369.430323648969,-6.89395383056222,-3.67568904838807));
#48362=CARTESIAN_POINT('Ctrl Pts',(369.322581510686,-6.88809373147414,-3.63271140485318));
#48363=CARTESIAN_POINT('Ctrl Pts',(369.216868816665,-6.88223363238606,-3.58501710095414));
#48364=CARTESIAN_POINT('Ctrl Pts',(369.107342249814,-6.87616211429196,-3.53560209537897));
#48365=CARTESIAN_POINT('Ctrl Pts',(368.999994765382,-6.87009059619786,-3.48112378160884));
#48366=CARTESIAN_POINT('Ctrl Pts',(368.895320307861,-6.86401907810376,-3.4218091003266));
#48367=CARTESIAN_POINT('Ctrl Pts',(368.794406887253,-6.858165714507,-3.36462564294582));
#48368=CARTESIAN_POINT('Ctrl Pts',(368.695978101632,-6.85231235091025,-3.30294760703743));
#48369=CARTESIAN_POINT('Ctrl Pts',(368.6004527361,-6.84645898731349,-3.23702573954811));
#48370=CARTESIAN_POINT('Ctrl Pts',(368.50494171338,-6.84060650257958,-3.17111377000538));
#48371=CARTESIAN_POINT('Ctrl Pts',(368.412333583885,-6.83475401784568,-3.10095947046379));
#48372=CARTESIAN_POINT('Ctrl Pts',(368.323018138932,-6.82890153311177,-3.02685690857625));
#48373=CARTESIAN_POINT('Ctrl Pts',(368.233694504952,-6.82304851178359,-2.95274755247875));
#48374=CARTESIAN_POINT('Ctrl Pts',(368.147664473629,-6.81719549045541,-2.87468947822377));
#48375=CARTESIAN_POINT('Ctrl Pts',(368.065284179068,-6.81134246912724,-2.79301656124543));
#48376=CARTESIAN_POINT('Ctrl Pts',(367.982876409087,-6.80548749570336,-2.71131640477127));
#48377=CARTESIAN_POINT('Ctrl Pts',(367.904121089567,-6.79963252227948,-2.62599929897062));
#48378=CARTESIAN_POINT('Ctrl Pts',(367.82933646899,-6.79377754885561,-2.53743490170824));
#48379=CARTESIAN_POINT('Ctrl Pts',(367.754467089651,-6.78791593957144,-2.44877012807792));
#48380=CARTESIAN_POINT('Ctrl Pts',(367.683577658234,-6.78205433028728,-2.35685103299066));
#48381=CARTESIAN_POINT('Ctrl Pts',(367.61694525172,-6.77619272100311,-2.26207925216892));
#48382=CARTESIAN_POINT('Ctrl Pts',(367.550267914486,-6.77032715919274,-2.16724356603906));
#48383=CARTESIAN_POINT('Ctrl Pts',(367.487853539927,-6.76446159738237,-2.06955171118032));
#48384=CARTESIAN_POINT('Ctrl Pts',(367.429934189944,-6.758596035572,-1.96943161170743));
#48385=CARTESIAN_POINT('Ctrl Pts',(367.371930147666,-6.75272189687167,-1.86916511209358));
#48386=CARTESIAN_POINT('Ctrl Pts',(367.318434437805,-6.74684775817134,-1.76646364659021));
#48387=CARTESIAN_POINT('Ctrl Pts',(367.269631826703,-6.74097361947101,-1.66177692014548));
#48388=CARTESIAN_POINT('Ctrl Pts',(367.257290443066,-6.7394881456899,-1.63530335605419));
#48389=CARTESIAN_POINT('Ctrl Pts',(367.245248937058,-6.73800267190878,-1.6087029169066));
#48390=CARTESIAN_POINT('Ctrl Pts',(367.233509792322,-6.73651719812767,-1.58198303042237));
#48391=CARTESIAN_POINT('Ctrl Pts',(367.182386656801,-6.73004806607979,-1.46561983628958));
#48392=CARTESIAN_POINT('Ctrl Pts',(367.136855419181,-6.7235789340319,-1.34665702101869));
#48393=CARTESIAN_POINT('Ctrl Pts',(367.097161857521,-6.71710980198402,-1.22562394876207));
#48394=CARTESIAN_POINT('Ctrl Pts',(367.05762730515,-6.71066658477084,-1.10507572548325));
#48395=CARTESIAN_POINT('Ctrl Pts',(367.023883885696,-6.70422336755765,-0.982474039744795));
#48396=CARTESIAN_POINT('Ctrl Pts',(366.996128507445,-6.69778015034447,-0.858365624862619));
#48397=CARTESIAN_POINT('Ctrl Pts',(366.968446864221,-6.69135405020284,-0.734586916794222));
#48398=CARTESIAN_POINT('Ctrl Pts',(366.946721618277,-6.68492795006121,-0.609309720773344));
#48399=CARTESIAN_POINT('Ctrl Pts',(366.93110035336,-6.67850184991958,-0.483096417658677));
#48400=CARTESIAN_POINT('Ctrl Pts',(366.915541521388,-6.67210143274021,-0.357387546692535));
#48401=CARTESIAN_POINT('Ctrl Pts',(366.906038079496,-6.66570101556084,-0.23075029565414));
#48402=CARTESIAN_POINT('Ctrl Pts',(366.902686689438,-6.65930059838148,-0.103756406788144));
#48403=CARTESIAN_POINT('Ctrl Pts',(366.901790063172,-6.65758823961168,-0.0697806372068197));
#48404=CARTESIAN_POINT('Ctrl Pts',(366.901333503911,-6.65587588084188,-0.0357794177768005));
#48405=CARTESIAN_POINT('Ctrl Pts',(366.901318248747,-6.65416352207208,-0.00176385594814673));
#48406=CARTESIAN_POINT('',(366.901319367511,-5.40416352200791,0.00345128679816103));
#48407=CARTESIAN_POINT('Ctrl Pts',(366.901318248747,-6.65416352203497,-0.00176385521094843));
#48408=CARTESIAN_POINT('Ctrl Pts',(366.901265199377,-6.64820884358741,0.116524284211845));
#48409=CARTESIAN_POINT('Ctrl Pts',(366.906552916805,-6.64225416513986,0.234793871859763));
#48410=CARTESIAN_POINT('Ctrl Pts',(366.917149970721,-6.6362994866923,0.352540466170501));
#48411=CARTESIAN_POINT('Ctrl Pts',(366.927751320045,-6.63034239457625,0.470334787868657));
#48412=CARTESIAN_POINT('Ctrl Pts',(366.943666256189,-6.6243853024602,0.587605302905504));
#48413=CARTESIAN_POINT('Ctrl Pts',(366.964811579099,-6.61842821034415,0.703853816146331));
#48414=CARTESIAN_POINT('Ctrl Pts',(366.98596984317,-6.61246747242437,0.820173474713461));
#48415=CARTESIAN_POINT('Ctrl Pts',(367.012364798096,-6.6065067345046,0.935469499932208));
#48416=CARTESIAN_POINT('Ctrl Pts',(367.043862465922,-6.60054599658482,1.04925542975754));
#48417=CARTESIAN_POINT('Ctrl Pts',(367.075408021142,-6.59457619627333,1.16321435371244));
#48418=CARTESIAN_POINT('Ctrl Pts',(367.112071678325,-6.58860639596184,1.27565821811409));
#48419=CARTESIAN_POINT('Ctrl Pts',(367.153669865202,-6.58263659565035,1.38611665752539));
#48420=CARTESIAN_POINT('Ctrl Pts',(367.195303399591,-6.57666172257948,1.49666895754418));
#48421=CARTESIAN_POINT('Ctrl Pts',(367.241879665614,-6.57068684950862,1.6052321101754));
#48422=CARTESIAN_POINT('Ctrl Pts',(367.293168055001,-6.56471197643775,1.71135826364399));
#48423=CARTESIAN_POINT('Ctrl Pts',(367.344548369054,-6.55872639454521,1.81767462802412));
#48424=CARTESIAN_POINT('Ctrl Pts',(367.400657490594,-6.55274081265266,1.92154492330828));
#48425=CARTESIAN_POINT('Ctrl Pts',(367.461219925966,-6.54675523076011,2.02254774310239));
#48426=CARTESIAN_POINT('Ctrl Pts',(367.490744910938,-6.54383718074542,2.07178794816112));
#48427=CARTESIAN_POINT('Ctrl Pts',(367.521327673345,-6.54091913073072,2.12034710914281));
#48428=CARTESIAN_POINT('Ctrl Pts',(367.552932801484,-6.53800108071602,2.16817922280896));
#48429=CARTESIAN_POINT('Ctrl Pts',(367.616550184635,-6.53212739132544,2.26445960770791));
#48430=CARTESIAN_POINT('Ctrl Pts',(367.684514613203,-6.52625370193487,2.35809804104892));
#48431=CARTESIAN_POINT('Ctrl Pts',(367.756579642237,-6.5203800125443,2.44867648018891));
#48432=CARTESIAN_POINT('Ctrl Pts',(367.828551628548,-6.51451390663854,2.53913797405444));
#48433=CARTESIAN_POINT('Ctrl Pts',(367.904613431905,-6.50864780073278,2.6265470100949));
#48434=CARTESIAN_POINT('Ctrl Pts',(367.984474736695,-6.50278169482702,2.71051345895475));
#48435=CARTESIAN_POINT('Ctrl Pts',(368.064254264528,-6.49692159573898,2.79439392724059));
#48436=CARTESIAN_POINT('Ctrl Pts',(368.147825271951,-6.49106149665095,2.87483852260736));
#48437=CARTESIAN_POINT('Ctrl Pts',(368.234856916643,-6.48520139756291,2.9514897660653));
#48438=CARTESIAN_POINT('Ctrl Pts',(368.325028464524,-6.4791298794688,3.0309064115177));
#48439=CARTESIAN_POINT('Ctrl Pts',(368.418914786781,-6.4730583613747,3.10625047285123));
#48440=CARTESIAN_POINT('Ctrl Pts',(368.516105501817,-6.46698684328059,3.1771654810199));
#48441=CARTESIAN_POINT('Ctrl Pts',(368.60980407679,-6.46113347968384,3.24553245627129));
#48442=CARTESIAN_POINT('Ctrl Pts',(368.706573309863,-6.45528011608708,3.30978291527893));
#48443=CARTESIAN_POINT('Ctrl Pts',(368.806012113383,-6.44942675249033,3.36963867880944));
#48444=CARTESIAN_POINT('Ctrl Pts',(368.905435986501,-6.44357426775642,3.42948545519847));
#48445=CARTESIAN_POINT('Ctrl Pts',(369.007528279199,-6.43772178302251,3.4849386351298));
#48446=CARTESIAN_POINT('Ctrl Pts',(369.11186038753,-6.4318692982886,3.53576431325329));
#48447=CARTESIAN_POINT('Ctrl Pts',(369.216202061715,-6.42601627696041,3.58659465140923));
#48448=CARTESIAN_POINT('Ctrl Pts',(369.322783588333,-6.42016325563221,3.63279646338199));
#48449=CARTESIAN_POINT('Ctrl Pts',(369.431153970121,-6.41431023430401,3.67418291830369));
#48450=CARTESIAN_POINT('Ctrl Pts',(369.539560495523,-6.40845526088018,3.71558317640724));
#48451=CARTESIAN_POINT('Ctrl Pts',(369.649756676694,-6.40260028745635,3.75216473665459));
#48452=CARTESIAN_POINT('Ctrl Pts',(369.761274533554,-6.39674531403253,3.78379003568001));
#48453=CARTESIAN_POINT('Ctrl Pts',(369.872918781581,-6.39088370474837,3.81545117791975));
#48454=CARTESIAN_POINT('Ctrl Pts',(369.985887297422,-6.38502209546421,3.84214473439232));
#48455=CARTESIAN_POINT('Ctrl Pts',(370.099699938997,-6.37916048618005,3.86378383454573));
#48456=CARTESIAN_POINT('Ctrl Pts',(370.213589325272,-6.37329492436972,3.88543752610323));
#48457=CARTESIAN_POINT('Ctrl Pts',(370.328323562807,-6.36742936255939,3.90202991575999));
#48458=CARTESIAN_POINT('Ctrl Pts',(370.443417115525,-6.36156380074906,3.91352598218878));
#48459=CARTESIAN_POINT('Ctrl Pts',(370.558678963247,-6.35568966204872,3.92503885868632));
#48460=CARTESIAN_POINT('Ctrl Pts',(370.674300763805,-6.34981552334837,3.93144051673659));
#48461=CARTESIAN_POINT('Ctrl Pts',(370.789796633956,-6.34394138464803,3.93274800375448));
#48462=CARTESIAN_POINT('Ctrl Pts',(370.819003654031,-6.34245591086681,3.93307864587641));
#48463=CARTESIAN_POINT('Ctrl Pts',(370.848202647226,-6.34097043708558,3.93308377387877));
#48464=CARTESIAN_POINT('Ctrl Pts',(370.877385822468,-6.33948496330436,3.93276418693331));
#48465=CARTESIAN_POINT('Ctrl Pts',(370.992778573902,-6.3336112739138,3.9315005130303));
#48466=CARTESIAN_POINT('Ctrl Pts',(371.108307847375,-6.32773758452324,3.92515175568437));
#48467=CARTESIAN_POINT('Ctrl Pts',(371.223488758222,-6.32186389513268,3.91369837962805));
#48468=CARTESIAN_POINT('Ctrl Pts',(371.338520959692,-6.31599778922692,3.90225979095622));
#48469=CARTESIAN_POINT('Ctrl Pts',(371.453205285617,-6.31013168332117,3.88572973050911));
#48470=CARTESIAN_POINT('Ctrl Pts',(371.567056524385,-6.30426557741542,3.8641406599379));
#48471=CARTESIAN_POINT('Ctrl Pts',(371.680791180934,-6.29840547832738,3.84257369629991));
#48472=CARTESIAN_POINT('Ctrl Pts',(371.793694043655,-6.29254537923935,3.81595810322062));
#48473=CARTESIAN_POINT('Ctrl Pts',(371.905285367377,-6.28668528015131,3.78437809734029));
#48474=CARTESIAN_POINT('Ctrl Pts',(372.020902651478,-6.2806137620572,3.75165875689333));
#48475=CARTESIAN_POINT('Ctrl Pts',(372.135111525706,-6.27454224396309,3.71361007580274));
#48476=CARTESIAN_POINT('Ctrl Pts',(372.247389974558,-6.26847072586898,3.67038365568356));
#48477=CARTESIAN_POINT('Ctrl Pts',(372.355634169012,-6.26261736227224,3.62871039538504));
#48478=CARTESIAN_POINT('Ctrl Pts',(372.462083855524,-6.2567639986755,3.58222523437998));
#48479=CARTESIAN_POINT('Ctrl Pts',(372.56628784447,-6.25091063507876,3.53111440616437));
#48480=CARTESIAN_POINT('Ctrl Pts',(372.670476187538,-6.24505815034487,3.48001125206761));
#48481=CARTESIAN_POINT('Ctrl Pts',(372.772419132659,-6.23920566561097,3.42428399363079));
#48482=CARTESIAN_POINT('Ctrl Pts',(372.871687777056,-6.23335318087708,3.36416598779938));
#48483=CARTESIAN_POINT('Ctrl Pts',(372.970965523054,-6.2275001595489,3.30404246995386));
#48484=CARTESIAN_POINT('Ctrl Pts',(373.067568127487,-6.22164713822072,3.23952761846589));
#48485=CARTESIAN_POINT('Ctrl Pts',(373.161094105004,-6.21579411689254,3.17089912708544));
#48486=CARTESIAN_POINT('Ctrl Pts',(373.254651275241,-6.20993914346874,3.1022477467781));
#48487=CARTESIAN_POINT('Ctrl Pts',(373.345129445268,-6.20408417004494,3.02948024274663));
#48488=CARTESIAN_POINT('Ctrl Pts',(373.432159323061,-6.19822919662114,2.95291528791417));
#48489=CARTESIAN_POINT('Ctrl Pts',(373.519287838041,-6.19236758733699,2.87626355653956));
#48490=CARTESIAN_POINT('Ctrl Pts',(373.602959949896,-6.18650597805284,2.79580605703823));
#48491=CARTESIAN_POINT('Ctrl Pts',(373.682842371033,-6.18064436876869,2.71189916321427));
#48492=CARTESIAN_POINT('Ctrl Pts',(373.762778657472,-6.17477880695837,2.62793569035573));
#48493=CARTESIAN_POINT('Ctrl Pts',(373.838919894111,-6.16891324514804,2.54051850245589));
#48494=CARTESIAN_POINT('Ctrl Pts',(373.910973438527,-6.16304768333771,2.45003661389421));
#48495=CARTESIAN_POINT('Ctrl Pts',(373.983132342898,-6.15717354463739,2.35942241861927));
#48496=CARTESIAN_POINT('Ctrl Pts',(374.051191384155,-6.15129940593707,2.2657349120178));
#48497=CARTESIAN_POINT('Ctrl Pts',(374.114901485447,-6.14542526723675,2.16939162715907));
#48498=CARTESIAN_POINT('Ctrl Pts',(374.13101272999,-6.1439397934554,2.14502798323304));
#48499=CARTESIAN_POINT('Ctrl Pts',(374.146846091015,-6.14245431967405,2.12049462005751));
#48500=CARTESIAN_POINT('Ctrl Pts',(374.162398016458,-6.1409688458927,2.09579851777101));
#48501=CARTESIAN_POINT('Ctrl Pts',(374.223891649414,-6.13509515650213,1.99814803358881));
#48502=CARTESIAN_POINT('Ctrl Pts',(374.281186256746,-6.12922146711156,1.89762615676717));
#48503=CARTESIAN_POINT('Ctrl Pts',(374.334002562226,-6.12334777772098,1.7946297494406));
#48504=CARTESIAN_POINT('Ctrl Pts',(374.386750676894,-6.11748167181523,1.69176632015215));
#48505=CARTESIAN_POINT('Ctrl Pts',(374.435031801233,-6.11161556590948,1.58643507813995));
#48506=CARTESIAN_POINT('Ctrl Pts',(374.478610175194,-6.10574946000373,1.47906134829925));
#48507=CARTESIAN_POINT('Ctrl Pts',(374.522143925455,-6.09988936091568,1.37179756778974));
#48508=CARTESIAN_POINT('Ctrl Pts',(374.560984349434,-6.09402926182763,1.26249584012391));
#48509=CARTESIAN_POINT('Ctrl Pts',(374.594942140613,-6.08816916273959,1.1516049535749));
#48510=CARTESIAN_POINT('Ctrl Pts',(374.630125051428,-6.08209764464548,1.03671337682208));
#48511=CARTESIAN_POINT('Ctrl Pts',(374.660066163093,-6.07602612655137,0.920116211687519));
#48512=CARTESIAN_POINT('Ctrl Pts',(374.684609878064,-6.06995460845727,0.802334296571989));
#48513=CARTESIAN_POINT('Ctrl Pts',(374.708271717741,-6.06410124486051,0.688784379795269));
#48514=CARTESIAN_POINT('Ctrl Pts',(374.726917259672,-6.05824788126375,0.574133824984173));
#48515=CARTESIAN_POINT('Ctrl Pts',(374.740458403138,-6.05239451766698,0.458862729270992));
#48516=CARTESIAN_POINT('Ctrl Pts',(374.753997513447,-6.04654203293307,0.34360894112484));
#48517=CARTESIAN_POINT('Ctrl Pts',(374.76243370101,-6.04068954819915,0.227735207551089));
#48518=CARTESIAN_POINT('Ctrl Pts',(374.765730545224,-6.03483706346523,0.111728443939046));
#48519=CARTESIAN_POINT('Ctrl Pts',(374.769027691713,-6.02898404213703,-0.00428895593571747));
#48520=CARTESIAN_POINT('Ctrl Pts',(374.767184546398,-6.02313102080884,-0.12043899709449));
#48521=CARTESIAN_POINT('Ctrl Pts',(374.760216808488,-6.01727799948065,-0.236233767823389));
#48522=CARTESIAN_POINT('Ctrl Pts',(374.753246746702,-6.01142302605686,-0.352067158343562));
#48523=CARTESIAN_POINT('Ctrl Pts',(374.741148718553,-6.00556805263307,-0.467544630646261));
#48524=CARTESIAN_POINT('Ctrl Pts',(374.72399031068,-5.99971307920928,-0.582183110120685));
#48525=CARTESIAN_POINT('Ctrl Pts',(374.706812455955,-5.99385146992511,-0.696951517587674));
#48526=CARTESIAN_POINT('Ctrl Pts',(374.6845628354,-5.98798986064094,-0.81087862548388));
#48527=CARTESIAN_POINT('Ctrl Pts',(374.657360234345,-5.98212825135678,-0.923491175999978));
#48528=CARTESIAN_POINT('Ctrl Pts',(374.630139290377,-5.97626268954643,-1.0361796619859));
#48529=CARTESIAN_POINT('Ctrl Pts',(374.597958829966,-5.97039712773607,-1.1475514296155));
#48530=CARTESIAN_POINT('Ctrl Pts',(374.560987100707,-5.96453156592572,-1.25714968077147));
#48531=CARTESIAN_POINT('Ctrl Pts',(374.523961309712,-5.95865742722538,-1.36690819145139));
#48532=CARTESIAN_POINT('Ctrl Pts',(374.482130416306,-5.95278328852503,-1.47488762628487));
#48533=CARTESIAN_POINT('Ctrl Pts',(374.435710249871,-5.94690914982468,-1.58065233539077));
#48534=CARTESIAN_POINT('Ctrl Pts',(374.423971347595,-5.94542367604347,-1.60739850370051));
#48535=CARTESIAN_POINT('Ctrl Pts',(374.411939185604,-5.94393820226226,-1.63400317072937));
#48536=CARTESIAN_POINT('Ctrl Pts',(374.399617703755,-5.94245272848105,-1.66045956765013));
#48537=CARTESIAN_POINT('Ctrl Pts',(374.350897518906,-5.9365790390905,-1.76507040620627));
#48538=CARTESIAN_POINT('Ctrl Pts',(374.297488148562,-5.93070534969995,-1.86770937983888));
#48539=CARTESIAN_POINT('Ctrl Pts',(374.239571680788,-5.92483166030939,-1.9679266678051));
#48540=CARTESIAN_POINT('Ctrl Pts',(374.181729988616,-5.91896555440365,-2.06801456583772));
#48541=CARTESIAN_POINT('Ctrl Pts',(374.119392976104,-5.9130994484979,-2.16568664159294));
#48542=CARTESIAN_POINT('Ctrl Pts',(374.052790239333,-5.90723334259215,-2.26051421137998));
#48543=CARTESIAN_POINT('Ctrl Pts',(373.986255702917,-5.90137324350412,-2.35524467894349));
#48544=CARTESIAN_POINT('Ctrl Pts',(373.915464366697,-5.89551314441609,-2.44713609813846));
#48545=CARTESIAN_POINT('Ctrl Pts',(373.840690726118,-5.88965304532807,-2.53578610082256));
#48546=CARTESIAN_POINT('Ctrl Pts',(373.763219423173,-5.88358152723396,-2.62763439336071));
#48547=CARTESIAN_POINT('Ctrl Pts',(373.681473271752,-5.87751000913985,-2.71600257662247));
#48548=CARTESIAN_POINT('Ctrl Pts',(373.595805585543,-5.87143849104573,-2.80047754932134));
#48549=CARTESIAN_POINT('Ctrl Pts',(373.513216007763,-5.86558512744899,-2.88191726874028));
#48550=CARTESIAN_POINT('Ctrl Pts',(373.426982172488,-5.85973176385225,-2.95973842014589));
#48551=CARTESIAN_POINT('Ctrl Pts',(373.337459748868,-5.8538784002555,-3.03360670659094));
#48552=CARTESIAN_POINT('Ctrl Pts',(373.247950766738,-5.84802591552162,-3.10746390196119));
#48553=CARTESIAN_POINT('Ctrl Pts',(373.155154496646,-5.84217343078773,-3.17736914961662));
#48554=CARTESIAN_POINT('Ctrl Pts',(373.059460353459,-5.83632094605385,-3.24302788357548));
#48555=CARTESIAN_POINT('Ctrl Pts',(372.963757436404,-5.83046792472569,-3.30869263755875));
#48556=CARTESIAN_POINT('Ctrl Pts',(372.86515645876,-5.82461490339752,-3.37010987010284));
#48557=CARTESIAN_POINT('Ctrl Pts',(372.76407592726,-5.81876188206936,-3.42702827179645));
#48558=CARTESIAN_POINT('Ctrl Pts',(372.662961683451,-5.81290690864556,-3.48396565687613));
#48559=CARTESIAN_POINT('Ctrl Pts',(372.559366601176,-5.80705193522176,-3.53640102493));
#48560=CARTESIAN_POINT('Ctrl Pts',(372.45373325118,-5.80119696179795,-3.58412929019914));
#48561=CARTESIAN_POINT('Ctrl Pts',(372.347980179349,-5.79533535251381,-3.63191164932661));
#48562=CARTESIAN_POINT('Ctrl Pts',(372.240184605656,-5.78947374322966,-3.6749760873295));
#48563=CARTESIAN_POINT('Ctrl Pts',(372.130808607008,-5.78361213394551,-3.71316586289273));
#48564=CARTESIAN_POINT('Ctrl Pts',(372.021358855321,-5.77774657213518,-3.75138139010204));
#48565=CARTESIAN_POINT('Ctrl Pts',(371.910326951368,-5.77188101032485,-3.78471559118148));
#48566=CARTESIAN_POINT('Ctrl Pts',(371.798187954813,-5.76601544851453,-3.81306221130252));
#48567=CARTESIAN_POINT('Ctrl Pts',(371.685884983541,-5.76014130981421,-3.84145028113463));
#48568=CARTESIAN_POINT('Ctrl Pts',(371.572472091944,-5.7542671711139,-3.86483613176591));
#48569=CARTESIAN_POINT('Ctrl Pts',(371.458432363199,-5.74839303241358,-3.88316495637757));
#48570=CARTESIAN_POINT('Ctrl Pts',(371.429593577509,-5.74690755863219,-3.88780001690193));
#48571=CARTESIAN_POINT('Ctrl Pts',(371.400714717576,-5.74542208485079,-3.89211193979637));
#48572=CARTESIAN_POINT('Ctrl Pts',(371.371803607131,-5.74393661106939,-3.89610036630818));
#48573=CARTESIAN_POINT('Ctrl Pts',(371.257486623005,-5.73806292167884,-3.91187094319804));
#48574=CARTESIAN_POINT('Ctrl Pts',(371.142284560392,-5.73218923228829,-3.9226321939895));
#48575=CARTESIAN_POINT('Ctrl Pts',(371.026674118864,-5.72631554289773,-3.92829327661122));
#48576=CARTESIAN_POINT('Ctrl Pts',(370.911212941278,-5.720449436992,-3.93394705024344));
#48577=CARTESIAN_POINT('Ctrl Pts',(370.795344842198,-5.71458333108627,-3.93451373068496));
#48578=CARTESIAN_POINT('Ctrl Pts',(370.679554514112,-5.70871722518053,-3.92995385581905));
#48579=CARTESIAN_POINT('Ctrl Pts',(370.563882753847,-5.70285712609249,-3.92539865020689));
#48580=CARTESIAN_POINT('Ctrl Pts',(370.448289016545,-5.69699702700445,-3.9157273471928));
#48581=CARTESIAN_POINT('Ctrl Pts',(370.333260221904,-5.6911369279164,-3.90095247985613));
#48582=CARTESIAN_POINT('Ctrl Pts',(370.214081450775,-5.68506540982229,-3.88564456901284));
#48583=CARTESIAN_POINT('Ctrl Pts',(370.095509606763,-5.67899389172818,-3.86485786911162));
#48584=CARTESIAN_POINT('Ctrl Pts',(369.978083356832,-5.67292237363407,-3.83866532628042));
#48585=CARTESIAN_POINT('Ctrl Pts',(369.864876325905,-5.66706901003732,-3.81341390244574));
#48586=CARTESIAN_POINT('Ctrl Pts',(369.752734419427,-5.66121564644057,-3.78313852030416));
#48587=CARTESIAN_POINT('Ctrl Pts',(369.642131361374,-5.65536228284383,-3.74795682587876));
#48588=CARTESIAN_POINT('Ctrl Pts',(369.531544909999,-5.64950979810993,-3.71278041386644));
#48589=CARTESIAN_POINT('Ctrl Pts',(369.42249724123,-5.64365731337604,-3.67269927954007));
#48590=CARTESIAN_POINT('Ctrl Pts',(369.315446986677,-5.63780482864214,-3.62788096424831));
#48591=CARTESIAN_POINT('Ctrl Pts',(369.208386917054,-5.631951807314,-3.58305853971895));
#48592=CARTESIAN_POINT('Ctrl Pts',(369.103325006818,-5.62609878598585,-3.53349823036481));
#48593=CARTESIAN_POINT('Ctrl Pts',(369.000699309721,-5.62024576465771,-3.47941547345564));
#48594=CARTESIAN_POINT('Ctrl Pts',(368.898039384972,-5.61439079123388,-3.4253146789023));
#48595=CARTESIAN_POINT('Ctrl Pts',(368.797817654329,-5.60853581781006,-3.36668863006956));
#48596=CARTESIAN_POINT('Ctrl Pts',(368.700446374777,-5.60268084438624,-3.30379804368727));
#48597=CARTESIAN_POINT('Ctrl Pts',(368.602964737387,-5.5968192351021,-3.24083617890346));
#48598=CARTESIAN_POINT('Ctrl Pts',(368.508340346454,-5.59095762581795,-3.1736003538628));
#48599=CARTESIAN_POINT('Ctrl Pts',(368.416955409222,-5.58509601653381,-3.10239388445924));
#48600=CARTESIAN_POINT('Ctrl Pts',(368.325508850456,-5.57923045472348,-3.03113940001043));
#48601=CARTESIAN_POINT('Ctrl Pts',(368.23730640855,-5.57336489291316,-2.95590920727524));
#48602=CARTESIAN_POINT('Ctrl Pts',(368.152694904633,-5.56749933110283,-2.87704490086473));
#48603=CARTESIAN_POINT('Ctrl Pts',(368.067959677945,-5.56162519240251,-2.79806527549552));
#48604=CARTESIAN_POINT('Ctrl Pts',(367.986826156941,-5.55575105370219,-2.71544122476289));
#48605=CARTESIAN_POINT('Ctrl Pts',(367.909602280204,-5.54987691500187,-2.62954897595249));
#48606=CARTESIAN_POINT('Ctrl Pts',(367.890073622465,-5.54839144122049,-2.60782822842837));
#48607=CARTESIAN_POINT('Ctrl Pts',(367.870794775183,-5.54690596743912,-2.58589863022008));
#48608=CARTESIAN_POINT('Ctrl Pts',(367.851770281142,-5.54542049365774,-2.56376656118834));
#48609=CARTESIAN_POINT('Ctrl Pts',(367.776391905551,-5.53953478650679,-2.47607542951134));
#48610=CARTESIAN_POINT('Ctrl Pts',(367.704746549278,-5.53364907935584,-2.38489680937957));
#48611=CARTESIAN_POINT('Ctrl Pts',(367.637177087695,-5.52776337220489,-2.29058506181116));
#48612=CARTESIAN_POINT('Ctrl Pts',(367.570345064632,-5.52194190039155,-2.19730261230155));
#48613=CARTESIAN_POINT('Ctrl Pts',(367.50750069668,-5.51612042857821,-2.10095540839542));
#48614=CARTESIAN_POINT('Ctrl Pts',(367.44893834687,-5.51029895676486,-2.00192272527074));
#48615=CARTESIAN_POINT('Ctrl Pts',(367.390431992956,-5.50448305130154,-1.90298473479348));
#48616=CARTESIAN_POINT('Ctrl Pts',(367.336199731708,-5.49866714583822,-1.80136672753239));
#48617=CARTESIAN_POINT('Ctrl Pts',(367.286493706853,-5.4928512403749,-1.69747837288983));
#48618=CARTESIAN_POINT('Ctrl Pts',(367.23682274017,-5.48703943692969,-1.59366329177548));
#48619=CARTESIAN_POINT('Ctrl Pts',(367.191671843342,-5.48122763348449,-1.48758142417816));
#48620=CARTESIAN_POINT('Ctrl Pts',(367.151247721531,-5.47541583003929,-1.37966786040398));
#48621=CARTESIAN_POINT('Ctrl Pts',(367.109947976893,-5.4694781377056,-1.26941679180456));
#48622=CARTESIAN_POINT('Ctrl Pts',(367.073582365988,-5.4635404453719,-1.15725414933701));
#48623=CARTESIAN_POINT('Ctrl Pts',(367.042319722158,-5.45760275303821,-1.04366621771041));
#48624=CARTESIAN_POINT('Ctrl Pts',(367.011734517152,-5.45179372619235,-0.932539654206915));
#48625=CARTESIAN_POINT('Ctrl Pts',(366.98603345829,-5.44598469934649,-0.820049372686403));
#48626=CARTESIAN_POINT('Ctrl Pts',(366.965324091192,-5.44017567250064,-0.706665599388753));
#48627=CARTESIAN_POINT('Ctrl Pts',(366.943926679205,-5.43417364742302,-0.589514780708706));
#48628=CARTESIAN_POINT('Ctrl Pts',(366.927858538497,-5.42817162234541,-0.471410527504311));
#48629=CARTESIAN_POINT('Ctrl Pts',(366.9171806346,-5.4221695972678,-0.352881014605549));
#48630=CARTESIAN_POINT('Ctrl Pts',(366.906502730703,-5.41616757219019,-0.234351501706782));
#48631=CARTESIAN_POINT('Ctrl Pts',(366.901215075524,-5.41016554711258,-0.115397222528112));
#48632=CARTESIAN_POINT('Ctrl Pts',(366.901319367511,-5.40416352203497,0.00345128626229814));
#48633=CARTESIAN_POINT('',(366.901317858377,-4.15416352198531,-0.000201332531193781));
#48634=CARTESIAN_POINT('Ctrl Pts',(366.901319367511,-5.40416352200791,0.00345128679815413));
#48635=CARTESIAN_POINT('Ctrl Pts',(366.901443455985,-5.39702220615151,0.144859349802664));
#48636=CARTESIAN_POINT('Ctrl Pts',(366.909197595463,-5.38988089029511,0.285932128098977));
#48637=CARTESIAN_POINT('Ctrl Pts',(366.924451232584,-5.3827395744387,0.425948364013215));
#48638=CARTESIAN_POINT('Ctrl Pts',(366.939931375364,-5.37549221512269,0.568043741412952));
#48639=CARTESIAN_POINT('Ctrl Pts',(366.963135339812,-5.36824485580668,0.709051009431602));
#48640=CARTESIAN_POINT('Ctrl Pts',(366.993877818114,-5.36099749649067,0.848238962043237));
#48641=CARTESIAN_POINT('Ctrl Pts',(367.013804958674,-5.35629978974247,0.938459986797252));
#48642=CARTESIAN_POINT('Ctrl Pts',(367.036898477992,-5.35160208299428,1.02791707226206));
#48643=CARTESIAN_POINT('Ctrl Pts',(367.063097287595,-5.34690437624608,1.11641589265549));
#48644=CARTESIAN_POINT('Ctrl Pts',(367.09585447706,-5.34103068685561,1.22706873036475));
#48645=CARTESIAN_POINT('Ctrl Pts',(367.133540412026,-5.33515699746515,1.33646292607195));
#48646=CARTESIAN_POINT('Ctrl Pts',(367.176041344644,-5.32928330807468,1.44412672116065));
#48647=CARTESIAN_POINT('Ctrl Pts',(367.218487404565,-5.32341720216902,1.55165151217537));
#48648=CARTESIAN_POINT('Ctrl Pts',(367.265735949017,-5.31755109626336,1.65744996470677));
#48649=CARTESIAN_POINT('Ctrl Pts',(367.317623124065,-5.3116849903577,1.76106421856329));
#48650=CARTESIAN_POINT('Ctrl Pts',(367.369457167306,-5.30582489126976,1.86457237274395));
#48651=CARTESIAN_POINT('Ctrl Pts',(367.425920209307,-5.29996479218181,1.9659004097976));
#48652=CARTESIAN_POINT('Ctrl Pts',(367.486800106332,-5.29410469309386,2.06460987458795));
#48653=CARTESIAN_POINT('Ctrl Pts',(367.549876411155,-5.28803317499972,2.16688055167779));
#48654=CARTESIAN_POINT('Ctrl Pts',(367.617694122466,-5.28196165690558,2.26633972479832));
#48655=CARTESIAN_POINT('Ctrl Pts',(367.689964723536,-5.27589013881143,2.36252669737809));
#48656=CARTESIAN_POINT('Ctrl Pts',(367.759638584152,-5.27003677521478,2.45525759516031));
#48657=CARTESIAN_POINT('Ctrl Pts',(367.833450580304,-5.26418341161812,2.54494703253149));
#48658=CARTESIAN_POINT('Ctrl Pts',(367.911098241926,-5.25833004802147,2.63121190787158));
#48659=CARTESIAN_POINT('Ctrl Pts',(367.988734245014,-5.25247756328766,2.71746383083095));
#48660=CARTESIAN_POINT('Ctrl Pts',(368.070204492117,-5.24662507855384,2.80029190716569));
#48661=CARTESIAN_POINT('Ctrl Pts',(368.155167276245,-5.24077259382003,2.8793473541535));
#48662=CARTESIAN_POINT('Ctrl Pts',(368.240137850318,-5.23491957249195,2.95841004946434));
#48663=CARTESIAN_POINT('Ctrl Pts',(368.3286012955,-5.22906655116387,3.03369914636362));
#48664=CARTESIAN_POINT('Ctrl Pts',(368.420180750793,-5.22321352983579,3.104904354512));
#48665=CARTESIAN_POINT('Ctrl Pts',(368.511790749603,-5.21735855641207,3.1761333109724));
#48666=CARTESIAN_POINT('Ctrl Pts',(368.606518499045,-5.21150358298834,3.24327541683681));
#48667=CARTESIAN_POINT('Ctrl Pts',(368.703956519332,-5.20564860956462,3.30606255038524));
#48668=CARTESIAN_POINT('Ctrl Pts',(368.8015049731,-5.19978700028055,3.36892084508492));
#48669=CARTESIAN_POINT('Ctrl Pts',(368.901769481247,-5.19392539099649,3.42741409199497));
#48670=CARTESIAN_POINT('Ctrl Pts',(369.004316140376,-5.18806378171242,3.48131910789192));
#48671=CARTESIAN_POINT('Ctrl Pts',(369.106931947471,-5.18219821990216,3.53526047233701));
#48672=CARTESIAN_POINT('Ctrl Pts',(369.211832596861,-5.17633265809191,3.58460726974429));
#48673=CARTESIAN_POINT('Ctrl Pts',(369.318563897641,-5.17046709628165,3.62918433620219));
#48674=CARTESIAN_POINT('Ctrl Pts',(369.425451265761,-5.1645929575814,3.67382658526451));
#48675=CARTESIAN_POINT('Ctrl Pts',(369.534174241206,-5.15871881888115,3.7136850423363));
#48676=CARTESIAN_POINT('Ctrl Pts',(369.64426310874,-5.15284468018091,3.7486342453127));
#48677=CARTESIAN_POINT('Ctrl Pts',(369.672102786142,-5.15135920639875,3.75747232820079));
#48678=CARTESIAN_POINT('Ctrl Pts',(369.700029762253,-5.14987373261658,3.76599671886946));
#48679=CARTESIAN_POINT('Ctrl Pts',(369.728036351832,-5.14838825883442,3.77420590848957));
#48680=CARTESIAN_POINT('Ctrl Pts',(369.838776783638,-5.14251456944392,3.80666574087116));
#48681=CARTESIAN_POINT('Ctrl Pts',(369.951131488505,-5.13664088005343,3.83430158793247));
#48682=CARTESIAN_POINT('Ctrl Pts',(370.064642380177,-5.13076719066293,3.8569532880488));
#48683=CARTESIAN_POINT('Ctrl Pts',(370.178006718624,-5.12490108475724,3.87957574269224));
#48684=CARTESIAN_POINT('Ctrl Pts',(370.292523873838,-5.11903497885156,3.89722676738695));
#48685=CARTESIAN_POINT('Ctrl Pts',(370.407720275528,-5.11316887294588,3.90979583951695));
#48686=CARTESIAN_POINT('Ctrl Pts',(370.522798717571,-5.10730877385791,3.92235204107722));
#48687=CARTESIAN_POINT('Ctrl Pts',(370.638554614338,-5.10144867476994,3.9298365964251));
#48688=CARTESIAN_POINT('Ctrl Pts',(370.754504523402,-5.09558857568197,3.93219008090691));
#48689=CARTESIAN_POINT('Ctrl Pts',(370.874637640662,-5.08951705758784,3.9346284737397));
#48690=CARTESIAN_POINT('Ctrl Pts',(370.994978590628,-5.08344553949371,3.93155848245066));
#48691=CARTESIAN_POINT('Ctrl Pts',(371.114983838692,-5.07737402139957,3.92297280191965));
#48692=CARTESIAN_POINT('Ctrl Pts',(371.230677202285,-5.0715206578029,3.91469561175176));
#48693=CARTESIAN_POINT('Ctrl Pts',(371.34605812546,-5.06566729420622,3.90129230920273));
#48694=CARTESIAN_POINT('Ctrl Pts',(371.46064071302,-5.05981393060954,3.88280937921204));
#48695=CARTESIAN_POINT('Ctrl Pts',(371.57520609639,-5.05396144587571,3.86432922437107));
#48696=CARTESIAN_POINT('Ctrl Pts',(371.688972974722,-5.04810896114188,3.84077102437545));
#48697=CARTESIAN_POINT('Ctrl Pts',(371.801463020548,-5.04225647640805,3.81223283986203));
#48698=CARTESIAN_POINT('Ctrl Pts',(371.9139633802,-5.03640345507995,3.78369203878026));
#48699=CARTESIAN_POINT('Ctrl Pts',(372.025186274143,-5.03055043375185,3.75017044710723));
#48700=CARTESIAN_POINT('Ctrl Pts',(372.13466666304,-5.02469741242375,3.71181653275185));
#48701=CARTESIAN_POINT('Ctrl Pts',(372.244183565761,-5.018842439,3.67344982662537));
#48702=CARTESIAN_POINT('Ctrl Pts',(372.351956418126,-5.01298746557626,3.63024772959922));
#48703=CARTESIAN_POINT('Ctrl Pts',(372.457539016682,-5.00713249215252,3.58240729880111));
#48704=CARTESIAN_POINT('Ctrl Pts',(372.563241279551,-5.00127088286844,3.53451264701955));
#48705=CARTESIAN_POINT('Ctrl Pts',(372.666747957422,-4.99540927358436,3.48196933950716));
#48706=CARTESIAN_POINT('Ctrl Pts',(372.76763628452,-4.98954766430028,3.42502099894465));
#48707=CARTESIAN_POINT('Ctrl Pts',(372.868592641358,-4.98368210249002,3.36803425769789));
#48708=CARTESIAN_POINT('Ctrl Pts',(372.966926782199,-4.97781654067976,3.30663678705056));
#48709=CARTESIAN_POINT('Ctrl Pts',(373.062245294225,-4.97195097886949,3.24111528916138));
#48710=CARTESIAN_POINT('Ctrl Pts',(373.157703185293,-4.96607684016924,3.17549798277209));
#48711=CARTESIAN_POINT('Ctrl Pts',(373.250136318602,-4.96020270146898,3.10574486200673));
#48712=CARTESIAN_POINT('Ctrl Pts',(373.339184630263,-4.95432856276873,3.03218261806313));
#48713=CARTESIAN_POINT('Ctrl Pts',(373.361703494569,-4.95284308898674,3.01357992747338));
#48714=CARTESIAN_POINT('Ctrl Pts',(373.384006086301,-4.95135761520476,2.9947338235578));
#48715=CARTESIAN_POINT('Ctrl Pts',(373.406086971337,-4.94987214142277,2.97564994633422));
#48716=CARTESIAN_POINT('Ctrl Pts',(373.493396664552,-4.94399845203163,2.90019067633606));
#48717=CARTESIAN_POINT('Ctrl Pts',(373.577527837825,-4.93812476264049,2.82075979169304));
#48718=CARTESIAN_POINT('Ctrl Pts',(373.658097573172,-4.93225107324935,2.73765540074166));
#48719=CARTESIAN_POINT('Ctrl Pts',(373.738563285421,-4.92638496734302,2.65465830536628));
#48720=CARTESIAN_POINT('Ctrl Pts',(373.815476419005,-4.92051886143669,2.56799742955658));
#48721=CARTESIAN_POINT('Ctrl Pts',(373.888487373944,-4.91465275553036,2.4780108027816));
#48722=CARTESIAN_POINT('Ctrl Pts',(373.961423566596,-4.90879265644175,2.38811632116605));
#48723=CARTESIAN_POINT('Ctrl Pts',(374.030465269786,-4.90293255735314,2.2949031813806));
#48724=CARTESIAN_POINT('Ctrl Pts',(374.095300469772,-4.89707245826453,2.19874540922173));
#48725=CARTESIAN_POINT('Ctrl Pts',(374.162474775852,-4.89100094017063,2.09911848402769));
#48726=CARTESIAN_POINT('Ctrl Pts',(374.225133011615,-4.88492942207674,1.99633076795799));
#48727=CARTESIAN_POINT('Ctrl Pts',(374.282974383232,-4.87885790398285,1.89083503723376));
#48728=CARTESIAN_POINT('Ctrl Pts',(374.338737468149,-4.87300454038553,1.78912985241094));
#48729=CARTESIAN_POINT('Ctrl Pts',(374.390023663683,-4.8671511767882,1.68490829944616));
#48730=CARTESIAN_POINT('Ctrl Pts',(374.436608623086,-4.86129781319088,1.57860387981518));
#48731=CARTESIAN_POINT('Ctrl Pts',(374.483186587914,-4.8554453284564,1.47231542143513));
#48732=CARTESIAN_POINT('Ctrl Pts',(374.525064554373,-4.84959284372192,1.36394509652811));
#48733=CARTESIAN_POINT('Ctrl Pts',(374.562065617717,-4.84374035898745,1.2539480070243));
#48734=CARTESIAN_POINT('Ctrl Pts',(374.599070073561,-4.8378873376587,1.14394083226427));
#48735=CARTESIAN_POINT('Ctrl Pts',(374.631196605674,-4.83203431632996,1.03230698801189));
#48736=CARTESIAN_POINT('Ctrl Pts',(374.658317870557,-4.82618129500121,0.919517736337605));
#48737=CARTESIAN_POINT('Ctrl Pts',(374.685448180905,-4.82032632157682,0.806690867269793));
#48738=CARTESIAN_POINT('Ctrl Pts',(374.70756980805,-4.81447134815243,0.692708226005589));
#48739=CARTESIAN_POINT('Ctrl Pts',(374.724606449506,-4.80861637472804,0.578051587351353));
#48740=CARTESIAN_POINT('Ctrl Pts',(374.741662399806,-4.80275476544333,0.463265000124452));
#48741=CARTESIAN_POINT('Ctrl Pts',(374.753621800706,-4.79689315615861,0.347803299717017));
#48742=CARTESIAN_POINT('Ctrl Pts',(374.760460184908,-4.7910315468739,0.232153809697238));
#48743=CARTESIAN_POINT('Ctrl Pts',(374.767303180283,-4.785165985063,0.116426336377062));
#48744=CARTESIAN_POINT('Ctrl Pts',(374.769018276898,-4.7793004232521,0.000511233377731596));
#48745=CARTESIAN_POINT('Ctrl Pts',(374.765633119996,-4.7734348614412,-0.115105487454939));
#48746=CARTESIAN_POINT('Ctrl Pts',(374.762243013165,-4.76756072274032,-0.230891268290099));
#48747=CARTESIAN_POINT('Ctrl Pts',(374.753737799107,-4.76168658403944,-0.346377385752583));
#48748=CARTESIAN_POINT('Ctrl Pts',(374.740196804942,-4.75581244533856,-0.461084172926413));
#48749=CARTESIAN_POINT('Ctrl Pts',(374.736772508589,-4.75432697156275,-0.490091646690872));
#48750=CARTESIAN_POINT('Ctrl Pts',(374.733026426693,-4.75284149778693,-0.519049341594463));
#48751=CARTESIAN_POINT('Ctrl Pts',(374.728960352713,-4.75135602401112,-0.547949633793531));
#48752=CARTESIAN_POINT('Ctrl Pts',(374.712882751089,-4.7454823346216,-0.662223842068144));
#48753=CARTESIAN_POINT('Ctrl Pts',(374.691744664624,-4.73960864523207,-0.775980165168239));
#48754=CARTESIAN_POINT('Ctrl Pts',(374.665589012611,-4.73373495584255,-0.888735226740352));
#48755=CARTESIAN_POINT('Ctrl Pts',(374.639467130002,-4.72786884993784,-1.00134471093508));
#48756=CARTESIAN_POINT('Ctrl Pts',(374.608340657263,-4.72200274403313,-1.11295510562042));
#48757=CARTESIAN_POINT('Ctrl Pts',(374.572304121735,-4.71613663812842,-1.22308939020026));
#48758=CARTESIAN_POINT('Ctrl Pts',(374.536304487161,-4.71027653904142,-1.33311089867579));
#48759=CARTESIAN_POINT('Ctrl Pts',(374.495404918309,-4.70441643995442,-1.44165891325449));
#48760=CARTESIAN_POINT('Ctrl Pts',(374.449750566373,-4.69855634086742,-1.54826848339961));
#48761=CARTESIAN_POINT('Ctrl Pts',(374.402449109563,-4.69248482277292,-1.6587242836469));
#48762=CARTESIAN_POINT('Ctrl Pts',(374.350043410704,-4.68641330467842,-1.76709868936488));
#48763=CARTESIAN_POINT('Ctrl Pts',(374.292750878012,-4.68034178658393,-1.87289348684141));
#48764=CARTESIAN_POINT('Ctrl Pts',(374.23751691182,-4.6744884229882,-1.97488699267111));
#48765=CARTESIAN_POINT('Ctrl Pts',(374.17774145742,-4.66863505939248,-2.074482680326));
#48766=CARTESIAN_POINT('Ctrl Pts',(374.113667168997,-4.66278169579675,-2.17125702419965));
#48767=CARTESIAN_POINT('Ctrl Pts',(374.049602501113,-4.65692921106386,-2.26801683773135));
#48768=CARTESIAN_POINT('Ctrl Pts',(373.981240510635,-4.65107672633098,-2.36195580539885));
#48769=CARTESIAN_POINT('Ctrl Pts',(373.908867721538,-4.64522424159809,-2.45267855766956));
#48770=CARTESIAN_POINT('Ctrl Pts',(373.836488296828,-4.63937122027092,-2.54340962799867));
#48771=CARTESIAN_POINT('Ctrl Pts',(373.760097600132,-4.63351819894376,-2.63092357374349));
#48772=CARTESIAN_POINT('Ctrl Pts',(373.680022602544,-4.62766517761659,-2.71485791151199));
#48773=CARTESIAN_POINT('Ctrl Pts',(373.599920898397,-4.62181020419378,-2.79882024300317));
#48774=CARTESIAN_POINT('Ctrl Pts',(373.516132735004,-4.61595523077096,-2.87920029379615));
#48775=CARTESIAN_POINT('Ctrl Pts',(373.429021587211,-4.61010025734814,-2.95567277160947));
#48776=CARTESIAN_POINT('Ctrl Pts',(373.341811710121,-4.60423864806497,-3.03223192115416));
#48777=CARTESIAN_POINT('Ctrl Pts',(373.251271642225,-4.59837703878179,-3.10487438552158));
#48778=CARTESIAN_POINT('Ctrl Pts',(373.157797621388,-4.59251542949862,-3.17331542191015));
#48779=CARTESIAN_POINT('Ctrl Pts',(373.064260570332,-4.58664986768925,-3.24180260859232));
#48780=CARTESIAN_POINT('Ctrl Pts',(372.967785969897,-4.58078430587988,-3.30608249754257));
#48781=CARTESIAN_POINT('Ctrl Pts',(372.868797206398,-4.57491874407051,-3.3659148476317));
#48782=CARTESIAN_POINT('Ctrl Pts',(372.769663697049,-4.56904460537112,-3.42583468729174));
#48783=CARTESIAN_POINT('Ctrl Pts',(372.668009048907,-4.56317046667174,-3.48129381184849));
#48784=CARTESIAN_POINT('Ctrl Pts',(372.564279333832,-4.55729632797235,-3.53209884850545));
#48785=CARTESIAN_POINT('Ctrl Pts',(372.538047782114,-4.55581085418139,-3.54494661296339));
#48786=CARTESIAN_POINT('Ctrl Pts',(372.511683616958,-4.55432538039042,-3.55749699290363));
#48787=CARTESIAN_POINT('Ctrl Pts',(372.48519421699,-4.55283990659946,-3.56974736242754));
#48788=CARTESIAN_POINT('Ctrl Pts',(372.380452882276,-4.54696621720899,-3.61818636279197));
#48789=CARTESIAN_POINT('Ctrl Pts',(372.273403393574,-4.54109252781852,-3.66209224755465));
#48790=CARTESIAN_POINT('Ctrl Pts',(372.164475202786,-4.53521883842805,-3.70123903921455));
#48791=CARTESIAN_POINT('Ctrl Pts',(372.055687648526,-4.5293527325224,-3.74033528868866));
#48792=CARTESIAN_POINT('Ctrl Pts',(371.945026601111,-4.52348662661676,-3.77468452587795));
#48793=CARTESIAN_POINT('Ctrl Pts',(371.832944148865,-4.51762052071111,-3.80410758544697));
#48794=CARTESIAN_POINT('Ctrl Pts',(371.720976467621,-4.51176042162319,-3.83350051617779));
#48795=CARTESIAN_POINT('Ctrl Pts',(371.607590673886,-4.50590032253527,-3.85797719862695));
#48796=CARTESIAN_POINT('Ctrl Pts',(371.493256157088,-4.50004022344735,-3.87740755037443));
#48797=CARTESIAN_POINT('Ctrl Pts',(371.37479671176,-4.4939687053532,-3.89753890488576));
#48798=CARTESIAN_POINT('Ctrl Pts',(371.255319220426,-4.48789718725905,-3.91225278098011));
#48799=CARTESIAN_POINT('Ctrl Pts',(371.135360195041,-4.48182566916491,-3.92146178209518));
#48800=CARTESIAN_POINT('Ctrl Pts',(371.019711393311,-4.4759723055683,-3.93033989644025));
#48801=CARTESIAN_POINT('Ctrl Pts',(370.903615513057,-4.47011894197169,-3.9341018825666));
#48802=CARTESIAN_POINT('Ctrl Pts',(370.787559991312,-4.46426557837508,-3.93272204743095));
#48803=CARTESIAN_POINT('Ctrl Pts',(370.671521894914,-4.45841309364133,-3.93134241947289));
#48804=CARTESIAN_POINT('Ctrl Pts',(370.55552455798,-4.45256060890758,-3.92482251024321));
#48805=CARTESIAN_POINT('Ctrl Pts',(370.440055540005,-4.44670812417383,-3.91318875450386));
#48806=CARTESIAN_POINT('Ctrl Pts',(370.324575935072,-4.44085510284582,-3.90155393210533));
#48807=CARTESIAN_POINT('Ctrl Pts',(370.209625156478,-4.4350020815178,-3.88480437254318));
#48808=CARTESIAN_POINT('Ctrl Pts',(370.095685056001,-4.42914906018979,-3.86301832649884));
#48809=CARTESIAN_POINT('Ctrl Pts',(369.9817069543,-4.42329408676615,-3.84122501438746));
#48810=CARTESIAN_POINT('Ctrl Pts',(369.868740606561,-4.4174391133425,-3.8143919532035));
#48811=CARTESIAN_POINT('Ctrl Pts',(369.757256401613,-4.41158413991886,-3.78264822967379));
#48812=CARTESIAN_POINT('Ctrl Pts',(369.645645843639,-4.40572253063489,-3.75086852871079));
#48813=CARTESIAN_POINT('Ctrl Pts',(369.535521178845,-4.39986092135091,-3.71416716999359));
#48814=CARTESIAN_POINT('Ctrl Pts',(369.427336483157,-4.39399931206694,-3.67272275352827));
#48815=CARTESIAN_POINT('Ctrl Pts',(369.319078837735,-4.38813375025678,-3.63125039078861));
#48816=CARTESIAN_POINT('Ctrl Pts',(369.212764144155,-4.38226818844663,-3.58502876613611));
#48817=CARTESIAN_POINT('Ctrl Pts',(369.108823800672,-4.37640262663648,-3.53428341741415));
#48818=CARTESIAN_POINT('Ctrl Pts',(369.004731470915,-4.37052848793635,-3.48346386654634));
#48819=CARTESIAN_POINT('Ctrl Pts',(368.903020781746,-4.36465434923621,-3.42810758688272));
#48820=CARTESIAN_POINT('Ctrl Pts',(368.804096045641,-4.35878021053608,-3.36848458687471));
#48821=CARTESIAN_POINT('Ctrl Pts',(368.779079594812,-4.35729473675332,-3.35340690350991));
#48822=CARTESIAN_POINT('Ctrl Pts',(368.754241147519,-4.35580926297056,-3.33805656905904));
#48823=CARTESIAN_POINT('Ctrl Pts',(368.729586910349,-4.3543237891878,-3.32243836031665));
#48824=CARTESIAN_POINT('Ctrl Pts',(368.632101964404,-4.34845009979252,-3.26068263757823));
#48825=CARTESIAN_POINT('Ctrl Pts',(368.537174958848,-4.34257641039724,-3.19452990984391));
#48826=CARTESIAN_POINT('Ctrl Pts',(368.44522859431,-4.33670272100197,-3.12421854436291));
#48827=CARTESIAN_POINT('Ctrl Pts',(368.353400941165,-4.33083661509148,-3.05399795745991));
#48828=CARTESIAN_POINT('Ctrl Pts',(368.264546601244,-4.324970509181,-2.97962965904421));
#48829=CARTESIAN_POINT('Ctrl Pts',(368.179061209962,-4.31910440327052,-2.90139641524809));
#48830=CARTESIAN_POINT('Ctrl Pts',(368.093663354632,-4.31324430417774,-2.82324328129676));
#48831=CARTESIAN_POINT('Ctrl Pts',(368.011627889049,-4.30738420508496,-2.74123335133408));
#48832=CARTESIAN_POINT('Ctrl Pts',(367.933318582965,-4.30152410599219,-2.65569053806343));
#48833=CARTESIAN_POINT('Ctrl Pts',(367.85218405586,-4.29545258789985,-2.56706153534194));
#48834=CARTESIAN_POINT('Ctrl Pts',(367.775049985958,-4.28938106980751,-2.47464019400271));
#48835=CARTESIAN_POINT('Ctrl Pts',(367.702280661507,-4.28330955171518,-2.37882997074181));
#48836=CARTESIAN_POINT('Ctrl Pts',(367.632125996962,-4.2774561881137,-2.28646228527073));
#48837=CARTESIAN_POINT('Ctrl Pts',(367.566028089594,-4.27160282451223,-2.19094541443752));
#48838=CARTESIAN_POINT('Ctrl Pts',(367.504272773721,-4.26574946091075,-2.09267502696315));
#48839=CARTESIAN_POINT('Ctrl Pts',(367.4425267302,-4.25989697617212,-1.99441939445682));
#48840=CARTESIAN_POINT('Ctrl Pts',(367.38512220147,-4.2540444914335,-1.89341141707912));
#48841=CARTESIAN_POINT('Ctrl Pts',(367.332301284831,-4.24819200669487,-1.79007512543516));
#48842=CARTESIAN_POINT('Ctrl Pts',(367.279475525224,-4.24233898536199,-1.68672935924111));
#48843=CARTESIAN_POINT('Ctrl Pts',(367.231234401187,-4.23648596402912,-1.58105522230436));
#48844=CARTESIAN_POINT('Ctrl Pts',(367.187773374491,-4.23063294269625,-1.47350003889497));
#48845=CARTESIAN_POINT('Ctrl Pts',(367.144297852704,-4.22477796926775,-1.36590898375529));
#48846=CARTESIAN_POINT('Ctrl Pts',(367.105605753064,-4.21892299583925,-1.25643601750229));
#48847=CARTESIAN_POINT('Ctrl Pts',(367.071843605239,-4.21306802241076,-1.14554639070291));
#48848=CARTESIAN_POINT('Ctrl Pts',(367.038043192357,-4.20720641312197,-1.03453108475579));
#48849=CARTESIAN_POINT('Ctrl Pts',(367.009184003941,-4.20134480383319,-0.922096309028896));
#48850=CARTESIAN_POINT('Ctrl Pts',(366.985362119881,-4.19548319454441,-0.808720447848522));
#48851=CARTESIAN_POINT('Ctrl Pts',(366.961524172551,-4.18961763272946,-0.695268136492842));
#48852=CARTESIAN_POINT('Ctrl Pts',(366.942730359955,-4.18375207091451,-0.580873882763329));
#48853=CARTESIAN_POINT('Ctrl Pts',(366.929025025973,-4.17788650909957,-0.466022460209995));
#48854=CARTESIAN_POINT('Ctrl Pts',(366.915299651431,-4.17201237039471,-0.351003096709402));
#48855=CARTESIAN_POINT('Ctrl Pts',(366.906677635719,-4.16613823168985,-0.235525640655453));
#48856=CARTESIAN_POINT('Ctrl Pts',(366.903151270257,-4.160264092985,-0.120076213144621));
#48857=CARTESIAN_POINT('Ctrl Pts',(366.902259510027,-4.15877861924871,-0.0908809385600446));
#48858=CARTESIAN_POINT('Ctrl Pts',(366.901693358034,-4.15729314551243,-0.061687434995945));
#48859=CARTESIAN_POINT('Ctrl Pts',(366.90145216495,-4.15580767177615,-0.0325035074416985));
#48860=CARTESIAN_POINT('Ctrl Pts',(366.901363179298,-4.15525962186242,-0.0217364042693529));
#48861=CARTESIAN_POINT('Ctrl Pts',(366.90131840958,-4.15471157194869,-0.0109689351661175));
#48862=CARTESIAN_POINT('Ctrl Pts',(366.901317858377,-4.15416352203497,-0.000201333506838279));
#48863=CARTESIAN_POINT('',(366.901319261778,-2.90416352206856,-0.00332861608659438));
#48864=CARTESIAN_POINT('Ctrl Pts',(366.901317858377,-4.15416352198531,-0.000201332531196401));
#48865=CARTESIAN_POINT('Ctrl Pts',(366.901311959597,-4.14829845024365,0.115030427635469));
#48866=CARTESIAN_POINT('Ctrl Pts',(366.906374564303,-4.14243337850199,0.230457043287648));
#48867=CARTESIAN_POINT('Ctrl Pts',(366.916531103072,-4.13656830676033,0.3455951103968));
#48868=CARTESIAN_POINT('Ctrl Pts',(366.926674528538,-4.13071080752541,0.460584520536864));
#48869=CARTESIAN_POINT('Ctrl Pts',(366.941898773558,-4.12485330829048,0.575285713870508));
#48870=CARTESIAN_POINT('Ctrl Pts',(366.962177279116,-4.11899580905555,0.689214316700083));
#48871=CARTESIAN_POINT('Ctrl Pts',(366.98243506294,-4.11314429534733,0.803026500787282));
#48872=CARTESIAN_POINT('Ctrl Pts',(367.007736762632,-4.10729278163911,0.916067258950138));
#48873=CARTESIAN_POINT('Ctrl Pts',(367.038004001566,-4.10144126793088,1.02785706190746));
#48874=CARTESIAN_POINT('Ctrl Pts',(367.069071559755,-4.09543502986562,1.14260278469151));
#48875=CARTESIAN_POINT('Ctrl Pts',(367.105370893532,-4.08942879180035,1.256030028129));
#48876=CARTESIAN_POINT('Ctrl Pts',(367.146761046028,-4.08342255373508,1.36763072270954));
#48877=CARTESIAN_POINT('Ctrl Pts',(367.187039217511,-4.07757767827118,1.47623317143383));
#48878=CARTESIAN_POINT('Ctrl Pts',(367.23213798919,-4.07173280280727,1.58310555597647));
#48879=CARTESIAN_POINT('Ctrl Pts',(367.281877114629,-4.06588792734336,1.68779554412487));
#48880=CARTESIAN_POINT('Ctrl Pts',(367.331609051504,-4.06004389661206,1.79247040191723));
#48881=CARTESIAN_POINT('Ctrl Pts',(367.385979830845,-4.05419986588076,1.89496311613479));
#48882=CARTESIAN_POINT('Ctrl Pts',(367.444761818848,-4.04835583514946,1.99484307398559));
#48883=CARTESIAN_POINT('Ctrl Pts',(367.503549640188,-4.04251122447522,2.09473294360429));
#48884=CARTESIAN_POINT('Ctrl Pts',(367.566749330053,-4.03666661380098,2.19200918422794));
#48885=CARTESIAN_POINT('Ctrl Pts',(367.634088602332,-4.03082200312674,2.28626808177333));
#48886=CARTESIAN_POINT('Ctrl Pts',(367.704687643426,-4.02469446572989,2.3850898770798));
#48887=CARTESIAN_POINT('Ctrl Pts',(367.779836810539,-4.01856692833304,2.48059445845192));
#48888=CARTESIAN_POINT('Ctrl Pts',(367.859173997445,-4.01243939093618,2.57235457070331));
#48889=CARTESIAN_POINT('Ctrl Pts',(367.934961989404,-4.00658597246905,2.66000974125744));
#48890=CARTESIAN_POINT('Ctrl Pts',(368.014571057159,-4.00073255400193,2.74424795993098));
#48891=CARTESIAN_POINT('Ctrl Pts',(368.097647806168,-3.9948791355348,2.82473468728379));
#48892=CARTESIAN_POINT('Ctrl Pts',(368.180782445084,-3.98902163826277,2.90527749975334));
#48893=CARTESIAN_POINT('Ctrl Pts',(368.267389266849,-3.98316414099074,2.98206334218022));
#48894=CARTESIAN_POINT('Ctrl Pts',(368.357082035874,-3.97730664371871,3.05479814476148));
#48895=CARTESIAN_POINT('Ctrl Pts',(368.446903188543,-3.97144076219393,3.12763705784251));
#48896=CARTESIAN_POINT('Ctrl Pts',(368.539818769934,-3.96557488066915,3.19641311649315));
#48897=CARTESIAN_POINT('Ctrl Pts',(368.63541389815,-3.95970899914438,3.26087571004458));
#48898=CARTESIAN_POINT('Ctrl Pts',(368.648546106992,-3.95890318421775,3.26973114291913));
#48899=CARTESIAN_POINT('Ctrl Pts',(368.661728846035,-3.95809736929113,3.27850524631598));
#48900=CARTESIAN_POINT('Ctrl Pts',(368.674961006031,-3.9572915543645,3.28719743953404));
#48901=CARTESIAN_POINT('Ctrl Pts',(368.771411934462,-3.95141786497133,3.35055596197065));
#48902=CARTESIAN_POINT('Ctrl Pts',(368.870814404899,-3.94554417557816,3.40977140443023));
#48903=CARTESIAN_POINT('Ctrl Pts',(368.972776994441,-3.93967048618499,3.46455691699257));
#48904=CARTESIAN_POINT('Ctrl Pts',(369.074607940699,-3.93380438027672,3.5192716963105));
#48905=CARTESIAN_POINT('Ctrl Pts',(369.178992072182,-3.92793827436845,3.56956772609239));
#48906=CARTESIAN_POINT('Ctrl Pts',(369.285508672368,-3.92207216846018,3.61520111768304));
#48907=CARTESIAN_POINT('Ctrl Pts',(369.391916200911,-3.91621206936971,3.66078778126142));
#48908=CARTESIAN_POINT('Ctrl Pts',(369.500451477251,-3.91035197027924,3.70172114176048));
#48909=CARTESIAN_POINT('Ctrl Pts',(369.610669433267,-3.90449187118878,3.7378033046614));
#48910=CARTESIAN_POINT('Ctrl Pts',(369.724863801624,-3.89842035309561,3.77518722966189));
#48911=CARTESIAN_POINT('Ctrl Pts',(369.840864158629,-3.89234883500245,3.80736309407966));
#48912=CARTESIAN_POINT('Ctrl Pts',(369.958152751656,-3.88627731690928,3.83416532178712));
#48913=CARTESIAN_POINT('Ctrl Pts',(370.071227071861,-3.88042395331036,3.86000452404688));
#48914=CARTESIAN_POINT('Ctrl Pts',(370.185498209295,-3.87457058971143,3.88084950207189));
#48915=CARTESIAN_POINT('Ctrl Pts',(370.300487848205,-3.8687172261125,3.89660294689376));
#48916=CARTESIAN_POINT('Ctrl Pts',(370.415460221806,-3.86286474137651,3.91235402638865));
#48917=CARTESIAN_POINT('Ctrl Pts',(370.531150473165,-3.85701225664053,3.9230150366856));
#48918=CARTESIAN_POINT('Ctrl Pts',(370.647072476559,-3.85115977190454,3.92854020838753));
#48919=CARTESIAN_POINT('Ctrl Pts',(370.763005108442,-3.84530675057437,3.93406588667342));
#48920=CARTESIAN_POINT('Ctrl Pts',(370.879169121901,-3.83945372924421,3.93445477061384));
#48921=CARTESIAN_POINT('Ctrl Pts',(370.995076393649,-3.83360070791404,3.92971318185953));
#48922=CARTESIAN_POINT('Ctrl Pts',(371.111022322708,-3.82774573448833,3.92497001169388));
#48923=CARTESIAN_POINT('Ctrl Pts',(371.226710927212,-3.82189076106261,3.91509298324222));
#48924=CARTESIAN_POINT('Ctrl Pts',(371.341657923126,-3.8160357876369,3.90014038894392));
#48925=CARTESIAN_POINT('Ctrl Pts',(371.456735196693,-3.810174178351,3.88517084780096));
#48926=CARTESIAN_POINT('Ctrl Pts',(371.571068774125,-3.8043125690651,3.86511431248785));
#48927=CARTESIAN_POINT('Ctrl Pts',(371.684183202654,-3.7984509597792,3.84008045330274));
#48928=CARTESIAN_POINT('Ctrl Pts',(371.797373905072,-3.79258539796719,3.81502971360289));
#48929=CARTESIAN_POINT('Ctrl Pts',(371.909343423589,-3.78671983615519,3.78499507377374));
#48930=CARTESIAN_POINT('Ctrl Pts',(372.019631811733,-3.78085427434318,3.75013597350344));
#48931=CARTESIAN_POINT('Ctrl Pts',(372.130081468547,-3.77498013564133,3.71522590067961));
#48932=CARTESIAN_POINT('Ctrl Pts',(372.238844702436,-3.76910599693947,3.6754774295862));
#48933=CARTESIAN_POINT('Ctrl Pts',(372.345481797028,-3.76323185823761,3.6310979792545));
#48934=CARTESIAN_POINT('Ctrl Pts',(372.372448577023,-3.76174638447602,3.61987514091721));
#48935=CARTESIAN_POINT('Ctrl Pts',(372.399279516508,-3.76026091071442,3.60835637822555));
#48936=CARTESIAN_POINT('Ctrl Pts',(372.425967772208,-3.75877543695283,3.59654550025402));
#48937=CARTESIAN_POINT('Ctrl Pts',(372.531495402127,-3.7529017475244,3.54984428554702));
#48938=CARTESIAN_POINT('Ctrl Pts',(372.635141628382,-3.74702805809597,3.49841686381751));
#48939=CARTESIAN_POINT('Ctrl Pts',(372.736453214653,-3.74115436866754,3.44243664673768));
#48940=CARTESIAN_POINT('Ctrl Pts',(372.837633998151,-3.73528826272376,3.38652870537523));
#48941=CARTESIAN_POINT('Ctrl Pts',(372.936485777689,-3.72942215677999,3.32607985623519));
#48942=CARTESIAN_POINT('Ctrl Pts',(373.032575537284,-3.72355605083621,3.2613114163583));
#48943=CARTESIAN_POINT('Ctrl Pts',(373.128566902192,-3.71769595171007,3.19660929853737));
#48944=CARTESIAN_POINT('Ctrl Pts',(373.221801532277,-3.71183585258392,3.12759661764766));
#48945=CARTESIAN_POINT('Ctrl Pts',(373.311871859558,-3.70597575345778,3.054540087427));
#48946=CARTESIAN_POINT('Ctrl Pts',(373.405191717938,-3.69990423537792,2.97884784493447));
#48947=CARTESIAN_POINT('Ctrl Pts',(373.495114245767,-3.69383271729806,2.89881467686671));
#48948=CARTESIAN_POINT('Ctrl Pts',(373.581219629511,-3.6877611992182,2.81478589442051));
#48949=CARTESIAN_POINT('Ctrl Pts',(373.66423117874,-3.68190783558331,2.73377633256367));
#48950=CARTESIAN_POINT('Ctrl Pts',(373.743694848106,-3.67605447194841,2.64905365930637));
#48951=CARTESIAN_POINT('Ctrl Pts',(373.8192695686,-3.67020110831352,2.56096705501544));
#48952=CARTESIAN_POINT('Ctrl Pts',(373.894832941803,-3.66434862354153,2.47289367663253));
#48953=CARTESIAN_POINT('Ctrl Pts',(373.966508258225,-3.65849613876954,2.38145768498292));
#48954=CARTESIAN_POINT('Ctrl Pts',(374.033993524102,-3.65264365399755,2.28704276330604));
#48955=CARTESIAN_POINT('Ctrl Pts',(374.101484977471,-3.64679063263138,2.19261918505006));
#48956=CARTESIAN_POINT('Ctrl Pts',(374.16478537634,-3.64093761126521,2.09521646994503));
#48957=CARTESIAN_POINT('Ctrl Pts',(374.223635416565,-3.63508458989904,1.99524821885047));
#48958=CARTESIAN_POINT('Ctrl Pts',(374.282505084414,-3.62922961643737,1.89524662641627));
#48959=CARTESIAN_POINT('Ctrl Pts',(374.336921232713,-3.6233746429757,1.79267815240053));
#48960=CARTESIAN_POINT('Ctrl Pts',(374.386670310075,-3.61751966951403,1.68798134536712));
#48961=CARTESIAN_POINT('Ctrl Pts',(374.436475771622,-3.61165806019242,1.58316587795847));
#48962=CARTESIAN_POINT('Ctrl Pts',(374.481603427243,-3.6057964508708,1.47621763631053));
#48963=CARTESIAN_POINT('Ctrl Pts',(374.521887686282,-3.59993484154919,1.36759560043147));
#48964=CARTESIAN_POINT('Ctrl Pts',(374.562199109291,-3.59406927970158,1.25890031991987));
#48965=CARTESIAN_POINT('Ctrl Pts',(374.597660506445,-3.58820371785396,1.14852939014922));
#48966=CARTESIAN_POINT('Ctrl Pts',(374.628156514806,-3.58233815600635,1.03695574152775));
#48967=CARTESIAN_POINT('Ctrl Pts',(374.658697115807,-3.57646401726932,0.925218944878658));
#48968=CARTESIAN_POINT('Ctrl Pts',(374.684257746806,-3.57058987853229,0.812276320921258));
#48969=CARTESIAN_POINT('Ctrl Pts',(374.704774329213,-3.56471573979525,0.698609810607917));
#48970=CARTESIAN_POINT('Ctrl Pts',(374.709962636666,-3.56323026637723,0.66986541297809));
#48971=CARTESIAN_POINT('Ctrl Pts',(374.71482863628,-3.56174479295921,0.641074739808487));
#48972=CARTESIAN_POINT('Ctrl Pts',(374.719371819044,-3.56025931954118,0.612245606488703));
#48973=CARTESIAN_POINT('Ctrl Pts',(374.737335953332,-3.55438563024687,0.49825274085406));
#48974=CARTESIAN_POINT('Ctrl Pts',(374.750308692182,-3.54851194095256,0.383278711694387));
#48975=CARTESIAN_POINT('Ctrl Pts',(374.758190051055,-3.54263825165825,0.267798385142579));
#48976=CARTESIAN_POINT('Ctrl Pts',(374.766061234354,-3.53677214584872,0.152467154543017));
#48977=CARTESIAN_POINT('Ctrl Pts',(374.76885408224,-3.53090604003919,0.0366313349230434));
#48978=CARTESIAN_POINT('Ctrl Pts',(374.766519827068,-3.52503993422966,-0.0792252289365442));
#48979=CARTESIAN_POINT('Ctrl Pts',(374.764187962143,-3.5191798352377,-0.194963157151585));
#48980=CARTESIAN_POINT('Ctrl Pts',(374.756739445294,-3.51331973624574,-0.310721376748395));
#48981=CARTESIAN_POINT('Ctrl Pts',(374.744177451681,-3.50745963725378,-0.426012817119104));
#48982=CARTESIAN_POINT('Ctrl Pts',(374.731162249707,-3.5013881191236,-0.545463712304576));
#48983=CARTESIAN_POINT('Ctrl Pts',(374.712657608584,-3.49531660099342,-0.664413061049791));
#48984=CARTESIAN_POINT('Ctrl Pts',(374.688726111108,-3.48924508286325,-0.782320894232927));
#48985=CARTESIAN_POINT('Ctrl Pts',(374.665654491975,-3.48339171936158,-0.895992202218437));
#48986=CARTESIAN_POINT('Ctrl Pts',(374.637539376976,-3.47753835585991,-1.00869511198927));
#48987=CARTESIAN_POINT('Ctrl Pts',(374.604489288355,-3.47168499235824,-1.11995372659874));
#48988=CARTESIAN_POINT('Ctrl Pts',(374.57144416209,-3.46583250771889,-1.23119563611135));
#48989=CARTESIAN_POINT('Ctrl Pts',(374.533465653143,-3.45998002307955,-1.34099328571946));
#48990=CARTESIAN_POINT('Ctrl Pts',(374.490712459852,-3.4541275384402,-1.44888490937688));
#48991=CARTESIAN_POINT('Ctrl Pts',(374.447955346663,-3.44827451720597,-1.55678642525895));
#48992=CARTESIAN_POINT('Ctrl Pts',(374.400422831082,-3.44242149597174,-1.66278118367952));
#48993=CARTESIAN_POINT('Ctrl Pts',(374.348321893907,-3.43656847473752,-1.7664270723876));
#48994=CARTESIAN_POINT('Ctrl Pts',(374.296203580056,-3.4307135014069,-1.87010752901486));
#48995=CARTESIAN_POINT('Ctrl Pts',(374.239514000343,-3.42485852807629,-1.97143718925419));
#48996=CARTESIAN_POINT('Ctrl Pts',(374.178505902321,-3.41900355474567,-2.06999886286803));
#48997=CARTESIAN_POINT('Ctrl Pts',(374.117428659439,-3.41314194555319,-2.16867224350662));
#48998=CARTESIAN_POINT('Ctrl Pts',(374.052023346714,-3.40728033636072,-2.26457102445186));
#48999=CARTESIAN_POINT('Ctrl Pts',(373.98258588037,-3.40141872716824,-2.35730724116484));
#49000=CARTESIAN_POINT('Ctrl Pts',(373.913101591823,-3.39555316544878,-2.45010599060338));
#49001=CARTESIAN_POINT('Ctrl Pts',(373.839579997071,-3.38968760372932,-2.53973761080811));
#49002=CARTESIAN_POINT('Ctrl Pts',(373.762355963892,-3.38382204200986,-2.62584878134184));
#49003=CARTESIAN_POINT('Ctrl Pts',(373.685019010211,-3.37794790339858,-2.71208586755588));
#49004=CARTESIAN_POINT('Ctrl Pts',(373.603969101428,-3.3720737647873,-2.79479193651726));
#49005=CARTESIAN_POINT('Ctrl Pts',(373.519576478687,-3.36619962617602,-2.87365187772935));
#49006=CARTESIAN_POINT('Ctrl Pts',(373.498234948849,-3.36471415149385,-2.89359428186034));
#49007=CARTESIAN_POINT('Ctrl Pts',(373.476679806803,-3.36322867681169,-2.91329093417751));
#49008=CARTESIAN_POINT('Ctrl Pts',(373.454917343959,-3.36174320212952,-2.93273717014677));
#49009=CARTESIAN_POINT('Ctrl Pts',(373.368866770481,-3.35586951268532,-3.00962919147399));
#49010=CARTESIAN_POINT('Ctrl Pts',(373.279285834524,-3.34999582324112,-3.0828588019322));
#49011=CARTESIAN_POINT('Ctrl Pts',(373.186519367276,-3.34412213379692,-3.15208455427388));
#49012=CARTESIAN_POINT('Ctrl Pts',(373.093872670263,-3.3382560278383,-3.22122092965763));
#49013=CARTESIAN_POINT('Ctrl Pts',(372.998048949099,-3.33238992187967,-3.28636348224985));
#49014=CARTESIAN_POINT('Ctrl Pts',(372.899428344965,-3.32652381592105,-3.34720893535185));
#49015=CARTESIAN_POINT('Ctrl Pts',(372.800908727086,-3.32066371678092,-3.40799208347748));
#49016=CARTESIAN_POINT('Ctrl Pts',(372.699598272437,-3.31480361764079,-3.46448666878525));
#49017=CARTESIAN_POINT('Ctrl Pts',(372.595907991573,-3.30894351850066,-3.51643131377136));
#49018=CARTESIAN_POINT('Ctrl Pts',(372.488476803237,-3.30287200042638,-3.57025000238973));
#49019=CARTESIAN_POINT('Ctrl Pts',(372.378491191236,-3.29680048235209,-3.61918397922802));
#49020=CARTESIAN_POINT('Ctrl Pts',(372.266438822559,-3.29072896427781,-3.66299311072114));
#49021=CARTESIAN_POINT('Ctrl Pts',(372.158412583767,-3.28487560063129,-3.70522814560539));
#49022=CARTESIAN_POINT('Ctrl Pts',(372.04846597045,-3.27902223698476,-3.74270011324722));
#49023=CARTESIAN_POINT('Ctrl Pts',(371.937057713501,-3.27316887333824,-3.77524221746847));
#49024=CARTESIAN_POINT('Ctrl Pts',(371.825666184145,-3.26731638855549,-3.80777943559712));
#49025=CARTESIAN_POINT('Ctrl Pts',(371.712813843995,-3.26146390377275,-3.83538814630011));
#49026=CARTESIAN_POINT('Ctrl Pts',(371.598974750581,-3.25561141899,-3.85795137726281));
#49027=CARTESIAN_POINT('Ctrl Pts',(371.48512521967,-3.24975839761397,-3.88051667696704));
#49028=CARTESIAN_POINT('Ctrl Pts',(371.370289160928,-3.24390537623794,-3.89803549699331));
#49029=CARTESIAN_POINT('Ctrl Pts',(371.254950291026,-3.23805235486191,-3.91044209166542));
#49030=CARTESIAN_POINT('Ctrl Pts',(371.139572953405,-3.23219738139126,-3.92285282417422));
#49031=CARTESIAN_POINT('Ctrl Pts',(371.023692881719,-3.22634240792062,-3.93014789680099));
#49032=CARTESIAN_POINT('Ctrl Pts',(370.907797661072,-3.22048743444998,-3.9323135324944));
#49033=CARTESIAN_POINT('Ctrl Pts',(370.791771088114,-3.21462582512074,-3.93448162265704));
#49034=CARTESIAN_POINT('Ctrl Pts',(370.675729745229,-3.20876421579151,-3.93150866465489));
#49035=CARTESIAN_POINT('Ctrl Pts',(370.560160061085,-3.20290260646227,-3.92343299993888));
#49036=CARTESIAN_POINT('Ctrl Pts',(370.444512447474,-3.19703704460784,-3.91535188974426));
#49037=CARTESIAN_POINT('Ctrl Pts',(370.329337535343,-3.19117148275342,-3.90216126834876));
#49038=CARTESIAN_POINT('Ctrl Pts',(370.215113757659,-3.18530592089899,-3.88395098939671));
#49039=CARTESIAN_POINT('Ctrl Pts',(370.100722956831,-3.17943178215628,-3.86571408255599));
#49040=CARTESIAN_POINT('Ctrl Pts',(369.987286469281,-3.17355764341358,-3.84244295213291));
#49041=CARTESIAN_POINT('Ctrl Pts',(369.875269796099,-3.16768350467087,-3.81427789025974));
#49042=CARTESIAN_POINT('Ctrl Pts',(369.846942617182,-3.16619803135321,-3.80715540818438));
#49043=CARTESIAN_POINT('Ctrl Pts',(369.818706144067,-3.16471255803554,-3.79972020227127));
#49044=CARTESIAN_POINT('Ctrl Pts',(369.790567707011,-3.16322708471787,-3.79197503054557));
#49045=CARTESIAN_POINT('Ctrl Pts',(369.679305898748,-3.15735339503414,-3.76134995318948));
#49046=CARTESIAN_POINT('Ctrl Pts',(369.569207800241,-3.15147970535042,-3.7257728563648));
#49047=CARTESIAN_POINT('Ctrl Pts',(369.460747268587,-3.14560601566669,-3.68534840266416));
#49048=CARTESIAN_POINT('Ctrl Pts',(369.352426769633,-3.13973990946625,-3.64497614071789));
#49049=CARTESIAN_POINT('Ctrl Pts',(369.245740016573,-3.13387380326582,-3.59976911075438));
#49050=CARTESIAN_POINT('Ctrl Pts',(369.14114793337,-3.12800769706538,-3.54988233924749));
#49051=CARTESIAN_POINT('Ctrl Pts',(369.036662951102,-3.12214759768154,-3.50004665114697));
#49052=CARTESIAN_POINT('Ctrl Pts',(368.934268742962,-3.1162874982977,-3.44554092998064));
#49053=CARTESIAN_POINT('Ctrl Pts',(368.83440775927,-3.11042739891385,-3.38656885595178));
#49054=CARTESIAN_POINT('Ctrl Pts',(368.730944026211,-3.1043558809302,-3.32546920822455));
#49055=CARTESIAN_POINT('Ctrl Pts',(368.630200177461,-3.09828436294655,-3.25957500975565));
#49056=CARTESIAN_POINT('Ctrl Pts',(368.532642367994,-3.0922128449629,-3.18916587224481));
#49057=CARTESIAN_POINT('Ctrl Pts',(368.438589882107,-3.08635948106936,-3.1212865866377));
#49058=CARTESIAN_POINT('Ctrl Pts',(368.347498786021,-3.08050611717582,-3.04921149091342));
#49059=CARTESIAN_POINT('Ctrl Pts',(368.259757922272,-3.07465275328228,-2.97323563848114));
#49060=CARTESIAN_POINT('Ctrl Pts',(368.17203023252,-3.06880026825175,-2.89727119356892));
#49061=CARTESIAN_POINT('Ctrl Pts',(368.087652087142,-3.06294778322122,-2.81740742688554));
#49062=CARTESIAN_POINT('Ctrl Pts',(368.006978770004,-3.05709529819069,-2.73397928091984));
#49063=CARTESIAN_POINT('Ctrl Pts',(367.926298056214,-3.05124227656635,-2.65054348572035));
#49064=CARTESIAN_POINT('Ctrl Pts',(367.849323133129,-3.04538925494202,-2.56354295859619));
#49065=CARTESIAN_POINT('Ctrl Pts',(367.776371474784,-3.03953623331768,-2.47334852913671));
#49066=CARTESIAN_POINT('Ctrl Pts',(367.703395485661,-3.03368125959846,-2.38312401810635));
#49067=CARTESIAN_POINT('Ctrl Pts',(367.634445689133,-3.02782628587923,-2.28970380763392));
#49068=CARTESIAN_POINT('Ctrl Pts',(367.569797986701,-3.02197131216,-2.19349015066754));
#49069=CARTESIAN_POINT('Ctrl Pts',(367.505077014435,-3.01610970258316,-2.0971674479294));
#49070=CARTESIAN_POINT('Ctrl Pts',(367.444668098752,-3.01024809300633,-1.99804532264505));
#49071=CARTESIAN_POINT('Ctrl Pts',(367.388802718651,-3.00438648342949,-1.89655330993627));
#49072=CARTESIAN_POINT('Ctrl Pts',(367.332899668128,-2.99852092132768,-1.79499286044245));
#49073=CARTESIAN_POINT('Ctrl Pts',(367.281546436331,-2.99265535922588,-1.69105971096975));
#49074=CARTESIAN_POINT('Ctrl Pts',(367.234926881615,-2.98678979712407,-1.58520460303999));
#49075=CARTESIAN_POINT('Ctrl Pts',(367.188239157711,-2.98091565813626,-1.4791947090595));
#49076=CARTESIAN_POINT('Ctrl Pts',(367.146299074105,-2.97504151914846,-1.37125763143878));
#49077=CARTESIAN_POINT('Ctrl Pts',(367.109241094803,-2.96916738016065,-1.26186058812891));
#49078=CARTESIAN_POINT('Ctrl Pts',(367.099869755125,-2.96768190920917,-1.23419591585064));
#49079=CARTESIAN_POINT('Ctrl Pts',(367.090810371226,-2.96619643825769,-1.20643793410368));
#49080=CARTESIAN_POINT('Ctrl Pts',(367.082064599313,-2.96471096730621,-1.17859429767576));
#49081=CARTESIAN_POINT('Ctrl Pts',(367.040187967712,-2.95759821380612,-1.04527299491962));
#49082=CARTESIAN_POINT('Ctrl Pts',(367.005392554132,-2.95048546030604,-0.909628073109617));
#49083=CARTESIAN_POINT('Ctrl Pts',(366.977897824696,-2.94337270680596,-0.772342905429096));
#49084=CARTESIAN_POINT('Ctrl Pts',(366.950733234797,-2.93634535880723,-0.636706172292929));
#49085=CARTESIAN_POINT('Ctrl Pts',(366.930695083428,-2.92931801080851,-0.49946836452728));
#49086=CARTESIAN_POINT('Ctrl Pts',(366.917949055783,-2.92229066280978,-0.36130934450515));
#49087=CARTESIAN_POINT('Ctrl Pts',(366.906989537955,-2.91624828256271,-0.242514980872078));
#49088=CARTESIAN_POINT('Ctrl Pts',(366.901420577048,-2.91020590231564,-0.12303987234602));
#49089=CARTESIAN_POINT('Ctrl Pts',(366.901319261778,-2.90416352206856,-0.00332861608662543));
#49090=CARTESIAN_POINT('',(366.901318397982,-1.65416352199376,0.00207004085040813));
#49091=CARTESIAN_POINT('Ctrl Pts',(366.901319261778,-2.90416352203497,-0.00332861542100308));
#49092=CARTESIAN_POINT('Ctrl Pts',(366.901221605676,-2.89833937116086,0.112059094269534));
#49093=CARTESIAN_POINT('Ctrl Pts',(366.90620615245,-2.89251522028675,0.227532235631285));
#49094=CARTESIAN_POINT('Ctrl Pts',(366.916268663384,-2.88669106941264,0.342606984741543));
#49095=CARTESIAN_POINT('Ctrl Pts',(366.926328011892,-2.88086874894105,0.457645568389189));
#49096=CARTESIAN_POINT('Ctrl Pts',(366.941462116302,-2.87504642846945,0.572285592939777));
#49097=CARTESIAN_POINT('Ctrl Pts',(366.961614702161,-2.86922410799786,0.686046138208073));
#49098=CARTESIAN_POINT('Ctrl Pts',(366.981765953168,-2.86340217318109,0.799799148284504));
#49099=CARTESIAN_POINT('Ctrl Pts',(367.006934951835,-2.85758023836431,0.912672383610354));
#49100=CARTESIAN_POINT('Ctrl Pts',(367.037014036022,-2.85175830354753,1.02419369255015));
#49101=CARTESIAN_POINT('Ctrl Pts',(367.067098588865,-2.84593531024896,1.13573527709911));
#49102=CARTESIAN_POINT('Ctrl Pts',(367.102094892846,-2.84011231695039,1.2459240434281));
#49103=CARTESIAN_POINT('Ctrl Pts',(367.141845223444,-2.83428932365182,1.35430235853338));
#49104=CARTESIAN_POINT('Ctrl Pts',(367.18163849359,-2.82846004017431,1.46279774727414));
#49105=CARTESIAN_POINT('Ctrl Pts',(367.226195902583,-2.82263075669681,1.56947838606366));
#49106=CARTESIAN_POINT('Ctrl Pts',(367.275311231093,-2.8168014732193,1.67390587060044));
#49107=CARTESIAN_POINT('Ctrl Pts',(367.32445349731,-2.81096899262337,1.77839062924911));
#49108=CARTESIAN_POINT('Ctrl Pts',(367.378158467062,-2.80513651202745,1.88061940309016));
#49109=CARTESIAN_POINT('Ctrl Pts',(367.436174443088,-2.79930403143153,1.98017937676107));
#49110=CARTESIAN_POINT('Ctrl Pts',(367.494288052215,-2.79346173555352,2.07990689650603));
#49111=CARTESIAN_POINT('Ctrl Pts',(367.556726934978,-2.78761943967551,2.17695629228589));
#49112=CARTESIAN_POINT('Ctrl Pts',(367.623196376333,-2.7817771437975,2.27094426630184));
#49113=CARTESIAN_POINT('Ctrl Pts',(367.682291087978,-2.77658304582985,2.35450435209916));
#49114=CARTESIAN_POINT('Ctrl Pts',(367.744570876838,-2.7713889478622,2.43564496159557));
#49115=CARTESIAN_POINT('Ctrl Pts',(367.809803658402,-2.76619484989455,2.51412069823983));
#49116=CARTESIAN_POINT('Ctrl Pts',(367.883571451695,-2.76032115976456,2.60286414563765));
#49117=CARTESIAN_POINT('Ctrl Pts',(367.961371198811,-2.75444746963457,2.68850596907481));
#49118=CARTESIAN_POINT('Ctrl Pts',(368.042912203698,-2.74857377950458,2.77065759338757));
#49119=CARTESIAN_POINT('Ctrl Pts',(368.124347931416,-2.74270767286554,2.85270315216294));
#49120=CARTESIAN_POINT('Ctrl Pts',(368.209515022598,-2.73684156622651,2.93126718257746));
#49121=CARTESIAN_POINT('Ctrl Pts',(368.298082227265,-2.73097545958748,3.00599365428754));
#49122=CARTESIAN_POINT('Ctrl Pts',(368.38655874015,-2.72511535977305,3.08064360696428));
#49123=CARTESIAN_POINT('Ctrl Pts',(368.478428127287,-2.71925525995863,3.15146355242979));
#49124=CARTESIAN_POINT('Ctrl Pts',(368.573322426838,-2.71339516014421,3.21813434801291));
#49125=CARTESIAN_POINT('Ctrl Pts',(368.67164027959,-2.70732364232499,3.28721046211055));
#49126=CARTESIAN_POINT('Ctrl Pts',(368.77320511027,-2.70125212450577,3.35183207103601));
#49127=CARTESIAN_POINT('Ctrl Pts',(368.877570005795,-2.69518060668655,3.4116897370047));
#49128=CARTESIAN_POINT('Ctrl Pts',(368.978185003889,-2.68932724238497,3.46939667875951));
#49129=CARTESIAN_POINT('Ctrl Pts',(369.081401924361,-2.68347387808339,3.52267590578454));
#49130=CARTESIAN_POINT('Ctrl Pts',(369.186791656259,-2.67762051378181,3.57129478345251));
#49131=CARTESIAN_POINT('Ctrl Pts',(369.292165564081,-2.6717680283522,3.6199063610847));
#49132=CARTESIAN_POINT('Ctrl Pts',(369.399711259585,-2.66591554292259,3.66385880769255));
#49133=CARTESIAN_POINT('Ctrl Pts',(369.508977123804,-2.66006305749298,3.70296650686193));
#49134=CARTESIAN_POINT('Ctrl Pts',(369.618253006051,-2.65421003547893,3.74207779161616));
#49135=CARTESIAN_POINT('Ctrl Pts',(369.729248981531,-2.64835701346487,3.77634330669451));
#49136=CARTESIAN_POINT('Ctrl Pts',(369.841496321851,-2.64250399145082,3.80562667728218));
#49137=CARTESIAN_POINT('Ctrl Pts',(369.95378109862,-2.63664901735164,3.83491981438564));
#49138=CARTESIAN_POINT('Ctrl Pts',(370.067317670567,-2.63079404325247,3.85922739868144));
#49139=CARTESIAN_POINT('Ctrl Pts',(370.181625817804,-2.62493906915329,3.87846388495488));
#49140=CARTESIAN_POINT('Ctrl Pts',(370.296063518259,-2.61907745921268,3.89772217325005));
#49141=CARTESIAN_POINT('Ctrl Pts',(370.411274131767,-2.61321584927208,3.91189782341532));
#49142=CARTESIAN_POINT('Ctrl Pts',(370.526770894742,-2.60735423933147,3.92095700924261));
#49143=CARTESIAN_POINT('Ctrl Pts',(370.642345537823,-2.60148867687489,3.93002230372895));
#49144=CARTESIAN_POINT('Ctrl Pts',(370.758206302698,-2.59562311441832,3.9339642500285));
#49145=CARTESIAN_POINT('Ctrl Pts',(370.873866735968,-2.58975755196174,3.93280115005497));
#49146=CARTESIAN_POINT('Ctrl Pts',(370.98969629275,-2.58388341263499,3.93163634934813));
#49147=CARTESIAN_POINT('Ctrl Pts',(371.105324522356,-2.57800927330824,3.92535162681694));
#49148=CARTESIAN_POINT('Ctrl Pts',(371.220270322131,-2.57213513398149,3.91401707862201));
#49149=CARTESIAN_POINT('Ctrl Pts',(371.249338105845,-2.5706496668153,3.91115076949131));
#49150=CARTESIAN_POINT('Ctrl Pts',(371.278362303016,-2.5691641996491,3.90796178063672));
#49151=CARTESIAN_POINT('Ctrl Pts',(371.307335256849,-2.5676787324829,3.90445175868106));
#49152=CARTESIAN_POINT('Ctrl Pts',(371.421897327312,-2.56180504093109,3.89057276709056));
#49153=CARTESIAN_POINT('Ctrl Pts',(371.536038838117,-2.55593134937928,3.87162427043913));
#49154=CARTESIAN_POINT('Ctrl Pts',(371.649275677197,-2.55005765782746,3.84763989286235));
#49155=CARTESIAN_POINT('Ctrl Pts',(371.762366317211,-2.54419154974604,3.82368648129995));
#49156=CARTESIAN_POINT('Ctrl Pts',(371.874554207809,-2.53832544166461,3.79471020354817));
#49157=CARTESIAN_POINT('Ctrl Pts',(371.985360599952,-2.53245933358318,3.76079640438102));
#49158=CARTESIAN_POINT('Ctrl Pts',(372.096053528024,-2.52659923230772,3.72691733243144));
#49159=CARTESIAN_POINT('Ctrl Pts',(372.205367378757,-2.52073913103227,3.68811091595824));
#49160=CARTESIAN_POINT('Ctrl Pts',(372.312834498288,-2.51487902975682,3.64451334615041));
#49161=CARTESIAN_POINT('Ctrl Pts',(372.424178729803,-2.50880751247825,3.59934289841421));
#49162=CARTESIAN_POINT('Ctrl Pts',(372.533540022709,-2.50273599519969,3.5490291612744));
#49163=CARTESIAN_POINT('Ctrl Pts',(372.640416078535,-2.49666447792112,3.4937799301799));
#49164=CARTESIAN_POINT('Ctrl Pts',(372.743452044873,-2.49081111212182,3.4405158209155));
#49165=CARTESIAN_POINT('Ctrl Pts',(372.844177892854,-2.48495774632252,3.38266498762702));
#49166=CARTESIAN_POINT('Ctrl Pts',(372.942165512519,-2.47910438052322,3.32046190238743));
#49167=CARTESIAN_POINT('Ctrl Pts',(373.040138419707,-2.47325189358497,3.25826815670921));
#49168=CARTESIAN_POINT('Ctrl Pts',(373.135373567362,-2.46739940664672,3.19172367979328));
#49169=CARTESIAN_POINT('Ctrl Pts',(373.227470153504,-2.46154691970847,3.12110734638631));
#49170=CARTESIAN_POINT('Ctrl Pts',(373.319575183653,-2.45569389617654,3.05048453841917));
#49171=CARTESIAN_POINT('Ctrl Pts',(373.408540752363,-2.4498408726446,2.97578938321193));
#49172=CARTESIAN_POINT('Ctrl Pts',(373.493998160584,-2.44398784911266,2.89734182702733));
#49173=CARTESIAN_POINT('Ctrl Pts',(373.579484070446,-2.43813287348808,2.81886810711782));
#49174=CARTESIAN_POINT('Ctrl Pts',(373.661459189062,-2.4322778978635,2.73663977692442));
#49175=CARTESIAN_POINT('Ctrl Pts',(373.739591300248,-2.42642292223891,2.65101399430834));
#49176=CARTESIAN_POINT('Ctrl Pts',(373.817811963905,-2.42056131076958,2.56529116613026));
#49177=CARTESIAN_POINT('Ctrl Pts',(373.892180648096,-2.41469969930025,2.4761635053898));
#49178=CARTESIAN_POINT('Ctrl Pts',(373.962405049128,-2.40883808783092,2.38402170602979));
#49179=CARTESIAN_POINT('Ctrl Pts',(374.032676802894,-2.40297252384184,2.29181777490229));
#49180=CARTESIAN_POINT('Ctrl Pts',(374.098798473939,-2.39710695985277,2.19659599660529));
#49181=CARTESIAN_POINT('Ctrl Pts',(374.160521730394,-2.39124139586369,2.09877506357777));
#49182=CARTESIAN_POINT('Ctrl Pts',(374.22233524108,-2.38536725501087,2.00081109284468));
#49183=CARTESIAN_POINT('Ctrl Pts',(374.279737297431,-2.37949311415804,1.90024073979457));
#49184=CARTESIAN_POINT('Ctrl Pts',(374.332525991379,-2.37361897330521,1.79750627875001));
#49185=CARTESIAN_POINT('Ctrl Pts',(374.345875196357,-2.37213352056056,1.77152678813974));
#49186=CARTESIAN_POINT('Ctrl Pts',(374.358929628063,-2.3706480678159,1.74540899861485));
#49187=CARTESIAN_POINT('Ctrl Pts',(374.371686519428,-2.36916261507124,1.71916023667212));
#49188=CARTESIAN_POINT('Ctrl Pts',(374.422128995786,-2.36328893371683,1.61536907660059));
#49189=CARTESIAN_POINT('Ctrl Pts',(374.468083555297,-2.35741525236242,1.50918309354284));
#49190=CARTESIAN_POINT('Ctrl Pts',(374.509316010673,-2.35154157100801,1.40102731691575));
#49191=CARTESIAN_POINT('Ctrl Pts',(374.550495230961,-2.34567547314448,1.29301117985996));
#49192=CARTESIAN_POINT('Ctrl Pts',(374.58696432561,-2.33980937528096,1.18303068933183));
#49193=CARTESIAN_POINT('Ctrl Pts',(374.618535475887,-2.33394327741743,1.07153440650688));
#49194=CARTESIAN_POINT('Ctrl Pts',(374.650074297681,-2.32808318636828,0.960152294548065));
#49195=CARTESIAN_POINT('Ctrl Pts',(374.676725039331,-2.32222309531912,0.847257872808208));
#49196=CARTESIAN_POINT('Ctrl Pts',(374.698348623511,-2.31636300426997,0.733317943509966));
#49197=CARTESIAN_POINT('Ctrl Pts',(374.720752379135,-2.3102914831612,0.615267100944081));
#49198=CARTESIAN_POINT('Ctrl Pts',(374.737759210823,-2.30421996205244,0.496094305290207));
#49199=CARTESIAN_POINT('Ctrl Pts',(374.749271429024,-2.29814844094367,0.376334291991625));
#49200=CARTESIAN_POINT('Ctrl Pts',(374.760369983383,-2.29229508532721,0.260877566418002));
#49201=CARTESIAN_POINT('Ctrl Pts',(374.766361956726,-2.28644172971074,0.144875543911012));
#49202=CARTESIAN_POINT('Ctrl Pts',(374.767212295152,-2.28058837409428,0.0288150767852721));
#49203=CARTESIAN_POINT('Ctrl Pts',(374.768062505908,-2.27473589730551,-0.0872279649249877));
#49204=CARTESIAN_POINT('Ctrl Pts',(374.763772613688,-2.26888342051675,-0.203329020781968));
#49205=CARTESIAN_POINT('Ctrl Pts',(374.754359680422,-2.26303094372798,-0.319000114451182));
#49206=CARTESIAN_POINT('Ctrl Pts',(374.744945884045,-2.25717793030141,-0.434681814481509));
#49207=CARTESIAN_POINT('Ctrl Pts',(374.73040814631,-2.25132491687484,-0.549933062143207));
#49208=CARTESIAN_POINT('Ctrl Pts',(374.710815445168,-2.24547190344827,-0.664270592191428));
#49209=CARTESIAN_POINT('Ctrl Pts',(374.6912162093,-2.23961693787405,-0.778646257081286));
#49210=CARTESIAN_POINT('Ctrl Pts',(374.66655872728,-2.23376197229983,-0.89210719138289));
#49211=CARTESIAN_POINT('Ctrl Pts',(374.636963023964,-2.22790700672561,-1.00418061395693));
#49212=CARTESIAN_POINT('Ctrl Pts',(374.607333777087,-2.22204540517478,-1.1163810597563));
#49213=CARTESIAN_POINT('Ctrl Pts',(374.572755243293,-2.21618380362394,-1.22719045534492));
#49214=CARTESIAN_POINT('Ctrl Pts',(374.533397265,-2.21032220207311,-1.33615137816496));
#49215=CARTESIAN_POINT('Ctrl Pts',(374.494012746907,-2.20445664793774,-1.44518577531713));
#49216=CARTESIAN_POINT('Ctrl Pts',(374.449842523899,-2.19859109380236,-1.55236883668829));
#49217=CARTESIAN_POINT('Ctrl Pts',(374.401103803266,-2.19272553966699,-1.65726491140704));
#49218=CARTESIAN_POINT('Ctrl Pts',(374.352293813378,-2.18685140849739,-1.76231437269449));
#49219=CARTESIAN_POINT('Ctrl Pts',(374.298902183255,-2.1809772773278,-1.86506980795421));
#49220=CARTESIAN_POINT('Ctrl Pts',(374.241191102975,-2.1751031461582,-1.96512179269728));
#49221=CARTESIAN_POINT('Ctrl Pts',(374.226596150299,-2.17361759665866,-1.99042462839697));
#49222=CARTESIAN_POINT('Ctrl Pts',(374.211725148619,-2.17213204715913,-2.01555471456537));
#49223=CARTESIAN_POINT('Ctrl Pts',(374.196582755325,-2.17064649765959,-2.04050575301744));
#49224=CARTESIAN_POINT('Ctrl Pts',(374.136711409584,-2.16477279949461,-2.13915939519895));
#49225=CARTESIAN_POINT('Ctrl Pts',(374.072394712155,-2.15889910132964,-2.23534004402309));
#49226=CARTESIAN_POINT('Ctrl Pts',(374.003862865492,-2.15302540316466,-2.32862049617492));
#49227=CARTESIAN_POINT('Ctrl Pts',(373.935419500314,-2.14715928853291,-2.42178051391063));
#49228=CARTESIAN_POINT('Ctrl Pts',(373.862772050991,-2.14129317390117,-2.51204745154188));
#49229=CARTESIAN_POINT('Ctrl Pts',(373.786195630664,-2.13542705926942,-2.59902031293644));
#49230=CARTESIAN_POINT('Ctrl Pts',(373.709697624255,-2.12956695151328,-2.6859041145032));
#49231=CARTESIAN_POINT('Ctrl Pts',(373.629278920811,-2.12370684375713,-2.76950024100981));
#49232=CARTESIAN_POINT('Ctrl Pts',(373.545256384692,-2.11784673600099,-2.8494387655473));
#49233=CARTESIAN_POINT('Ctrl Pts',(373.458202682824,-2.11177522117794,-2.93226112255134));
#49234=CARTESIAN_POINT('Ctrl Pts',(373.367280485604,-2.1057037063549,-3.01115663072952));
#49235=CARTESIAN_POINT('Ctrl Pts',(373.2728861744,-2.09963219153185,-3.08575331855246));
#49236=CARTESIAN_POINT('Ctrl Pts',(373.181883345503,-2.09377881946382,-3.1576698305922));
#49237=CARTESIAN_POINT('Ctrl Pts',(373.08765395933,-2.08792544739578,-3.22559083191305));
#49238=CARTESIAN_POINT('Ctrl Pts',(372.990588120366,-2.08207207532774,-3.28922293787454));
#49239=CARTESIAN_POINT('Ctrl Pts',(372.893536856928,-2.07621958220929,-3.35284548876038));
#49240=CARTESIAN_POINT('Ctrl Pts',(372.793650333023,-2.07036708909084,-3.41218019840676));
#49241=CARTESIAN_POINT('Ctrl Pts',(372.691347850167,-2.06451459597238,-3.46697686615502));
#49242=CARTESIAN_POINT('Ctrl Pts',(372.589035989226,-2.05866156635498,-3.52177855712227));
#49243=CARTESIAN_POINT('Ctrl Pts',(372.48430809328,-2.05280853673758,-3.5720411841332));
#49244=CARTESIAN_POINT('Ctrl Pts',(372.377607649301,-2.04695550712018,-3.61756072586551));
#49245=CARTESIAN_POINT('Ctrl Pts',(372.270871620611,-2.0411005255112,-3.6630954484132));
#49246=CARTESIAN_POINT('Ctrl Pts',(372.162162115591,-2.03524554390222,-3.70388377826776));
#49247=CARTESIAN_POINT('Ctrl Pts',(372.051941484438,-2.02939056229325,-3.73977027271838));
#49248=CARTESIAN_POINT('Ctrl Pts',(371.941595936191,-2.02352894501829,-3.77569743865288));
#49249=CARTESIAN_POINT('Ctrl Pts',(371.829736236601,-2.01766732774334,-3.80671155290144));
#49250=CARTESIAN_POINT('Ctrl Pts',(371.716838836597,-2.01180571046839,-3.83270736084911));
#49251=CARTESIAN_POINT('Ctrl Pts',(371.603865311144,-2.00594014077078,-3.85872069747794));
#49252=CARTESIAN_POINT('Ctrl Pts',(371.48985309731,-2.00007457107318,-3.87970891532077));
#49253=CARTESIAN_POINT('Ctrl Pts',(371.375286028223,-1.99420900137557,-3.89561836344863));
#49254=CARTESIAN_POINT('Ctrl Pts',(371.260551438335,-1.98833485499935,-3.91155107448708));
#49255=CARTESIAN_POINT('Ctrl Pts',(371.145260783764,-1.98246070862314,-3.9223901564312));
#49256=CARTESIAN_POINT('Ctrl Pts',(371.029900245164,-1.97658656224692,-3.92813397530723));
#49257=CARTESIAN_POINT('Ctrl Pts',(371.000729053154,-1.97510116824726,-3.92958641342286));
#49258=CARTESIAN_POINT('Ctrl Pts',(370.971553376122,-1.9736157742476,-3.93071330423033));
#49259=CARTESIAN_POINT('Ctrl Pts',(370.942381028825,-1.97213038024793,-3.93151514687137));
#49260=CARTESIAN_POINT('Ctrl Pts',(370.827024605462,-1.96625667603962,-3.93468587901123));
#49261=CARTESIAN_POINT('Ctrl Pts',(370.711336395662,-1.96038297183131,-3.93278049909418));
#49262=CARTESIAN_POINT('Ctrl Pts',(370.595800177937,-1.954509267623,-3.92576085855667));
#49263=CARTESIAN_POINT('Ctrl Pts',(370.480413125292,-1.94864314676452,-3.91875028085039));
#49264=CARTESIAN_POINT('Ctrl Pts',(370.365178083096,-1.94277702590605,-3.90663859826885));
#49265=CARTESIAN_POINT('Ctrl Pts',(370.250581154075,-1.93691090504757,-3.8894396082298));
#49266=CARTESIAN_POINT('Ctrl Pts',(370.136101568291,-1.93105079089115,-3.87225822935343));
#49267=CARTESIAN_POINT('Ctrl Pts',(370.022259202141,-1.92519067673472,-3.84999996555435));
#49268=CARTESIAN_POINT('Ctrl Pts',(369.909536684186,-1.9193305625783,-3.82273054103916));
#49269=CARTESIAN_POINT('Ctrl Pts',(369.792747803064,-1.91325905008905,-3.79447739662947));
#49270=CARTESIAN_POINT('Ctrl Pts',(369.6771615413,-1.9071875375998,-3.76084474719226));
#49271=CARTESIAN_POINT('Ctrl Pts',(369.563305350035,-1.90111602511055,-3.72196402679242));
#49272=CARTESIAN_POINT('Ctrl Pts',(369.45353971524,-1.89526264625483,-3.68448018943125));
#49273=CARTESIAN_POINT('Ctrl Pts',(369.345382400785,-1.88940926739911,-3.64211903594313));
#49274=CARTESIAN_POINT('Ctrl Pts',(369.239291420052,-1.8835558885434,-3.59504932893611));
#49275=CARTESIAN_POINT('Ctrl Pts',(369.133216367688,-1.87770338850668,-3.54798668891616));
#49276=CARTESIAN_POINT('Ctrl Pts',(369.02920740972,-1.87185088846996,-3.49621706853729));
#49277=CARTESIAN_POINT('Ctrl Pts',(368.927702099564,-1.86599838843324,-3.43995717529977));
#49278=CARTESIAN_POINT('Ctrl Pts',(368.826187482287,-1.8601453517751,-3.38369212353793));
#49279=CARTESIAN_POINT('Ctrl Pts',(368.72717733054,-1.85429231511697,-3.32293618075318));
#49280=CARTESIAN_POINT('Ctrl Pts',(368.631083503943,-1.84843927845883,-3.25795141187662));
#49281=CARTESIAN_POINT('Ctrl Pts',(368.534957628112,-1.84258428969461,-3.19294496926558));
#49282=CARTESIAN_POINT('Ctrl Pts',(368.441750353557,-1.83672930093039,-3.12370712736096));
#49283=CARTESIAN_POINT('Ctrl Pts',(368.351842944765,-1.83087431216617,-3.05054213687864));
#49284=CARTESIAN_POINT('Ctrl Pts',(368.261833638707,-1.82501268760456,-2.977294224281));
#49285=CARTESIAN_POINT('Ctrl Pts',(368.175131983708,-1.81915106304294,-2.90011054036536));
#49286=CARTESIAN_POINT('Ctrl Pts',(368.09208471489,-1.81328943848132,-2.81933439219659));
#49287=CARTESIAN_POINT('Ctrl Pts',(368.008981447091,-1.80742386141163,-2.73850377646946));
#49288=CARTESIAN_POINT('Ctrl Pts',(367.929537754586,-1.80155828434194,-2.65407617307459));
#49289=CARTESIAN_POINT('Ctrl Pts',(367.854061011427,-1.79569270727225,-2.5664290671904));
#49290=CARTESIAN_POINT('Ctrl Pts',(367.778473904908,-1.78981855345736,-2.47865380223767));
#49291=CARTESIAN_POINT('Ctrl Pts',(367.706865578653,-1.78394439964248,-2.38764996301879));
#49292=CARTESIAN_POINT('Ctrl Pts',(367.639500969047,-1.7780702458276,-2.29382520619512));
#49293=CARTESIAN_POINT('Ctrl Pts',(367.622467278517,-1.77658491816383,-2.27010085180318));
#49294=CARTESIAN_POINT('Ctrl Pts',(367.605704692428,-1.77509959050005,-2.24619626268826));
#49295=CARTESIAN_POINT('Ctrl Pts',(367.589217027284,-1.77361426283628,-2.22211827531365));
#49296=CARTESIAN_POINT('Ctrl Pts',(367.523092229448,-1.76765726464239,-2.12555202208811));
#49297=CARTESIAN_POINT('Ctrl Pts',(367.461176617048,-1.76170026644851,-2.02587883354736));
#49298=CARTESIAN_POINT('Ctrl Pts',(367.403770540428,-1.75574326825462,-1.92349529104395));
#49299=CARTESIAN_POINT('Ctrl Pts',(367.346443934608,-1.74979451670351,-1.82125348444072));
#49300=CARTESIAN_POINT('Ctrl Pts',(367.293614638098,-1.74384576515241,-1.71630913170595));
#49301=CARTESIAN_POINT('Ctrl Pts',(367.245540626912,-1.7378970136013,-1.60908887880941));
#49302=CARTESIAN_POINT('Ctrl Pts',(367.197522718397,-1.73195520428017,-1.50199375261339));
#49303=CARTESIAN_POINT('Ctrl Pts',(367.15424921483,-1.72601339495904,-1.39262837160822));
#49304=CARTESIAN_POINT('Ctrl Pts',(367.115932659183,-1.72007158563791,-1.28144471154241));
#49305=CARTESIAN_POINT('Ctrl Pts',(367.077658873099,-1.71413640866083,-1.17038515648355));
#49306=CARTESIAN_POINT('Ctrl Pts',(367.044331144165,-1.70820123168376,-1.05751173899592));
#49307=CARTESIAN_POINT('Ctrl Pts',(367.016113989028,-1.70226605470669,-0.943296481198009));
#49308=CARTESIAN_POINT('Ctrl Pts',(366.987915424115,-1.69633478798449,-0.829156471496444));
#49309=CARTESIAN_POINT('Ctrl Pts',(366.964820828366,-1.6904035212623,-0.713676765600365));
#49310=CARTESIAN_POINT('Ctrl Pts',(366.946944887028,-1.6844722545401,-0.59734447489317));
#49311=CARTESIAN_POINT('Ctrl Pts',(366.929076286795,-1.67854342360909,-0.481059958326177));
#49312=CARTESIAN_POINT('Ctrl Pts',(366.916422137311,-1.67261459267808,-0.363923946200259));
#49313=CARTESIAN_POINT('Ctrl Pts',(366.909045930346,-1.66668576174707,-0.246433219083321));
#49314=CARTESIAN_POINT('Ctrl Pts',(366.903852853057,-1.66251168184304,-0.163716122125167));
#49315=CARTESIAN_POINT('Ctrl Pts',(366.90127476899,-1.658337601939,-0.0808234308795856));
#49316=CARTESIAN_POINT('Ctrl Pts',(366.901318397982,-1.65416352203497,0.00207004003203127));
#49317=CARTESIAN_POINT('Ctrl Pts',(366.901318397982,-1.65416352199376,0.0020700408504056));
#49318=CARTESIAN_POINT('Ctrl Pts',(366.901387266335,-1.647574740613,0.132917310256408));
#49319=CARTESIAN_POINT('Ctrl Pts',(366.907990299073,-1.64098595923224,0.263537049001877));
#49320=CARTESIAN_POINT('Ctrl Pts',(366.921033153443,-1.63439717785148,0.393308858862064));
#49321=CARTESIAN_POINT('Ctrl Pts',(366.93390211787,-1.62789623942197,0.521350524996328));
#49322=CARTESIAN_POINT('Ctrl Pts',(366.953040076547,-1.62139530099246,0.64856652162196));
#49323=CARTESIAN_POINT('Ctrl Pts',(366.978305822652,-1.61489436256295,0.774377311187052));
#49324=CARTESIAN_POINT('Ctrl Pts',(367.004083668139,-1.60826165970656,0.902738099765647));
#49325=CARTESIAN_POINT('Ctrl Pts',(367.036240232741,-1.60162895685017,1.02963583952188));
#49326=CARTESIAN_POINT('Ctrl Pts',(367.074573994238,-1.59499625399378,1.15447612137308));
#49327=CARTESIAN_POINT('Ctrl Pts',(367.112907755736,-1.58836355113739,1.27931640322429));
#49328=CARTESIAN_POINT('Ctrl Pts',(367.157418544267,-1.581730848281,1.40209900418968));
#49329=CARTESIAN_POINT('Ctrl Pts',(367.207855253712,-1.57509814542462,1.52225425417008));
#49330=CARTESIAN_POINT('Ctrl Pts',(367.252520967112,-1.56922436007833,1.62866127433904));
#49331=CARTESIAN_POINT('Ctrl Pts',(367.301948294204,-1.56335057473204,1.73327796658719));
#49332=CARTESIAN_POINT('Ctrl Pts',(367.355972554108,-1.55747678938575,1.83564783662771));
#49333=CARTESIAN_POINT('Ctrl Pts',(367.409927061389,-1.55161058789037,1.93788553332751));
#49334=CARTESIAN_POINT('Ctrl Pts',(367.468466507126,-1.54574438639499,2.03788181482829));
#49335=CARTESIAN_POINT('Ctrl Pts',(367.531377925647,-1.53987818489961,2.13519948361255));
#49336=CARTESIAN_POINT('Ctrl Pts',(367.594224919664,-1.53401799069406,2.23241749413557));
#49337=CARTESIAN_POINT('Ctrl Pts',(367.661434758137,-1.5281577964885,2.32696200318616));
#49338=CARTESIAN_POINT('Ctrl Pts',(367.732748598351,-1.52229760228294,2.41842038471899));
#49339=CARTESIAN_POINT('Ctrl Pts',(367.806633643905,-1.51622612002169,2.51317627874593));
#49340=CARTESIAN_POINT('Ctrl Pts',(367.884924002244,-1.51015463776044,2.60461890741811));
#49341=CARTESIAN_POINT('Ctrl Pts',(367.967282504934,-1.5040831554992,2.69232191828074));
#49342=CARTESIAN_POINT('Ctrl Pts',(368.046683535811,-1.49822969854276,2.77687553747036));
#49343=CARTESIAN_POINT('Ctrl Pts',(368.12986525722,-1.49237624158632,2.85795316988102));
#49344=CARTESIAN_POINT('Ctrl Pts',(368.216485098508,-1.48652278462989,2.93520709121813));
#49345=CARTESIAN_POINT('Ctrl Pts',(368.303091922414,-1.48067020734126,3.01244940270004));
#49346=CARTESIAN_POINT('Ctrl Pts',(368.393135530594,-1.47481763005263,3.08586887078945));
#49347=CARTESIAN_POINT('Ctrl Pts',(368.486238104937,-1.468965052764,3.15515617611592));
#49348=CARTESIAN_POINT('Ctrl Pts',(368.57934920107,-1.46311193978194,3.2244498233928));
#49349=CARTESIAN_POINT('Ctrl Pts',(368.675519488519,-1.45725882679987,3.28961030937691));
#49350=CARTESIAN_POINT('Ctrl Pts',(368.774340416498,-1.4514057138178,3.35037042133874));
#49351=CARTESIAN_POINT('Ctrl Pts',(368.873194285809,-1.44555064973755,3.41115078729947));
#49352=CARTESIAN_POINT('Ctrl Pts',(368.974700200859,-1.43969558565731,3.46752764622947));
#49353=CARTESIAN_POINT('Ctrl Pts',(369.07842378813,-1.43384052157706,3.51927905005661));
#49354=CARTESIAN_POINT('Ctrl Pts',(369.182264896829,-1.42797882356225,3.57108908952324));
#49355=CARTESIAN_POINT('Ctrl Pts',(369.288328323026,-1.42211712554744,3.61826302910341));
#49356=CARTESIAN_POINT('Ctrl Pts',(369.396158343451,-1.41625542753262,3.66062647977775));
#49357=CARTESIAN_POINT('Ctrl Pts',(369.504061054693,-1.41038977800583,3.70301848867573));
#49358=CARTESIAN_POINT('Ctrl Pts',(369.613732341657,-1.40452412847904,3.74059341782054));
#49359=CARTESIAN_POINT('Ctrl Pts',(369.724701567165,-1.39865847895225,3.77322682828817));
#49360=CARTESIAN_POINT('Ctrl Pts',(369.835833013767,-1.39278425468705,3.80590794412192));
#49361=CARTESIAN_POINT('Ctrl Pts',(369.948265786073,-1.38691003042185,3.83363302586876));
#49362=CARTESIAN_POINT('Ctrl Pts',(370.061519251664,-1.38103580615665,3.85632873617203));
#49363=CARTESIAN_POINT('Ctrl Pts',(370.090141800331,-1.37955121344209,3.86206462309885));
#49364=CARTESIAN_POINT('Ctrl Pts',(370.118816746645,-1.37806662072753,3.86747953073522));
#49365=CARTESIAN_POINT('Ctrl Pts',(370.147536300447,-1.37658202801298,3.87257280096382));
#49366=CARTESIAN_POINT('Ctrl Pts',(370.261164980889,-1.37070824904298,3.89272428309351));
#49367=CARTESIAN_POINT('Ctrl Pts',(370.375870526143,-1.36483447007299,3.90790395514502));
#49368=CARTESIAN_POINT('Ctrl Pts',(370.491180061432,-1.35896069110299,3.91800273811087));
#49369=CARTESIAN_POINT('Ctrl Pts',(370.606340747741,-1.35309449438551,3.92808848491671));
#49370=CARTESIAN_POINT('Ctrl Pts',(370.722103465781,-1.34722829766803,3.93310635011528));
#49371=CARTESIAN_POINT('Ctrl Pts',(370.837985381494,-1.34136210095055,3.93299829001188));
#49372=CARTESIAN_POINT('Ctrl Pts',(370.953748659356,-1.33550190994133,3.9328903405385));
#49373=CARTESIAN_POINT('Ctrl Pts',(371.069630481483,-1.3296417189321,3.92766690452695));
#49374=CARTESIAN_POINT('Ctrl Pts',(371.185143792175,-1.32378152792287,3.91732180967547));
#49375=CARTESIAN_POINT('Ctrl Pts',(371.304822011351,-1.3177100438678,3.90660371561675));
#49376=CARTESIAN_POINT('Ctrl Pts',(371.424104193896,-1.31163855981274,3.89038762477201));
#49377=CARTESIAN_POINT('Ctrl Pts',(371.542449288747,-1.30556707575767,3.86872574241488));
#49378=CARTESIAN_POINT('Ctrl Pts',(371.656544623168,-1.29971361808323,3.84784173607042));
#49379=CARTESIAN_POINT('Ctrl Pts',(371.769768572609,-1.29386016040878,3.82189640766259));
#49380=CARTESIAN_POINT('Ctrl Pts',(371.881643231203,-1.28800670273434,3.79098912589329));
#49381=CARTESIAN_POINT('Ctrl Pts',(371.993501104517,-1.28215412329209,3.76008648134384));
#49382=CARTESIAN_POINT('Ctrl Pts',(372.104009691411,-1.27630154384984,3.72422347371164));
#49383=CARTESIAN_POINT('Ctrl Pts',(372.212704251087,-1.2704489644076,3.68354990982684));
#49384=CARTESIAN_POINT('Ctrl Pts',(372.321408786192,-1.26459584784569,3.64287261313136));
#49385=CARTESIAN_POINT('Ctrl Pts',(372.428298576181,-1.25874273128377,3.5973840273411));
#49386=CARTESIAN_POINT('Ctrl Pts',(372.532927603359,-1.25288961472186,3.54728261021654));
#49387=CARTESIAN_POINT('Ctrl Pts',(372.637591533287,-1.24703454564386,3.49716447997482));
#49388=CARTESIAN_POINT('Ctrl Pts',(372.739992828382,-1.24117947656586,3.44243063693976));
#49389=CARTESIAN_POINT('Ctrl Pts',(372.839709509419,-1.23532440748786,3.38332577581028));
#49390=CARTESIAN_POINT('Ctrl Pts',(372.93953920686,-1.22946270242036,3.32415392670291));
#49391=CARTESIAN_POINT('Ctrl Pts',(373.036677861656,-1.22360099735286,3.26060138237516));
#49392=CARTESIAN_POINT('Ctrl Pts',(373.130731885692,-1.21773929228536,3.19295655959848));
#49393=CARTESIAN_POINT('Ctrl Pts',(373.224849333079,-1.21187363450049,3.12526612196006));
#49394=CARTESIAN_POINT('Ctrl Pts',(373.315877684262,-1.20600797671561,3.05347816620013));
#49395=CARTESIAN_POINT('Ctrl Pts',(373.403457240458,-1.20014231893074,2.97792071905295));
#49396=CARTESIAN_POINT('Ctrl Pts',(373.491164850365,-1.19426808472363,2.90225279621936));
#49397=CARTESIAN_POINT('Ctrl Pts',(373.575413302059,-1.18839385051651,2.82280466471597));
#49398=CARTESIAN_POINT('Ctrl Pts',(373.655880419957,-1.1825196163094,2.73994045227431));
#49399=CARTESIAN_POINT('Ctrl Pts',(373.676216509716,-1.18103504774004,2.71899855568341));
#49400=CARTESIAN_POINT('Ctrl Pts',(373.696311290769,-1.17955047917067,2.69783863238138));
#49401=CARTESIAN_POINT('Ctrl Pts',(373.716159987334,-1.17806591060131,2.6764668714688));
#49402=CARTESIAN_POINT('Ctrl Pts',(373.794683068952,-1.17219283482733,2.59191842160054));
#49403=CARTESIAN_POINT('Ctrl Pts',(373.869613173202,-1.16631975905336,2.50377044779303));
#49404=CARTESIAN_POINT('Ctrl Pts',(373.940602311623,-1.16044668327938,2.41236105579295));
#49405=CARTESIAN_POINT('Ctrl Pts',(374.011499772401,-1.15458119218332,2.32106971280559));
#49406=CARTESIAN_POINT('Ctrl Pts',(374.078466137477,-1.14871570108726,2.22652565106339));
#49407=CARTESIAN_POINT('Ctrl Pts',(374.1411908986,-1.1428502099912,2.12910301811899));
#49408=CARTESIAN_POINT('Ctrl Pts',(374.203851418684,-1.13699072617578,2.031780162855));
#49409=CARTESIAN_POINT('Ctrl Pts',(374.26227875325,-1.13113124236035,1.93158494587313));
#49410=CARTESIAN_POINT('Ctrl Pts',(374.316203688908,-1.12527175854492,1.82892318790745));
#49411=CARTESIAN_POINT('Ctrl Pts',(374.37208210082,-1.11920000998845,1.7225424212106));
#49412=CARTESIAN_POINT('Ctrl Pts',(374.42312544687,-1.11312826143198,1.61351337797017));
#49413=CARTESIAN_POINT('Ctrl Pts',(374.469084176485,-1.10705651287551,1.50231913230347));
#49414=CARTESIAN_POINT('Ctrl Pts',(374.513385253775,-1.1012037618458,1.39513547181891));
#49415=CARTESIAN_POINT('Ctrl Pts',(374.552961992507,-1.09535101081608,1.28594051525445));
#49416=CARTESIAN_POINT('Ctrl Pts',(374.587638829686,-1.08949825978636,1.17518962199757));
#49417=CARTESIAN_POINT('Ctrl Pts',(374.62231047179,-1.08364638558061,1.06445532077356));
#49418=CARTESIAN_POINT('Ctrl Pts',(374.652083548501,-1.07779451137487,0.952165940602883));
#49419=CARTESIAN_POINT('Ctrl Pts',(374.676832016761,-1.07194263716912,0.838793122894883));
#49420=CARTESIAN_POINT('Ctrl Pts',(374.701582765721,-1.06609022368301,0.725409857297624));
#49421=CARTESIAN_POINT('Ctrl Pts',(374.721307897605,-1.0602378101969,0.610943359437889));
#49422=CARTESIAN_POINT('Ctrl Pts',(374.735932401061,-1.05438539671079,0.495875912001588));
#49423=CARTESIAN_POINT('Ctrl Pts',(374.750561790914,-1.04853102779313,0.38077001777434));
#49424=CARTESIAN_POINT('Ctrl Pts',(374.760087111469,-1.04267665887547,0.265063184428101));
#49425=CARTESIAN_POINT('Ctrl Pts',(374.764485236239,-1.0368222899578,0.149242559231955));
#49426=CARTESIAN_POINT('Ctrl Pts',(374.768888352225,-1.03096127720409,0.0332904948907921));
#49427=CARTESIAN_POINT('Ctrl Pts',(374.768152643172,-1.02510026445037,-0.0827752058756374));
#49428=CARTESIAN_POINT('Ctrl Pts',(374.762307113717,-1.01923925169666,-0.19846755265044));
#49429=CARTESIAN_POINT('Ctrl Pts',(374.756457638265,-1.01337428249537,-0.31423799696978));
#49430=CARTESIAN_POINT('Ctrl Pts',(374.74549151302,-1.00750931329408,-0.429634175087716));
#49431=CARTESIAN_POINT('Ctrl Pts',(374.729489398386,-1.00164434409279,-0.544176105465635));
#49432=CARTESIAN_POINT('Ctrl Pts',(374.7134638543,-0.995770787713188,-0.658885742091846));
#49433=CARTESIAN_POINT('Ctrl Pts',(374.692387680276,-0.989897231333582,
-0.772738230042964));
#49434=CARTESIAN_POINT('Ctrl Pts',(374.666392213373,-0.984023674953976,
-0.885265552414129));
#49435=CARTESIAN_POINT('Ctrl Pts',(374.659791973369,-0.982532381032535,
-0.913836200417235));
#49436=CARTESIAN_POINT('Ctrl Pts',(374.652874858159,-0.981041087111095,
-0.942321509043616));
#49437=CARTESIAN_POINT('Ctrl Pts',(374.645643516695,-0.979549793189654,
-0.97071400884325));
#49438=CARTESIAN_POINT('Ctrl Pts',(374.61715694645,-0.973675108767121,-1.08256115975804));
#49439=CARTESIAN_POINT('Ctrl Pts',(374.583695430451,-0.967800424344588,
-1.193339308818));
#49440=CARTESIAN_POINT('Ctrl Pts',(374.545354598602,-0.961925739922055,
-1.30257256014839));
#49441=CARTESIAN_POINT('Ctrl Pts',(374.507063277007,-0.956058641592539,
-1.41166475647982));
#49442=CARTESIAN_POINT('Ctrl Pts',(374.463905305323,-0.950191543263022,
-1.51921563629043));
#49443=CARTESIAN_POINT('Ctrl Pts',(374.416026914772,-0.944324444933506,
-1.62476127428801));
#49444=CARTESIAN_POINT('Ctrl Pts',(374.368197573213,-0.938463357149759,
-1.73019878611279));
#49445=CARTESIAN_POINT('Ctrl Pts',(374.315657601324,-0.932602269366011,
-1.83363476839066));
#49446=CARTESIAN_POINT('Ctrl Pts',(374.258602228074,-0.926741181582264,
-1.93462283666815));
#49447=CARTESIAN_POINT('Ctrl Pts',(374.199502020373,-0.920670035507086,
-2.03923026398954));
#49448=CARTESIAN_POINT('Ctrl Pts',(374.135556829694,-0.914598889431908,
-2.14121059590081));
#49449=CARTESIAN_POINT('Ctrl Pts',(374.067037163071,-0.908527743356731,
-2.2400926015992));
#49450=CARTESIAN_POINT('Ctrl Pts',(374.000964430064,-0.902673406442331,
-2.33544339187203));
#49451=CARTESIAN_POINT('Ctrl Pts',(373.930638611108,-0.896819069527931,
-2.42791299446444));
#49452=CARTESIAN_POINT('Ctrl Pts',(373.856347308075,-0.890964732613531,
-2.51710686583075));
#49453=CARTESIAN_POINT('Ctrl Pts',(373.782067250599,-0.885111281876602,
-2.60628723582185));
#49454=CARTESIAN_POINT('Ctrl Pts',(373.703823166845,-0.879257831139672,
-2.6921925432886));
#49455=CARTESIAN_POINT('Ctrl Pts',(373.621943186131,-0.873404380402743,
-2.77446102934122));
#49456=CARTESIAN_POINT('Ctrl Pts',(373.540055815788,-0.867550401394647,
-2.85673694008588));
#49457=CARTESIAN_POINT('Ctrl Pts',(373.454532187536,-0.861696422386551,
-2.93537508420955));
#49458=CARTESIAN_POINT('Ctrl Pts',(373.365737040213,-0.855842443378455,
-3.01005081348208));
#49459=CARTESIAN_POINT('Ctrl Pts',(373.276912424492,-0.849986521613438,
-3.08475132534943));
#49460=CARTESIAN_POINT('Ctrl Pts',(373.184814446699,-0.844130599848422,
-3.15548654184991));
#49461=CARTESIAN_POINT('Ctrl Pts',(373.089840066501,-0.838274678083405,
-3.22197277229532));
#49462=CARTESIAN_POINT('Ctrl Pts',(372.994758363151,-0.832412138997133,
-3.28853413365326));
#49463=CARTESIAN_POINT('Ctrl Pts',(372.896794108303,-0.826549599910861,
-3.35083668854854));
#49464=CARTESIAN_POINT('Ctrl Pts',(372.79637239718,-0.820687060824589,-3.40864063323499));
#49465=CARTESIAN_POINT('Ctrl Pts',(372.695883147442,-0.814820578887978,
-3.46648345396124));
#49466=CARTESIAN_POINT('Ctrl Pts',(372.592933516173,-0.808954096951367,
-3.51982145035608));
#49467=CARTESIAN_POINT('Ctrl Pts',(372.48797072529,-0.803087615014756,-3.56846201867247));
#49468=CARTESIAN_POINT('Ctrl Pts',(372.382854855871,-0.797212577356091,
-3.61717352476511));
#49469=CARTESIAN_POINT('Ctrl Pts',(372.275720347855,-0.791337539697427,
-3.66117377401909));
#49470=CARTESIAN_POINT('Ctrl Pts',(372.167031854818,-0.785462502038762,
-3.70031922811472));
#49471=CARTESIAN_POINT('Ctrl Pts',(372.139720685076,-0.783986226618508,
-3.71015567088388));
#49472=CARTESIAN_POINT('Ctrl Pts',(372.112311454136,-0.782509951198253,
-3.71968582581753));
#49473=CARTESIAN_POINT('Ctrl Pts',(372.084811641178,-0.781033675777999,
-3.72890792140123));
#49474=CARTESIAN_POINT('Ctrl Pts',(371.975390032661,-0.775159583785276,
-3.76560259035059));
#49475=CARTESIAN_POINT('Ctrl Pts',(371.864170034379,-0.769285491792554,
-3.79753784047223));
#49476=CARTESIAN_POINT('Ctrl Pts',(371.751603346463,-0.763411399799832,
-3.82453609263826));
#49477=CARTESIAN_POINT('Ctrl Pts',(371.639181771813,-0.75754488028427,-3.85149954050634));
#49478=CARTESIAN_POINT('Ctrl Pts',(371.525417358021,-0.751678360768709,
-3.87353855180081));
#49479=CARTESIAN_POINT('Ctrl Pts',(371.410779173421,-0.745811841253147,
-3.89052455927433));
#49480=CARTESIAN_POINT('Ctrl Pts',(371.296258165902,-0.739951318183177,
-3.90749320455049));
#49481=CARTESIAN_POINT('Ctrl Pts',(371.180865570266,-0.734090795113207,
-3.91941905930915));
#49482=CARTESIAN_POINT('Ctrl Pts',(371.065082271911,-0.728230272043237,
-3.92622424003878));
#49483=CARTESIAN_POINT('Ctrl Pts',(370.945133517619,-0.722158908973366,
-3.93327424606596));
#49484=CARTESIAN_POINT('Ctrl Pts',(370.824765858313,-0.716087545903495,
-3.9348280894326));
#49485=CARTESIAN_POINT('Ctrl Pts',(370.704522065142,-0.710016182833625,
-3.93085767401927));
#49486=CARTESIAN_POINT('Ctrl Pts',(370.588586917445,-0.704162372373453,
-3.92702952883832));
#49487=CARTESIAN_POINT('Ctrl Pts',(370.47276735942,-0.698308561913282,-3.91806624270722));
#49488=CARTESIAN_POINT('Ctrl Pts',(370.357550777857,-0.692454751453111,
-3.90399566544915));
#49489=CARTESIAN_POINT('Ctrl Pts',(370.242351344099,-0.686601812221728,
-3.88992718232995));
#49490=CARTESIAN_POINT('Ctrl Pts',(370.127755118275,-0.680748872990345,
-3.87075296955846));
#49491=CARTESIAN_POINT('Ctrl Pts',(370.014243898829,-0.674895933758963,
-3.84655270460736));
#49492=CARTESIAN_POINT('Ctrl Pts',(369.900722134928,-0.669042450827617,
-3.82235019160914));
#49493=CARTESIAN_POINT('Ctrl Pts',(369.788285981781,-0.663188967896271,
-3.7931207844239));
#49494=CARTESIAN_POINT('Ctrl Pts',(369.677405889567,-0.657335484964925,
-3.7589950396811));
#49495=CARTESIAN_POINT('Ctrl Pts',(369.566488694934,-0.651480043355766,
-3.72485787586697));
#49496=CARTESIAN_POINT('Ctrl Pts',(369.457128991181,-0.645624601746607,
-3.68582123802798));
#49497=CARTESIAN_POINT('Ctrl Pts',(369.349780267916,-0.639769160137449,
-3.64206495793378));
#49498=CARTESIAN_POINT('Ctrl Pts',(369.242309755129,-0.633907075399046,
-3.59825903536283));
#49499=CARTESIAN_POINT('Ctrl Pts',(369.136855159301,-0.628044990660643,
-3.54972293919225));
#49500=CARTESIAN_POINT('Ctrl Pts',(369.033848334787,-0.62218290592224,-3.49668393098079));
#49501=CARTESIAN_POINT('Ctrl Pts',(368.930771973147,-0.616316863848724,
-3.4436091175671));
#49502=CARTESIAN_POINT('Ctrl Pts',(368.830147030803,-0.610450821775208,
-3.3860255438435));
#49503=CARTESIAN_POINT('Ctrl Pts',(368.732377682707,-0.604584779701691,
-3.32420464465819));
#49504=CARTESIAN_POINT('Ctrl Pts',(368.634465329476,-0.598710157493848,
-3.26229332136535));
#49505=CARTESIAN_POINT('Ctrl Pts',(368.539417244094,-0.592835535286005,
-3.19613253833672));
#49506=CARTESIAN_POINT('Ctrl Pts',(368.447605811247,-0.586960913078162,
-3.12603496920298));
#49507=CARTESIAN_POINT('Ctrl Pts',(368.42445818017,-0.585479794840889,-3.10836186881299));
#49508=CARTESIAN_POINT('Ctrl Pts',(368.401516108419,-0.583998676603616,
-3.09043871241285));
#49509=CARTESIAN_POINT('Ctrl Pts',(368.378785192664,-0.582517558366343,
-3.07227087883228));
#49510=CARTESIAN_POINT('Ctrl Pts',(368.289844403939,-0.576722287043533,
-3.00118436980314));
#49511=CARTESIAN_POINT('Ctrl Pts',(368.203825299216,-0.570927015720722,
-2.92609813391641));
#49512=CARTESIAN_POINT('Ctrl Pts',(368.121116540691,-0.565131744397912,
-2.84728425656222));
#49513=CARTESIAN_POINT('Ctrl Pts',(368.038515306707,-0.559344007148911,
-2.76857284025535));
#49514=CARTESIAN_POINT('Ctrl Pts',(367.959216170142,-0.55355626989991,-2.68614370458509));
#49515=CARTESIAN_POINT('Ctrl Pts',(367.883576547851,-0.54776853265091,-2.60031051006729));
#49516=CARTESIAN_POINT('Ctrl Pts',(367.805377962554,-0.541784990543842,
-2.51157349394409));
#49517=CARTESIAN_POINT('Ctrl Pts',(367.731091271125,-0.535801448436774,
-2.41919826775779));
#49518=CARTESIAN_POINT('Ctrl Pts',(367.661072177725,-0.529817906329707,
-2.32357502201362));
#49519=CARTESIAN_POINT('Ctrl Pts',(367.593463091785,-0.524040313491905,
-2.23124306046759));
#49520=CARTESIAN_POINT('Ctrl Pts',(367.529832947823,-0.518262720654104,
-2.13588335750866));
#49521=CARTESIAN_POINT('Ctrl Pts',(367.470461955913,-0.512485127816302,
-2.03788186657742));
#49522=CARTESIAN_POINT('Ctrl Pts',(367.411112110333,-0.506709592799693,
-1.93991528110778));
#49523=CARTESIAN_POINT('Ctrl Pts',(367.356018622257,-0.500934057783084,
-1.83930914069092));
#49524=CARTESIAN_POINT('Ctrl Pts',(367.305418137936,-0.495158522766475,
-1.73647798702939));
#49525=CARTESIAN_POINT('Ctrl Pts',(367.254822666203,-0.489383559886301,
-1.63365702003447));
#49526=CARTESIAN_POINT('Ctrl Pts',(367.20871950042,-0.483608597006127,-1.52861185975074));
#49527=CARTESIAN_POINT('Ctrl Pts',(367.167298712719,-0.477833634125952,
-1.42178044126834));
#49528=CARTESIAN_POINT('Ctrl Pts',(367.125871378126,-0.472057758465783,
-1.31493213720873));
#49529=CARTESIAN_POINT('Ctrl Pts',(367.08912804447,-0.466281882805614,-1.2062974108198));
#49530=CARTESIAN_POINT('Ctrl Pts',(367.057209835283,-0.460506007145445,
-1.09633207597307));
#49531=CARTESIAN_POINT('Ctrl Pts',(367.025262440197,-0.454724850044727,
-0.98626618920787));
#49532=CARTESIAN_POINT('Ctrl Pts',(366.998149092602,-0.448943692944008,
-0.874867674653828));
#49533=CARTESIAN_POINT('Ctrl Pts',(366.975960385223,-0.443162535843289,
-0.762605172500647));
#49534=CARTESIAN_POINT('Ctrl Pts',(366.95375949395,-0.437378204289422,-0.650281026623353));
#49535=CARTESIAN_POINT('Ctrl Pts',(366.93648868851,-0.431593872735556,-0.537092368462364));
#49536=CARTESIAN_POINT('Ctrl Pts',(366.924186782274,-0.425809541181689,
-0.423513881694839));
#49537=CARTESIAN_POINT('Ctrl Pts',(366.911868734401,-0.420017619863102,
-0.309786365781283));
#49538=CARTESIAN_POINT('Ctrl Pts',(366.904532619862,-0.414225698544515,
-0.195668423477765));
#49539=CARTESIAN_POINT('Ctrl Pts',(366.902165180061,-0.408433777225929,
-0.0816355004928817));
#49540=CARTESIAN_POINT('Ctrl Pts',(366.901583359773,-0.407010358844382,
-0.0536108520645037));
#49541=CARTESIAN_POINT('Ctrl Pts',(366.901301389935,-0.405586940462834,
-0.0255913162295418));
#49542=CARTESIAN_POINT('Ctrl Pts',(366.90131859535,-0.404163522081287,0.00241610556833745));
#49543=CARTESIAN_POINT('Origin',(370.834317853224,2.31077344927308,0.));
#49544=CARTESIAN_POINT('',(372.667675165437,-25.,-2.65045628680305));
#49545=CARTESIAN_POINT('Ctrl Pts',(372.667675165437,-25.,-2.65045628680305));
#49546=CARTESIAN_POINT('Ctrl Pts',(372.448644400709,-24.9825465826754,-2.80196289949983));
#49547=CARTESIAN_POINT('Ctrl Pts',(372.211615774371,-24.9641309779199,-2.92577950427151));
#49548=CARTESIAN_POINT('Ctrl Pts',(371.828930661503,-24.9370043306435,-3.0687182706999));
#49549=CARTESIAN_POINT('Ctrl Pts',(371.692738286308,-24.9277863008836,-3.10956755196565));
#49550=CARTESIAN_POINT('Ctrl Pts',(371.526496104034,-24.9170663903206,-3.14766884848412));
#49551=CARTESIAN_POINT('Ctrl Pts',(371.498630778317,-24.9152866573577,-3.15366744148132));
#49552=CARTESIAN_POINT('Ctrl Pts',(371.454762329649,-24.912510851018,-3.16250377998708));
#49553=CARTESIAN_POINT('Ctrl Pts',(371.438811594471,-24.9115069253944,-3.16559138848816));
#49554=CARTESIAN_POINT('Ctrl Pts',(371.408987931986,-24.9096396289647,-3.17113076108422));
#49555=CARTESIAN_POINT('Ctrl Pts',(371.39512101949,-24.9087753361535,-3.17361242465044));
#49556=CARTESIAN_POINT('Ctrl Pts',(371.364157131943,-24.9068539790705,-3.17894452811137));
#49557=CARTESIAN_POINT('Ctrl Pts',(371.347052456556,-24.9057984052931,-3.18174813878929));
#49558=CARTESIAN_POINT('Ctrl Pts',(371.303717882357,-24.9031382618445,-3.18849253783978));
#49559=CARTESIAN_POINT('Ctrl Pts',(371.277460116567,-24.901539479463,-3.19224780493738));
#49560=CARTESIAN_POINT('Ctrl Pts',(371.10932941491,-24.8913804173512,-3.21417857478562));
#49561=CARTESIAN_POINT('Ctrl Pts',(370.96641742835,-24.8831096809257,-3.22321763238307));
#49562=CARTESIAN_POINT('Ctrl Pts',(370.550408909798,-24.8594849897765,-3.22180359197394));
#49563=CARTESIAN_POINT('Ctrl Pts',(370.278717867171,-24.844678208846,-3.18620362372021));
#49564=CARTESIAN_POINT('Ctrl Pts',(369.990265227191,-24.8269501791359,-3.11035952347186));
#49565=CARTESIAN_POINT('Ctrl Pts',(369.965806970226,-24.8254299562328,-3.10361885001254));
#49566=CARTESIAN_POINT('Ctrl Pts',(369.922745060926,-24.8227190856935,-3.09120216531442));
#49567=CARTESIAN_POINT('Ctrl Pts',(369.904108168936,-24.8215343823679,-3.08564510015569));
#49568=CARTESIAN_POINT('Ctrl Pts',(369.87623249699,-24.8197435756331,-3.07705777032747));
#49569=CARTESIAN_POINT('Ctrl Pts',(369.866954900638,-24.8191444145313,-3.07415370209092));
#49570=CARTESIAN_POINT('Ctrl Pts',(369.857633356544,-24.8185391144997,-3.07118950246782));
#49571=CARTESIAN_POINT('Ctrl Pts',(369.857575988279,-24.8185353891312,-3.07117125790598));
#49572=CARTESIAN_POINT('Ctrl Pts',(369.857460101296,-24.8185278634317,-3.0711343993334));
#49573=CARTESIAN_POINT('Ctrl Pts',(369.857401583238,-24.8185240631386,-3.07111578546099));
#49574=CARTESIAN_POINT('Ctrl Pts',(369.857283356749,-24.8185163849817,-3.07107817535193));
#49575=CARTESIAN_POINT('Ctrl Pts',(369.85722364791,-24.8185125070862,-3.0710591789102));
#49576=CARTESIAN_POINT('Ctrl Pts',(369.857102998182,-24.8185046710014,-3.07102079017294));
#49577=CARTESIAN_POINT('Ctrl Pts',(369.857042056687,-24.8185007127672,-3.07100139760502));
#49578=CARTESIAN_POINT('Ctrl Pts',(369.856918897049,-24.818492713091,-3.07096220218226));
#49579=CARTESIAN_POINT('Ctrl Pts',(369.856856679008,-24.8184886716497,-3.07094239927493));
#49580=CARTESIAN_POINT('Ctrl Pts',(369.856730919775,-24.8184805025203,-3.0709023681155));
#49581=CARTESIAN_POINT('Ctrl Pts',(369.856667378586,-24.818476374826,-3.0708821397745));
#49582=CARTESIAN_POINT('Ctrl Pts',(369.856538924669,-24.818468030028,-3.07084124207271));
#49583=CARTESIAN_POINT('Ctrl Pts',(369.856474011656,-24.8184638128991,-3.07082057252598));
#49584=CARTESIAN_POINT('Ctrl Pts',(369.856342762487,-24.8184552858586,-3.07077877569272));
#49585=CARTESIAN_POINT('Ctrl Pts',(369.85627642705,-24.8184509759866,-3.07075764853467));
#49586=CARTESIAN_POINT('Ctrl Pts',(369.856142279099,-24.8184422599342,-3.07071491899692));
#49587=CARTESIAN_POINT('Ctrl Pts',(369.856074467295,-24.8184378537922,-3.07069331673669));
#49588=CARTESIAN_POINT('Ctrl Pts',(369.85593731171,-24.8184289416095,-3.07064961918199));
#49589=CARTESIAN_POINT('Ctrl Pts',(369.855867966481,-24.8184244354665,-3.07062752331326));
#49590=CARTESIAN_POINT('Ctrl Pts',(369.855727684286,-24.8184153193739,-3.07058281915683));
#49591=CARTESIAN_POINT('Ctrl Pts',(369.855656747705,-24.8184107094406,-3.0705602108717));
#49592=CARTESIAN_POINT('Ctrl Pts',(369.855513219865,-24.8184013816509,-3.07051446145761));
#49593=CARTESIAN_POINT('Ctrl Pts',(369.855440628942,-24.8183966638072,-3.07049132030815));
#49594=CARTESIAN_POINT('Ctrl Pts',(369.847994664454,-24.8179127134251,-3.06811734176985));
#49595=CARTESIAN_POINT('Ctrl Pts',(369.840630029142,-24.8174319473629,-3.06574003490417));
#49596=CARTESIAN_POINT('Ctrl Pts',(369.824164976934,-24.8163523461005,-3.06035954786767));
#49597=CARTESIAN_POINT('Ctrl Pts',(369.815069493631,-24.8157527247522,-3.05734233798866));
#49598=CARTESIAN_POINT('Ctrl Pts',(369.788636750979,-24.8140009819724,-3.04844284487031));
#49599=CARTESIAN_POINT('Ctrl Pts',(369.771336317858,-24.8128429491999,-3.04245344509478));
#49600=CARTESIAN_POINT('Ctrl Pts',(369.635473765185,-24.8036630351799,-2.99411767027075));
#49601=CARTESIAN_POINT('Ctrl Pts',(369.519446179933,-24.7953107027065,-2.94500820969916));
#49602=CARTESIAN_POINT('Ctrl Pts',(369.237719907392,-24.7741943945758,-2.80579363204798));
#49603=CARTESIAN_POINT('Ctrl Pts',(369.076468127299,-24.7613567555453,-2.70768806915914));
#49604=CARTESIAN_POINT('Ctrl Pts',(368.850610676171,-24.7427634833968,-2.54155160852021));
#49605=CARTESIAN_POINT('Ctrl Pts',(368.778875998483,-24.736748506122,-2.48389612085732));
#49606=CARTESIAN_POINT('Ctrl Pts',(368.664648623588,-24.7270015686668,-2.38374558430222));
#49607=CARTESIAN_POINT('Ctrl Pts',(368.620704247582,-24.7232063679244,-2.34299448258911));
#49608=CARTESIAN_POINT('Ctrl Pts',(368.562442854931,-24.7181082446221,-2.28586337902372));
#49609=CARTESIAN_POINT('Ctrl Pts',(368.547119691573,-24.7167608045272,-2.27053121568268));
#49610=CARTESIAN_POINT('Ctrl Pts',(368.521638175581,-24.7145085004393,-2.24451498892669));
#49611=CARTESIAN_POINT('Ctrl Pts',(368.51139650745,-24.7136000178971,-2.23391388815233));
#49612=CARTESIAN_POINT('Ctrl Pts',(368.491315878479,-24.7118121794831,-2.21284110347961));
#49613=CARTESIAN_POINT('Ctrl Pts',(368.481473510801,-24.7109326879771,-2.20237315496441));
#49614=CARTESIAN_POINT('Ctrl Pts',(368.457736306143,-24.7088035255141,-2.17678646904523));
#49615=CARTESIAN_POINT('Ctrl Pts',(368.443915202735,-24.7075569874861,-2.16159995841331));
#49616=CARTESIAN_POINT('Ctrl Pts',(368.405082155698,-24.7040340641129,-2.11810256816424));
#49617=CARTESIAN_POINT('Ctrl Pts',(368.380421046954,-24.7017721168798,-2.08948204214576));
#49618=CARTESIAN_POINT('Ctrl Pts',(368.22345784469,-24.6871946865673,-1.90070496737995));
#49619=CARTESIAN_POINT('Ctrl Pts',(368.106396810433,-24.6755073333159,-1.72850492485538));
#49620=CARTESIAN_POINT('Ctrl Pts',(367.908279587927,-24.6524023262666,-1.36620364124558));
#49621=CARTESIAN_POINT('Ctrl Pts',(367.827270016994,-24.6410225564316,-1.17722327904833));
#49622=CARTESIAN_POINT('Ctrl Pts',(367.754874649746,-24.6268407545519,-0.950896249762951));
#49623=CARTESIAN_POINT('Ctrl Pts',(367.745441007328,-24.6248795069265,-0.91979006752573));
#49624=CARTESIAN_POINT('Ctrl Pts',(367.733171356619,-24.6221591993239,-0.8770130940487));
#49625=CARTESIAN_POINT('Ctrl Pts',(367.729927357094,-24.6214222110258,-0.865460107440159));
#49626=CARTESIAN_POINT('Ctrl Pts',(367.724582672227,-24.620177115909,-0.84600913422874));
#49627=CARTESIAN_POINT('Ctrl Pts',(367.722447342584,-24.6196709816418,-0.838120679040251));
#49628=CARTESIAN_POINT('Ctrl Pts',(367.718449441033,-24.6187064853374,-0.823125491887318));
#49629=CARTESIAN_POINT('Ctrl Pts',(367.716581122336,-24.618248462339,-0.816020349700292));
#49630=CARTESIAN_POINT('Ctrl Pts',(367.712192384105,-24.6171550802018,-0.799095054810847));
#49631=CARTESIAN_POINT('Ctrl Pts',(367.709693991064,-24.6165184813489,-0.789269323539435));
#49632=CARTESIAN_POINT('Ctrl Pts',(367.700998727986,-24.6142521411005,-0.754383993529306));
#49633=CARTESIAN_POINT('Ctrl Pts',(367.695056821389,-24.6126088849863,-0.729262659499962));
#49634=CARTESIAN_POINT('Ctrl Pts',(367.644210762084,-24.5976682215547,-0.502147501288212));
#49635=CARTESIAN_POINT('Ctrl Pts',(367.618560359983,-24.5835631112317,-0.296353905149716));
#49636=CARTESIAN_POINT('Ctrl Pts',(367.608444592571,-24.5589525710454,0.0675882832181993));
#49637=CARTESIAN_POINT('Ctrl Pts',(367.615578627539,-24.5484219776061,0.224841692000858));
#49638=CARTESIAN_POINT('Ctrl Pts',(367.640848444246,-24.5345278856317,0.437113961219011));
#49639=CARTESIAN_POINT('Ctrl Pts',(367.649010363277,-24.5308933608261,0.493084476890864));
#49640=CARTESIAN_POINT('Ctrl Pts',(367.665730274147,-24.5246614758267,0.589833139501906));
#49641=CARTESIAN_POINT('Ctrl Pts',(367.673613436201,-24.5220441082923,0.630712476995468));
#49642=CARTESIAN_POINT('Ctrl Pts',(367.686182511502,-24.5182875522315,0.689718126841434));
#49643=CARTESIAN_POINT('Ctrl Pts',(367.690237487035,-24.5171283371825,0.707973091989622));
#49644=CARTESIAN_POINT('Ctrl Pts',(367.697622558549,-24.5151056053922,0.739904231990943));
#49645=CARTESIAN_POINT('Ctrl Pts',(367.700883758669,-24.5142398970322,0.753595666965451));
#49646=CARTESIAN_POINT('Ctrl Pts',(367.707833107197,-24.5124504697705,0.781945749512933));
#49647=CARTESIAN_POINT('Ctrl Pts',(367.711534907162,-24.5115272161059,0.796600719543625));
#49648=CARTESIAN_POINT('Ctrl Pts',(367.721368043498,-24.5091496892589,0.834406722176211));
#49649=CARTESIAN_POINT('Ctrl Pts',(367.727654647783,-24.5077004784285,0.857516688720314));
#49650=CARTESIAN_POINT('Ctrl Pts',(367.754164313037,-24.5018622048959,0.950847753848242));
#49651=CARTESIAN_POINT('Ctrl Pts',(367.776516171631,-24.4975425793569,1.0204446884582));
#49652=CARTESIAN_POINT('Ctrl Pts',(367.91174684713,-24.4742387812159,1.3970134496823));
#49653=CARTESIAN_POINT('Ctrl Pts',(368.068460868441,-24.4568146728287,1.68613905001018));
#49654=CARTESIAN_POINT('Ctrl Pts',(368.294072103768,-24.4351298586021,1.98379263453229));
#49655=CARTESIAN_POINT('Ctrl Pts',(368.322970896775,-24.4323959671463,2.02025189505488));
#49656=CARTESIAN_POINT('Ctrl Pts',(368.372280468171,-24.4277781135113,2.07976837824262));
#49657=CARTESIAN_POINT('Ctrl Pts',(368.392251370031,-24.4259198657318,2.10318228528034));
#49658=CARTESIAN_POINT('Ctrl Pts',(368.420256956186,-24.423324539156,2.13507935857053));
#49659=CARTESIAN_POINT('Ctrl Pts',(368.428007762108,-24.4226073393088,2.14381100323403));
#49660=CARTESIAN_POINT('Ctrl Pts',(368.44118661164,-24.4213892975892,2.15849608015382));
#49661=CARTESIAN_POINT('Ctrl Pts',(368.446589937204,-24.4208902973008,2.16447172894608));
#49662=CARTESIAN_POINT('Ctrl Pts',(368.457004507245,-24.4199291385269,2.17590296018725));
#49663=CARTESIAN_POINT('Ctrl Pts',(368.462012207988,-24.4194672695119,2.18136158398425));
#49664=CARTESIAN_POINT('Ctrl Pts',(368.474044505634,-24.4183583093244,2.19438690475123));
#49665=CARTESIAN_POINT('Ctrl Pts',(368.481086681469,-24.4177099117997,2.20193714909296));
#49666=CARTESIAN_POINT('Ctrl Pts',(368.506646196549,-24.4153593122862,2.22907804030539));
#49667=CARTESIAN_POINT('Ctrl Pts',(368.525372302698,-24.4136423291366,2.2484693872613));
#49668=CARTESIAN_POINT('Ctrl Pts',(368.663434474271,-24.4010358399676,2.38789270398049));
#49669=CARTESIAN_POINT('Ctrl Pts',(368.79180902506,-24.3896077842501,2.49858222083691));
#49670=CARTESIAN_POINT('Ctrl Pts',(369.048805288126,-24.3680466591981,2.6870818749653));
#49671=CARTESIAN_POINT('Ctrl Pts',(369.175358541804,-24.3579426514072,2.76700631833854));
#49672=CARTESIAN_POINT('Ctrl Pts',(369.416006733603,-24.3399045566596,2.89652075102262));
#49673=CARTESIAN_POINT('Ctrl Pts',(369.528302107213,-24.3319085557739,2.94885879544395));
#49674=CARTESIAN_POINT('Ctrl Pts',(369.668799533226,-24.3224121125225,3.00473545055009));
#49675=CARTESIAN_POINT('Ctrl Pts',(369.694384471477,-24.3207023634977,3.01453479688036));
#49676=CARTESIAN_POINT('Ctrl Pts',(369.735040542545,-24.3180156013457,3.02951493747084));
#49677=CARTESIAN_POINT('Ctrl Pts',(369.750030027022,-24.3170314284073,3.03491207230534));
#49678=CARTESIAN_POINT('Ctrl Pts',(369.778264914666,-24.3151893938906,3.04484247837024));
#49679=CARTESIAN_POINT('Ctrl Pts',(369.791500978281,-24.314330713612,3.04940100711966));
#49680=CARTESIAN_POINT('Ctrl Pts',(369.821314062131,-24.3124072557553,3.05945188317832));
#49681=CARTESIAN_POINT('Ctrl Pts',(369.837906948615,-24.3113440832327,3.06489605599716));
#49682=CARTESIAN_POINT('Ctrl Pts',(369.880429384887,-24.3086377413946,3.0784659606429));
#49683=CARTESIAN_POINT('Ctrl Pts',(369.906419254964,-24.3070008556421,3.08639921916594));
#49684=CARTESIAN_POINT('Ctrl Pts',(370.089208444093,-24.2956025865504,3.13967689232167));
#49685=CARTESIAN_POINT('Ctrl Pts',(370.249162826964,-24.2862304451696,3.17338341285399));
#49686=CARTESIAN_POINT('Ctrl Pts',(370.509786338017,-24.2714012237934,3.20791628792476));
#49687=CARTESIAN_POINT('Ctrl Pts',(370.609127559571,-24.2658453950762,3.21641684016187));
#49688=CARTESIAN_POINT('Ctrl Pts',(370.893389874481,-24.2499163336759,3.22750509283093));
#49689=CARTESIAN_POINT('Ctrl Pts',(371.078329291471,-24.2395229202987,3.21880692367392));
#49690=CARTESIAN_POINT('Ctrl Pts',(371.281087576833,-24.2271569274619,3.19169326875078));
#49691=CARTESIAN_POINT('Ctrl Pts',(371.300675367745,-24.2259520033238,3.18889004700043));
#49692=CARTESIAN_POINT('Ctrl Pts',(371.329954868622,-24.2241338194649,3.18442430814373));
#49693=CARTESIAN_POINT('Ctrl Pts',(371.339667211896,-24.2235278853744,3.18289746066198));
#49694=CARTESIAN_POINT('Ctrl Pts',(371.356367178406,-24.2224809131446,3.18019374816224));
#49695=CARTESIAN_POINT('Ctrl Pts',(371.36335812424,-24.2220410826176,3.17903824514712));
#49696=CARTESIAN_POINT('Ctrl Pts',(371.379326052975,-24.2210328811139,3.17634484477636));
#49697=CARTESIAN_POINT('Ctrl Pts',(371.388300192321,-24.2204636866194,3.17479197332667));
#49698=CARTESIAN_POINT('Ctrl Pts',(371.412944970897,-24.2188937096521,3.17041980500747));
#49699=CARTESIAN_POINT('Ctrl Pts',(371.428601245566,-24.2178887090549,3.1675224240247));
#49700=CARTESIAN_POINT('Ctrl Pts',(371.510125350543,-24.2126179815457,3.15180973416503));
#49701=CARTESIAN_POINT('Ctrl Pts',(371.575597974716,-24.2082571103843,3.13705638151097));
#49702=CARTESIAN_POINT('Ctrl Pts',(371.871917901754,-24.1880737826883,3.06049102449278));
#49703=CARTESIAN_POINT('Ctrl Pts',(372.095911851213,-24.1716317433924,2.97516493087494));
#49704=CARTESIAN_POINT('Ctrl Pts',(372.308887474584,-24.1556842688952,2.86561725805281));
#49705=CARTESIAN_POINT('Ctrl Pts',(372.309354074345,-24.1556493282545,2.86537711030611));
#49706=CARTESIAN_POINT('Ctrl Pts',(372.309820613613,-24.1556143901908,2.86513684953877));
#49707=CARTESIAN_POINT('',(368.962731321485,-25.,-2.62360084935054));
#49708=CARTESIAN_POINT('Origin',(370.834317853224,-25.,0.));
#49709=CARTESIAN_POINT('',(367.611568051603,-24.8107734493349,0.00113077379776494));
#49710=CARTESIAN_POINT('Ctrl Pts',(367.611568051603,-24.8107734493349,0.00113077379776616));
#49711=CARTESIAN_POINT('Ctrl Pts',(367.611532632817,-24.8170524822338,-0.0998141594584466));
#49712=CARTESIAN_POINT('Ctrl Pts',(367.616244250843,-24.8233315151327,-0.200925999541271));
#49713=CARTESIAN_POINT('Ctrl Pts',(367.625723725616,-24.8296105480316,-0.301730486989598));
#49714=CARTESIAN_POINT('Ctrl Pts',(367.635188640088,-24.83587993645,-0.402380140575898));
#49715=CARTESIAN_POINT('Ctrl Pts',(367.649406805622,-24.8421493248684,-0.502722969158722));
#49716=CARTESIAN_POINT('Ctrl Pts',(367.668347051272,-24.8484187132868,-0.602284354511512));
#49717=CARTESIAN_POINT('Ctrl Pts',(367.687427772115,-24.8547346002331,-0.702584162427144));
#49718=CARTESIAN_POINT('Ctrl Pts',(367.711300931888,-24.8610504871795,-0.802090458055011));
#49719=CARTESIAN_POINT('Ctrl Pts',(367.739881201516,-24.8673663741259,-0.900321815278267));
#49720=CARTESIAN_POINT('Ctrl Pts',(367.768181811235,-24.8736204596831,-0.997591971898902));
#49721=CARTESIAN_POINT('Ctrl Pts',(367.801097712235,-24.8798745452403,-1.09361161824043));
#49722=CARTESIAN_POINT('Ctrl Pts',(367.838494790759,-24.8861286307975,-1.18792328914835));
#49723=CARTESIAN_POINT('Ctrl Pts',(367.87586737887,-24.8923786207103,-1.28217319769909));
#49724=CARTESIAN_POINT('Ctrl Pts',(367.917715153791,-24.8986286106231,-1.37471696939067));
#49725=CARTESIAN_POINT('Ctrl Pts',(367.963854745441,-24.9048786005359,-1.46511402605999));
#49726=CARTESIAN_POINT('Ctrl Pts',(368.009975053366,-24.9111259783083,-1.55547330190093));
#49727=CARTESIAN_POINT('Ctrl Pts',(368.060383419315,-24.9173733560808,-1.64368727742382));
#49728=CARTESIAN_POINT('Ctrl Pts',(368.114849422389,-24.9236207338533,-1.72933773919208));
#49729=CARTESIAN_POINT('Ctrl Pts',(368.17034034856,-24.9299856726988,-1.81659994280811));
#49730=CARTESIAN_POINT('Ctrl Pts',(368.230042973355,-24.9363506115444,-1.90120077635747));
#49731=CARTESIAN_POINT('Ctrl Pts',(368.293666270147,-24.94271555039,-1.98272718645562));
#49732=CARTESIAN_POINT('Ctrl Pts',(368.356124673653,-24.9489639521351,-2.06276091112919));
#49733=CARTESIAN_POINT('Ctrl Pts',(368.422361097585,-24.9552123538801,-2.13983153035847));
#49734=CARTESIAN_POINT('Ctrl Pts',(368.492059063977,-24.9614607556252,-2.21358110912948));
#49735=CARTESIAN_POINT('Ctrl Pts',(368.563706904731,-24.967883963021,-2.28939391040608));
#49736=CARTESIAN_POINT('Ctrl Pts',(368.639012527615,-24.9743071704168,-2.36169675026738));
#49737=CARTESIAN_POINT('Ctrl Pts',(368.71759196548,-24.9807303778126,-2.43014178159498));
#49738=CARTESIAN_POINT('Ctrl Pts',(368.796171403344,-24.9871535852084,-2.4985868129226));
#49739=CARTESIAN_POINT('Ctrl Pts',(368.878024270347,-24.9935767926042,-2.56317375500353));
#49740=CARTESIAN_POINT('Ctrl Pts',(368.962731321485,-25.,-2.62360084935057));
#49741=CARTESIAN_POINT('Ctrl Pts',(372.309820613641,-24.4036702759164,2.86513684952406));
#49742=CARTESIAN_POINT('Ctrl Pts',(372.306091397025,-24.4039307331992,2.86705734048141));
#49743=CARTESIAN_POINT('Ctrl Pts',(372.30235869357,-24.4041911904821,2.86897041531283));
#49744=CARTESIAN_POINT('Ctrl Pts',(372.298622535419,-24.404451647765,2.87087606144891));
#49745=CARTESIAN_POINT('Ctrl Pts',(372.210067064788,-24.4106250794922,2.91604422179583));
#49746=CARTESIAN_POINT('Ctrl Pts',(372.1192665904,-24.4167985112193,2.95718926796437));
#49747=CARTESIAN_POINT('Ctrl Pts',(372.02662222988,-24.4229719429465,2.99408213579816));
#49748=CARTESIAN_POINT('Ctrl Pts',(371.934101242199,-24.429137153625,3.03092587405992));
#49749=CARTESIAN_POINT('Ctrl Pts',(371.839741648865,-24.4353023643036,3.06352853005277));
#49750=CARTESIAN_POINT('Ctrl Pts',(371.743968650642,-24.4414675749822,3.09170713187007));
#49751=CARTESIAN_POINT('Ctrl Pts',(371.648294949118,-24.4476263936183,3.11985651833244));
#49752=CARTESIAN_POINT('Ctrl Pts',(371.551211170352,-24.4537852122544,3.14359084808161));
#49753=CARTESIAN_POINT('Ctrl Pts',(371.453161060238,-24.4599440308906,3.16277578206753));
#49754=CARTESIAN_POINT('Ctrl Pts',(371.355179532076,-24.4660985416906,3.18194729699424));
#49755=CARTESIAN_POINT('Ctrl Pts',(371.256233441068,-24.4722530524906,3.1965756592847));
#49756=CARTESIAN_POINT('Ctrl Pts',(371.156779335197,-24.4784075632906,3.20657701531455));
#49757=CARTESIAN_POINT('Ctrl Pts',(371.057360987235,-24.4845598612867,3.21657477543887));
#49758=CARTESIAN_POINT('Ctrl Pts',(370.957435418787,-24.4907121592828,3.22194879154235));
#49759=CARTESIAN_POINT('Ctrl Pts',(370.857466062772,-24.4968644572789,3.22266686501949));
#49760=CARTESIAN_POINT('Ctrl Pts',(370.757505958301,-24.5030161859181,3.2233848720434));
#49761=CARTESIAN_POINT('Ctrl Pts',(370.657502508378,-24.5091679145573,3.21944779003459));
#49762=CARTESIAN_POINT('Ctrl Pts',(370.557919914596,-24.5153196431964,3.21087554134724));
#49763=CARTESIAN_POINT('Ctrl Pts',(370.458319948442,-24.5214724450163,3.20230179721487));
#49764=CARTESIAN_POINT('Ctrl Pts',(370.359141416761,-24.5276252468362,3.18909131732326));
#49765=CARTESIAN_POINT('Ctrl Pts',(370.26084316178,-24.533778048656,3.17131586896868));
#49766=CARTESIAN_POINT('Ctrl Pts',(370.16243769844,-24.5399375609896,3.15352103393585));
#49767=CARTESIAN_POINT('Ctrl Pts',(370.064914856823,-24.5460970733231,3.1311513661488));
#49768=CARTESIAN_POINT('Ctrl Pts',(369.968722937462,-24.5522565856567,3.10432971900659));
#49769=CARTESIAN_POINT('Ctrl Pts',(369.87247588136,-24.5584196285928,3.07749269782637));
#49770=CARTESIAN_POINT('Ctrl Pts',(369.777561678892,-24.5645826715289,3.04619875142091));
#49771=CARTESIAN_POINT('Ctrl Pts',(369.684411120004,-24.5707457144651,3.01061988092088));
#49772=CARTESIAN_POINT('Ctrl Pts',(369.591104061668,-24.576919111744,2.97498123543201));
#49773=CARTESIAN_POINT('Ctrl Pts',(369.499566963191,-24.583092509023,2.93504346035694));
#49774=CARTESIAN_POINT('Ctrl Pts',(369.410208500937,-24.589265906302,2.89102578944393));
#49775=CARTESIAN_POINT('Ctrl Pts',(369.344098114509,-24.5938331925936,2.85846004065685));
#49776=CARTESIAN_POINT('Ctrl Pts',(369.279179732003,-24.5984004788852,2.82366213004029));
#49777=CARTESIAN_POINT('Ctrl Pts',(369.21560850966,-24.6029677651768,2.78673601612322));
#49778=CARTESIAN_POINT('Ctrl Pts',(369.130345774173,-24.6090934822642,2.73721012425808));
#49779=CARTESIAN_POINT('Ctrl Pts',(369.047195657591,-24.6152191993517,2.68367310090506));
#49780=CARTESIAN_POINT('Ctrl Pts',(368.966564492119,-24.6213449164392,2.62633108053452));
#49781=CARTESIAN_POINT('Ctrl Pts',(368.8860431591,-24.6274622893271,2.56906716910233));
#49782=CARTESIAN_POINT('Ctrl Pts',(368.808034316457,-24.6335796622151,2.50800881178686));
#49783=CARTESIAN_POINT('Ctrl Pts',(368.732919098709,-24.639697035103,2.44340762809323));
#49784=CARTESIAN_POINT('Ctrl Pts',(368.657883150478,-24.6458079522926,2.37887461839631));
#49785=CARTESIAN_POINT('Ctrl Pts',(368.585735091412,-24.6519188694821,2.31080649870567));
#49786=CARTESIAN_POINT('Ctrl Pts',(368.516825603552,-24.6580297866716,2.23949709426277));
#49787=CARTESIAN_POINT('Ctrl Pts',(368.447963610342,-24.6641364920193,2.16823683856927));
#49788=CARTESIAN_POINT('Ctrl Pts',(368.382336059312,-24.6702431973669,2.09374005345202));
#49789=CARTESIAN_POINT('Ctrl Pts',(368.320258416095,-24.6763499027146,2.01633893705434));
#49790=CARTESIAN_POINT('Ctrl Pts',(368.258202584804,-24.6824544623782,1.93896501671871));
#49791=CARTESIAN_POINT('Ctrl Pts',(368.199694460286,-24.6885590220418,1.85868913594861));
#49792=CARTESIAN_POINT('Ctrl Pts',(368.145009988683,-24.6946635817054,1.77587746542934));
#49793=CARTESIAN_POINT('Ctrl Pts',(368.090329549862,-24.70076769118,1.69307190196973));
#49794=CARTESIAN_POINT('Ctrl Pts',(368.039472447071,-24.7068718006545,1.60773128897416));
#49795=CARTESIAN_POINT('Ctrl Pts',(367.99267131847,-24.7129759101291,1.52025081286566));
#49796=CARTESIAN_POINT('Ctrl Pts',(367.945860647835,-24.719081264138,1.43275250082949));
#49797=CARTESIAN_POINT('Ctrl Pts',(367.903107802019,-24.7251866181468,1.343113848744));
#49798=CARTESIAN_POINT('Ctrl Pts',(367.864598960317,-24.7312919721557,1.25175367369583));
#49799=CARTESIAN_POINT('Ctrl Pts',(367.826044262477,-24.73740459639,1.16028470740223));
#49800=CARTESIAN_POINT('Ctrl Pts',(367.791743830973,-24.7435172206243,1.06709053296559));
#49801=CARTESIAN_POINT('Ctrl Pts',(367.761835195747,-24.7496298448586,0.972608802140001));
#49802=CARTESIAN_POINT('Ctrl Pts',(367.731908164023,-24.7557462289058,0.878068956563135));
#49803=CARTESIAN_POINT('Ctrl Pts',(367.706378417981,-24.7618626129531,0.78224040508794));
#49804=CARTESIAN_POINT('Ctrl Pts',(367.685332644382,-24.7679789970003,0.685572546850148));
#49805=CARTESIAN_POINT('Ctrl Pts',(367.664248227904,-24.7741066115537,0.588727193385713));
#49806=CARTESIAN_POINT('Ctrl Pts',(367.647664300376,-24.7802342261071,0.491039890785891));
#49807=CARTESIAN_POINT('Ctrl Pts',(367.635615838181,-24.7863618406604,0.392966896139527));
#49808=CARTESIAN_POINT('Ctrl Pts',(367.625704566898,-24.7914025213031,0.312290371633089));
#49809=CARTESIAN_POINT('Ctrl Pts',(367.618861470473,-24.7964432019457,0.231353040806152));
#49810=CARTESIAN_POINT('Ctrl Pts',(367.615079585837,-24.8014838825884,0.150407913003267));
#49811=CARTESIAN_POINT('Ctrl Pts',(367.612756350015,-24.8045804048166,0.100682805368083));
#49812=CARTESIAN_POINT('Ctrl Pts',(367.611585518489,-24.8076769270449,0.0509120444049194));
#49813=CARTESIAN_POINT('Ctrl Pts',(367.611568051603,-24.8107734492731,0.00113077479104779));
#49814=CARTESIAN_POINT('Ctrl Pts',(369.403995057531,0.413412695952972,2.88148094926035));
#49815=CARTESIAN_POINT('Ctrl Pts',(368.445565660651,0.347240656815754,2.40573134738565));
#49816=CARTESIAN_POINT('Ctrl Pts',(367.058003076544,0.214896578541317,0.429127078216204));
#49817=CARTESIAN_POINT('Ctrl Pts',(368.426799296739,0.0163804611296606,
-2.94632001420472));
#49818=CARTESIAN_POINT('Ctrl Pts',(372.004780269968,-0.182135656281995,
-3.6175583718889));
#49819=CARTESIAN_POINT('Ctrl Pts',(374.508790558812,-0.380651773693651,
-0.978876013732187));
#49820=CARTESIAN_POINT('Ctrl Pts',(373.64879697239,-0.579167891105306,2.55766308961752));
#49821=CARTESIAN_POINT('Ctrl Pts',(370.210870868906,-0.777684008516963,
3.75125713645417));
#49822=CARTESIAN_POINT('Ctrl Pts',(367.344120138506,-0.976200125928618,
1.50985201363752));
#49823=CARTESIAN_POINT('Ctrl Pts',(367.673512981428,-1.17471624334027,-2.11440641090759));
#49824=CARTESIAN_POINT('Ctrl Pts',(370.897565357316,-1.37323236075193,-3.80225470587514));
#49825=CARTESIAN_POINT('Ctrl Pts',(374.063670556472,-1.57174847816358,-2.00810758936603));
#49826=CARTESIAN_POINT('Ctrl Pts',(374.272408672299,-1.77026459557524,1.62504416509206));
#49827=CARTESIAN_POINT('Ctrl Pts',(371.332602492641,-1.9687807129869,3.77000274775842));
#49828=CARTESIAN_POINT('Ctrl Pts',(367.936479671958,-2.16729683039855,2.46246869320962));
#49829=CARTESIAN_POINT('Ctrl Pts',(367.194140510371,-2.36581294781021,-1.10014935901889));
#49830=CARTESIAN_POINT('Ctrl Pts',(369.78540720301,-2.56432906522186,-3.65527058599263));
#49831=CARTESIAN_POINT('Ctrl Pts',(373.337245985264,-2.76284518263352,-2.86296500849419));
#49832=CARTESIAN_POINT('Ctrl Pts',(374.596950954817,-2.96136130004518,0.551189689945338));
#49833=CARTESIAN_POINT('Ctrl Pts',(372.410908025683,-3.15987741745683,3.46057524628607));
#49834=CARTESIAN_POINT('Ctrl Pts',(368.781053843735,-3.35839353486848,3.20083187167307));
#49835=CARTESIAN_POINT('Ctrl Pts',(367.031539766512,-3.55690965228014,0.0098275299489643));
#49836=CARTESIAN_POINT('Ctrl Pts',(368.764537533245,-3.7554257696918,-3.19017666455396));
#49837=CARTESIAN_POINT('Ctrl Pts',(372.393000741445,-3.95394188710345,-3.46867775914217));
#49838=CARTESIAN_POINT('Ctrl Pts',(374.594051811918,-4.15245800451511,-0.570629740314608));
#49839=CARTESIAN_POINT('Ctrl Pts',(373.352010039771,-4.35097412192676,2.84999013879425));
#49840=CARTESIAN_POINT('Ctrl Pts',(369.804313655238,-4.54949023933842,3.6606432620171));
#49841=CARTESIAN_POINT('Ctrl Pts',(367.199875522236,-4.74800635675008,1.11894891838422));
#49842=CARTESIAN_POINT('Ctrl Pts',(367.923790541639,-4.94652247416173,-2.44745755988582));
#49843=CARTESIAN_POINT('Ctrl Pts',(371.31311110884,-5.14503859157339,-3.77252896046589));
#49844=CARTESIAN_POINT('Ctrl Pts',(374.263961920186,-5.34355470898505,-1.64279010012549));
#49845=CARTESIAN_POINT('Ctrl Pts',(374.074009933744,-5.5420708263967,1.99138468471137));
#49846=CARTESIAN_POINT('Ctrl Pts',(370.917209565446,-5.74058694380835,3.8018872554512));
#49847=CARTESIAN_POINT('Ctrl Pts',(367.68449854386,-5.93910306122002,2.13069379720876));
#49848=CARTESIAN_POINT('Ctrl Pts',(367.336332129874,-6.13761917863167,-1.4917485104219));
#49849=CARTESIAN_POINT('Ctrl Pts',(370.191554502588,-6.33613529604332,-3.74807590827464));
#49850=CARTESIAN_POINT('Ctrl Pts',(373.63540732516,-6.53465141345498,-2.57198668529261));
#49851=CARTESIAN_POINT('Ctrl Pts',(374.514075691705,-6.73316753086664,0.959479019705749));
#49852=CARTESIAN_POINT('Ctrl Pts',(372.022891826185,-6.93168364827829,3.61227208968389));
#49853=CARTESIAN_POINT('Ctrl Pts',(368.443234525303,-7.13019976568994,2.95701509263057));
#49854=CARTESIAN_POINT('Ctrl Pts',(367.053285852903,-7.32871588310161,-0.406220077862496));
#49855=CARTESIAN_POINT('Ctrl Pts',(369.125934363543,-7.52723200051325,-3.3974466281743));
#49856=CARTESIAN_POINT('Ctrl Pts',(372.763087977133,-7.72574811792492,-3.27735618269157));
#49857=CARTESIAN_POINT('Ctrl Pts',(374.633910600346,-7.92426423533656,-0.155925287024877));
#49858=CARTESIAN_POINT('Ctrl Pts',(373.025138461662,-8.12278035274823,3.10829902048574));
#49859=CARTESIAN_POINT('Ctrl Pts',(369.410054483599,-8.32129647015987,3.52600221115229));
#49860=CARTESIAN_POINT('Ctrl Pts',(367.099283807075,-8.51981258757154,0.714659648519558));
#49861=CARTESIAN_POINT('Ctrl Pts',(368.208986262136,-8.7183287049832,-2.75115462595943));
#49862=CARTESIAN_POINT('Ctrl Pts',(371.722917449212,-8.91684482239485,-3.69751382649478));
#49863=CARTESIAN_POINT('Ctrl Pts',(374.423086029239,-9.1153609398065,-1.25776019889706));
#49864=CARTESIAN_POINT('Ctrl Pts',(373.836728979282,-9.31387705721816,2.33382629371473));
#49865=CARTESIAN_POINT('Ctrl Pts',(370.500820931997,-9.51239317462982,3.78813906062597));
#49866=CARTESIAN_POINT('Ctrl Pts',(367.470323021388,-9.71090929204147,1.77334613386154));
#49867=CARTESIAN_POINT('Ctrl Pts',(367.520507587807,-9.90942540945314,-1.86544344967302));
#49868=CARTESIAN_POINT('Ctrl Pts',(370.605416559942,-10.1079415268648,-3.79589540649401));
#49869=CARTESIAN_POINT('Ctrl Pts',(373.899948982299,-10.3064576442765,-2.2501385556347));
#49870=CARTESIAN_POINT('Ctrl Pts',(374.387034731138,-10.5049737616881,1.35625238230104));
#49871=CARTESIAN_POINT('Ctrl Pts',(371.620609943024,-10.7034898790998,3.72061318718134));
#49872=CARTESIAN_POINT('Ctrl Pts',(368.134113815933,-10.9020059965114,2.67770720880823));
#49873=CARTESIAN_POINT('Ctrl Pts',(367.120413182867,-11.1005221139231,-0.817392095999423));
#49874=CARTESIAN_POINT('Ctrl Pts',(369.507835800956,-11.2990382313348,-3.56393926773715));
#49875=CARTESIAN_POINT('Ctrl Pts',(373.110025450149,-11.4975543487464,-3.0466986513945));
#49876=CARTESIAN_POINT('Ctrl Pts',(374.628165370627,-11.6960704661581,0.260650635541734));
#49877=CARTESIAN_POINT('Ctrl Pts',(372.6719719013,-11.8945865835697,3.32930102854965));
#49878=CARTESIAN_POINT('Ctrl Pts',(369.032889810631,-12.0931027009814,3.34904086963255));
#49879=CARTESIAN_POINT('Ctrl Pts',(367.043521254576,-12.291618818393,0.301792787818268));
#49880=CARTESIAN_POINT('Ctrl Pts',(368.525692114965,-12.4901349358047,-3.02183138837245));
#49881=CARTESIAN_POINT('Ctrl Pts',(372.122058511734,-12.6886510532163,-3.57811986041968));
#49882=CARTESIAN_POINT('Ctrl Pts',(374.539136508866,-12.887167170628,-0.857634227351326));
#49883=CARTESIAN_POINT('Ctrl Pts',(373.563412054284,-13.0856832880397,2.6482565171925));
#49884=CARTESIAN_POINT('Ctrl Pts',(370.088435043248,-13.2841994054513,3.72892431847192));
#49885=CARTESIAN_POINT('Ctrl Pts',(367.296523321393,-13.482715522863,1.39471416055649));
#49886=CARTESIAN_POINT('Ctrl Pts',(367.744456535802,-13.6812316402746,-2.21674869532011));
#49887=CARTESIAN_POINT('Ctrl Pts',(371.022025969311,-13.8797477576863,-3.7981552630539));
#49888=CARTESIAN_POINT('Ctrl Pts',(374.127695880695,-14.0782638750979,-1.90128348945687));
#49889=CARTESIAN_POINT('Ctrl Pts',(374.217352841214,-14.2767799925096,1.73674753753793));
#49890=CARTESIAN_POINT('Ctrl Pts',(371.208890711882,-14.4752961099213,3.78429820609665));
#49891=CARTESIAN_POINT('Ctrl Pts',(367.857401883721,-14.6738122273329,2.36626056249685));
#49892=CARTESIAN_POINT('Ctrl Pts',(367.232116073486,-14.8723283447446,-1.21875349318896));
#49893=CARTESIAN_POINT('Ctrl Pts',(369.905658131992,-15.0708444621562,-3.68765628296195));
#49894=CARTESIAN_POINT('Ctrl Pts',(373.429649098221,-15.2693605795679,-2.77947359545888));
#49895=CARTESIAN_POINT('Ctrl Pts',(374.576885078718,-15.4678766969795,0.674098139571492));
#49896=CARTESIAN_POINT('Ctrl Pts',(372.296749185285,-15.6663928143912,3.51034362108856));
#49897=CARTESIAN_POINT('Ctrl Pts',(368.677346496345,-15.8649089318029,3.1318831882287));
#49898=CARTESIAN_POINT('Ctrl Pts',(367.03325714609,-16.0634250492145,-0.114696293675766));
#49899=CARTESIAN_POINT('Ctrl Pts',(368.870106887587,-16.2619411666262,-3.25623909158683));
#49900=CARTESIAN_POINT('Ctrl Pts',(372.505743668162,-16.4604572840378,-3.41578006965798));
#49901=CARTESIAN_POINT('Ctrl Pts',(374.610720481307,-16.6589734014495,-0.447214634962899));
#49902=CARTESIAN_POINT('Ctrl Pts',(373.257339602449,-16.8574895188611,2.93090145550684));
#49903=CARTESIAN_POINT('Ctrl Pts',(369.685001496413,-17.0560056362728,3.62495374468069));
#49904=CARTESIAN_POINT('Ctrl Pts',(367.165185447629,-17.2545217536844,0.999342348407682));
#49905=CARTESIAN_POINT('Ctrl Pts',(368.005491061591,-17.4530378710961,-2.54144776102994));
#49906=CARTESIAN_POINT('Ctrl Pts',(371.43638244134,-17.6515539885078,-3.75482835437887));
#49907=CARTESIAN_POINT('Ctrl Pts',(374.315914523774,-17.8500701059194,-1.52960856519631));
#49908=CARTESIAN_POINT('Ctrl Pts',(374.007066602312,-18.0485862233311,2.09639765175277));
#49909=CARTESIAN_POINT('Ctrl Pts',(370.792675728515,-18.2471023407427,3.80256277693868));
#49910=CARTESIAN_POINT('Ctrl Pts',(367.616419920411,-18.4456184581544,2.02641324341738));
#49911=CARTESIAN_POINT('Ctrl Pts',(367.387053828267,-18.644134575566,-1.60548699195738));
#49912=CARTESIAN_POINT('Ctrl Pts',(370.314626556266,-18.8426506929777,-3.76711277970054));
#49913=CARTESIAN_POINT('Ctrl Pts',(373.71812268844,-19.0411668103893,-2.47888834187282));
#49914=CARTESIAN_POINT('Ctrl Pts',(374.480685208313,-19.239682927801,1.07945488597672));
#49915=CARTESIAN_POINT('Ctrl Pts',(371.903973865648,-19.4381990452126,3.64925386267693));
#49916=CARTESIAN_POINT('Ctrl Pts',(368.34769189384,-19.6367151626243,2.87713556806726));
#49917=CARTESIAN_POINT('Ctrl Pts',(367.068614674954,-19.8352312800359,-0.5298087507752));
#49918=CARTESIAN_POINT('Ctrl Pts',(369.238096795542,-20.0337473974476,-3.45156429385787));
#49919=CARTESIAN_POINT('Ctrl Pts',(372.869367797239,-20.2322635148593,-3.2124429119896));
#49920=CARTESIAN_POINT('Ctrl Pts',(374.63697877132,-20.4307796322709,-0.0314274191916297));
#49921=CARTESIAN_POINT('Ctrl Pts',(372.922185210146,-20.6292957496826,3.17836870779575));
#49922=CARTESIAN_POINT('Ctrl Pts',(369.295362440493,-20.8278118670942,3.47747522804387));
#49923=CARTESIAN_POINT('Ctrl Pts',(367.077885760591,-21.0263279845059,0.591976089517751));
#49924=CARTESIAN_POINT('Ctrl Pts',(368.300478142822,-21.2248441019175,-2.83564350463414));
#49925=CARTESIAN_POINT('Ctrl Pts',(371.843512719386,-21.4233602193292,-3.66643468906968));
#49926=CARTESIAN_POINT('Ctrl Pts',(374.462345862869,-21.6218763367409,-1.13957478593675));
#49927=CARTESIAN_POINT('Ctrl Pts',(373.758699908593,-21.8203924541525,2.43088614876417));
#49928=CARTESIAN_POINT('Ctrl Pts',(370.37696061784,-22.0189085715642,3.77518754079788));
#49929=CARTESIAN_POINT('Ctrl Pts',(367.414060130091,-22.2174246889758,1.66224450876473));
#49930=CARTESIAN_POINT('Ctrl Pts',(367.583367130122,-22.4159408063875,-1.9729514909897));
#49931=CARTESIAN_POINT('Ctrl Pts',(370.729831874048,-22.6144569237992,-3.80135383516712));
#49932=CARTESIAN_POINT('Ctrl Pts',(373.971985147174,-22.8129730412108,-2.14855322744992));
#49933=CARTESIAN_POINT('Ctrl Pts',(374.340717718146,-23.0114891586225,1.47186105312981));
#49934=CARTESIAN_POINT('Ctrl Pts',(371.498365692146,-23.2100052760341,3.74435329032221));
#49935=CARTESIAN_POINT('Ctrl Pts',(368.047871176115,-23.4085213934458,2.58787882708531));
#49936=CARTESIAN_POINT('Ctrl Pts',(367.149193215696,-23.6070375108574,-0.938610460621719));
#49937=CARTESIAN_POINT('Ctrl Pts',(369.625195865162,-23.8055536282691,-3.60536270908208));
#49938=CARTESIAN_POINT('Ctrl Pts',(373.208668628663,-24.0040697456807,-2.97075606325937));
#49939=CARTESIAN_POINT('Ctrl Pts',(374.617384679032,-24.2025858630924,0.38516659491335));
#49940=CARTESIAN_POINT('Ctrl Pts',(372.56241093661,-24.4011019805041,3.38679865628135));
#49941=CARTESIAN_POINT('Ctrl Pts',(368.923295180967,-24.5996180979157,3.29012759206182));
#49942=CARTESIAN_POINT('Ctrl Pts',(367.037251697264,-24.7981786416692,0.173073691602409));
#49943=CARTESIAN_POINT('Ctrl Pts',(368.095727704402,-24.9305671462855,-1.99893471883147));
#49944=CARTESIAN_POINT('Ctrl Pts',(368.967855604038,-24.9967836117645,-2.62012863412635));
#49945=CARTESIAN_POINT('Ctrl Pts',(369.297428771816,0.27503400748034,3.09616586027907));
#49946=CARTESIAN_POINT('Ctrl Pts',(368.267591535214,0.208861968343121,2.58497050577087));
#49947=CARTESIAN_POINT('Ctrl Pts',(366.776648517521,0.0765178900686841,
0.461099216927136));
#49948=CARTESIAN_POINT('Ctrl Pts',(368.247426982232,-0.121998227342972,
-3.16583576364755));
#49949=CARTESIAN_POINT('Ctrl Pts',(372.091985642559,-0.320514344754628,
-3.88708477544654));
#49950=CARTESIAN_POINT('Ctrl Pts',(374.782557368216,-0.519030462166284,
-1.05180722986966));
#49951=CARTESIAN_POINT('Ctrl Pts',(373.858489908038,-0.71754657957794,2.74822193157386));
#49952=CARTESIAN_POINT('Ctrl Pts',(370.164420913931,-0.916062696989595,
4.03074477448791));
#49953=CARTESIAN_POINT('Ctrl Pts',(367.084082748353,-1.11457881440125,1.62234362850746));
#49954=CARTESIAN_POINT('Ctrl Pts',(367.438017024802,-1.3130949318129,-2.27194038742045));
#49955=CARTESIAN_POINT('Ctrl Pts',(370.902277616403,-1.51161104922456,-4.08554192087854));
#49956=CARTESIAN_POINT('Ctrl Pts',(374.304273673394,-1.71012716663622,-2.15772176580187));
#49957=CARTESIAN_POINT('Ctrl Pts',(374.528563835066,-1.90864328404787,1.7461181781178));
#49958=CARTESIAN_POINT('Ctrl Pts',(371.369727219598,-2.10715940145953,4.05088702868714));
#49959=CARTESIAN_POINT('Ctrl Pts',(367.720576064387,-2.30567551887118,2.64593507094979));
#49960=CARTESIAN_POINT('Ctrl Pts',(366.922928879025,-2.50419163628284,-1.18211605302352));
#49961=CARTESIAN_POINT('Ctrl Pts',(369.707258052079,-2.7027077536945,-3.92760674032486));
#49962=CARTESIAN_POINT('Ctrl Pts',(373.523726795923,-2.90122387110615,-3.07627038823516));
#49963=CARTESIAN_POINT('Ctrl Pts',(374.877286159816,-3.09973998851781,0.592256110867064));
#49964=CARTESIAN_POINT('Ctrl Pts',(372.52837197108,-3.29825610592946,3.71840561265137));
#49965=CARTESIAN_POINT('Ctrl Pts',(368.628075285508,-3.49677222334112,3.4393100423278));
#49966=CARTESIAN_POINT('Ctrl Pts',(366.748213556987,-3.69528834075277,0.0105597306575114));
#49967=CARTESIAN_POINT('Ctrl Pts',(368.610328426315,-3.89380445816443,-3.4278609683629));
#49968=CARTESIAN_POINT('Ctrl Pts',(372.509130503555,-4.09232057557608,-3.72711180371402));
#49969=CARTESIAN_POINT('Ctrl Pts',(374.874171016102,-4.29083669298774,-0.613144543355595));
#49970=CARTESIAN_POINT('Ctrl Pts',(373.539590847196,-4.4893528103994,3.06232882508966));
#49971=CARTESIAN_POINT('Ctrl Pts',(369.727573130664,-4.68786892781105,3.93337970789892));
#49972=CARTESIAN_POINT('Ctrl Pts',(366.929091178293,-4.88638504522271,1.20231627468743));
#49973=CARTESIAN_POINT('Ctrl Pts',(367.706941529652,-5.08490116263436,-2.62980553223698));
#49974=CARTESIAN_POINT('Ctrl Pts',(371.348783629077,-5.28341728004602,-4.05360145702397));
#49975=CARTESIAN_POINT('Ctrl Pts',(374.519487757179,-5.48193339745768,-1.76518627510575));
#49976=CARTESIAN_POINT('Ctrl Pts',(374.315383386591,-5.68044951486934,2.13975292013245));
#49977=CARTESIAN_POINT('Ctrl Pts',(370.923385417439,-5.87896563228098,4.0851470935387));
#49978=CARTESIAN_POINT('Ctrl Pts',(367.449821067221,-6.07748174969265,2.28944126641531));
#49979=CARTESIAN_POINT('Ctrl Pts',(367.07571449367,-6.2759978671043,-1.60289132269847));
#49980=CARTESIAN_POINT('Ctrl Pts',(370.143665380582,-6.47451398451596,-4.02732652871198));
#49981=CARTESIAN_POINT('Ctrl Pts',(373.844102664337,-6.67303010192761,-2.76361270760422));
#49982=CARTESIAN_POINT('Ctrl Pts',(374.788236270252,-6.87154621933927,1.03096506163937));
#49983=CARTESIAN_POINT('Ctrl Pts',(372.111446601358,-7.07006233675092,3.88140463846864));
#49984=CARTESIAN_POINT('Ctrl Pts',(368.265086718486,-7.26857845416258,3.17732767953328));
#49985=CARTESIAN_POINT('Ctrl Pts',(366.771579836851,-7.46709457157424,-0.436485529137551));
#49986=CARTESIAN_POINT('Ctrl Pts',(368.998651149138,-7.66561068898589,-3.65057359305935));
#49987=CARTESIAN_POINT('Ctrl Pts',(372.906791110945,-7.86412680639755,-3.52153580173033));
#49988=CARTESIAN_POINT('Ctrl Pts',(374.916999485952,-8.0626429238092,-0.167542509890492));
#49989=CARTESIAN_POINT('Ctrl Pts',(373.188365682548,-8.26115904122086,3.33988302551057));
#49990=CARTESIAN_POINT('Ctrl Pts',(369.303939655786,-8.45967515863252,3.78870721746071));
#49991=CARTESIAN_POINT('Ctrl Pts',(366.821004871359,-8.65819127604416,0.767905408513408));
#49992=CARTESIAN_POINT('Ctrl Pts',(368.013385774417,-8.85670739345583,-2.95612956644076));
#49993=CARTESIAN_POINT('Ctrl Pts',(371.789122615428,-9.05522351086748,-3.97299731599531));
#49994=CARTESIAN_POINT('Ctrl Pts',(374.690467417526,-9.25373962827913,-1.3514696979838));
#49995=CARTESIAN_POINT('Ctrl Pts',(374.060423800379,-9.45225574569079,2.50770816176172));
#49996=CARTESIAN_POINT('Ctrl Pts',(370.47597372387,-9.65077186310245,4.07037458863311));
#49997=CARTESIAN_POINT('Ctrl Pts',(367.219688384595,-9.84928798051411,1.90546939396889));
#49998=CARTESIAN_POINT('Ctrl Pts',(367.273611955148,-10.0478040979258,-2.00442842582086));
#49999=CARTESIAN_POINT('Ctrl Pts',(370.588362255352,-10.2463202153375,-4.07870882151544));
#50000=CARTESIAN_POINT('Ctrl Pts',(374.128354013515,-10.4448363327491,-2.41778526373467));
#50001=CARTESIAN_POINT('Ctrl Pts',(374.651730115297,-10.6433524501608,1.45730004742194));
#50002=CARTESIAN_POINT('Ctrl Pts',(371.679192682353,-10.8418685675723,3.99781769593581));
#50003=CARTESIAN_POINT('Ctrl Pts',(367.932934952118,-11.0403846849841,2.87720994506778));
#50004=CARTESIAN_POINT('Ctrl Pts',(366.843708492561,-11.2389008023958,-0.878291943156831));
#50005=CARTESIAN_POINT('Ctrl Pts',(369.409006176061,-11.4374169198074,-3.82947077672271));
#50006=CARTESIAN_POINT('Ctrl Pts',(373.279577181204,-11.6359330372191,-3.2736931172241));
#50007=CARTESIAN_POINT('Ctrl Pts',(374.910826207548,-11.8344491546307,0.280070426782248));
#50008=CARTESIAN_POINT('Ctrl Pts',(372.808886426414,-12.0329652720424,3.57735080144582));
#50009=CARTESIAN_POINT('Ctrl Pts',(368.898674306229,-12.231481389454,3.59856136057304));
#50010=CARTESIAN_POINT('Ctrl Pts',(366.761087726538,-12.4299975068657,0.324277877582813));
#50011=CARTESIAN_POINT('Ctrl Pts',(368.353687815814,-12.6285136242772,-3.24697311727847));
#50012=CARTESIAN_POINT('Ctrl Pts',(372.218001706763,-12.827029741689,-3.84470789531392));
#50013=CARTESIAN_POINT('Ctrl Pts',(374.8151642451,-13.0255458591006,-0.921532316919773));
#50014=CARTESIAN_POINT('Ctrl Pts',(373.766743381484,-13.2240619765122,2.84556502790608));
#50015=CARTESIAN_POINT('Ctrl Pts',(370.032862999737,-13.422578093924,4.00674804856188));
#50016=CARTESIAN_POINT('Ctrl Pts',(367.032939727526,-13.6210942113356,1.49862742277415));
#50017=CARTESIAN_POINT('Ctrl Pts',(367.51424623295,-13.8196103287473,-2.38190768987384));
#50018=CARTESIAN_POINT('Ctrl Pts',(371.036011173762,-14.0181264461589,-4.08113704882393));
#50019=CARTESIAN_POINT('Ctrl Pts',(374.373069208241,-14.2166425635706,-2.04293872991932));
#50020=CARTESIAN_POINT('Ctrl Pts',(374.469406065983,-14.4151586809822,1.86614401703017));
#50021=CARTESIAN_POINT('Ctrl Pts',(371.236798285191,-14.6136747983939,4.06624757100662));
#50022=CARTESIAN_POINT('Ctrl Pts',(367.635606580794,-14.8121909158055,2.54255894768561));
#50023=CARTESIAN_POINT('Ctrl Pts',(366.963733813749,-15.0107070332172,-1.30955679532639));
#50024=CARTESIAN_POINT('Ctrl Pts',(369.83646828374,-15.2092231506288,-3.96240533559008));
#50025=CARTESIAN_POINT('Ctrl Pts',(373.623014408354,-15.4077392680404,-2.98655844246201));
#50026=CARTESIAN_POINT('Ctrl Pts',(374.855725274414,-15.6062553854522,0.724321861907345));
#50027=CARTESIAN_POINT('Ctrl Pts',(372.405707719428,-15.8047715028638,3.77188198320471));
#50028=CARTESIAN_POINT('Ctrl Pts',(368.516641215978,-16.0032876202755,3.36522433308636));
#50029=CARTESIAN_POINT('Ctrl Pts',(366.750058890034,-16.2018037376871,-0.123241747918035));
#50030=CARTESIAN_POINT('Ctrl Pts',(368.723763231736,-16.4003198550988,-3.49884538048572));
#50031=CARTESIAN_POINT('Ctrl Pts',(372.630273348791,-16.5988359725103,-3.67027296870085));
#50032=CARTESIAN_POINT('Ctrl Pts',(374.892081585703,-16.7973520899221,-0.480534388174527));
#50033=CARTESIAN_POINT('Ctrl Pts',(373.437866983261,-16.9958682073337,3.14926844430875));
#50034=CARTESIAN_POINT('Ctrl Pts',(369.599371612288,-17.1943843247454,3.89503114093192));
#50035=CARTESIAN_POINT('Ctrl Pts',(366.891816517596,-17.3929004421571,1.07379841003817));
#50036=CARTESIAN_POINT('Ctrl Pts',(367.794729151745,-17.5914165595686,-2.73079847895693));
#50037=CARTESIAN_POINT('Ctrl Pts',(371.481239299601,-17.7899326769803,-4.03458206621836));
#50038=CARTESIAN_POINT('Ctrl Pts',(374.575311092616,-17.9884487943919,-1.64357214312557));
#50039=CARTESIAN_POINT('Ctrl Pts',(374.243452438233,-18.1869649118037,2.25258988458425));
#50040=CARTESIAN_POINT('Ctrl Pts',(370.789573179515,-18.3854810292153,4.08587294479514));
#50041=CARTESIAN_POINT('Ctrl Pts',(367.376670241846,-18.5839971466269,2.17739128370667));
#50042=CARTESIAN_POINT('Ctrl Pts',(367.130215215246,-18.7825132640387,-1.72510389662527));
#50043=CARTESIAN_POINT('Ctrl Pts',(370.275906925004,-18.9810293814502,-4.04778174338571));
#50044=CARTESIAN_POINT('Ctrl Pts',(373.932980740722,-19.179545498862,-2.66357806652187));
#50045=CARTESIAN_POINT('Ctrl Pts',(374.752358026892,-19.3780616162735,1.15987973702563));
#50046=CARTESIAN_POINT('Ctrl Pts',(371.983668651035,-19.5765777336853,3.92114174067749));
#50047=CARTESIAN_POINT('Ctrl Pts',(368.162425677533,-19.7750938510969,3.09149672619948));
#50048=CARTESIAN_POINT('Ctrl Pts',(366.788050733709,-19.9736099685086,-0.569282183541161));
#50049=CARTESIAN_POINT('Ctrl Pts',(369.119170249864,-20.1721260859203,-3.70872329867184));
#50050=CARTESIAN_POINT('Ctrl Pts',(373.020989315425,-20.3706422033319,-3.45178616389979));
#50051=CARTESIAN_POINT('Ctrl Pts',(374.920296251189,-20.5691583207435,-0.0337689209442362));
#50052=CARTESIAN_POINT('Ctrl Pts',(373.07774189285,-20.7676744381551,3.41517325907793));
#50053=CARTESIAN_POINT('Ctrl Pts',(369.180702475126,-20.9661905555669,3.7365647285641));
#50054=CARTESIAN_POINT('Ctrl Pts',(366.798012562137,-21.1647066729785,0.636081303586939));
#50055=CARTESIAN_POINT('Ctrl Pts',(368.111694263164,-21.3632227903902,-3.04691329409063));
#50056=CARTESIAN_POINT('Ctrl Pts',(371.918702843443,-21.5617389078019,-3.93960262557153));
#50057=CARTESIAN_POINT('Ctrl Pts',(374.732652307415,-21.7602550252134,-1.22447887373956));
#50058=CARTESIAN_POINT('Ctrl Pts',(373.976581169097,-21.9587711426251,2.61199946713539));
#50059=CARTESIAN_POINT('Ctrl Pts',(370.342885189575,-22.1572872600367,4.05645811504312));
#50060=CARTESIAN_POINT('Ctrl Pts',(367.159233623208,-22.3558033774484,1.78609013562795));
#50061=CARTESIAN_POINT('Ctrl Pts',(367.341154851434,-22.5543194948601,-2.11994636020653));
#50062=CARTESIAN_POINT('Ctrl Pts',(370.7220471399,-22.7528356122718,-4.08457393074435));
#50063=CARTESIAN_POINT('Ctrl Pts',(374.205757237175,-22.9513517296833,-2.30863131457819));
#50064=CARTESIAN_POINT('Ctrl Pts',(374.601962250472,-23.149867847095,1.58152214920754));
#50065=CARTESIAN_POINT('Ctrl Pts',(371.547840616229,-23.3483839645068,4.02332655688563));
#50066=CARTESIAN_POINT('Ctrl Pts',(367.840266799244,-23.5469000819183,2.78068889437474));
#50067=CARTESIAN_POINT('Ctrl Pts',(366.874632783463,-23.7454161993299,-1.00854168930863));
#50068=CARTESIAN_POINT('Ctrl Pts',(369.535110158892,-23.9439323167417,-3.87398047405052));
#50069=CARTESIAN_POINT('Ctrl Pts',(373.385569775652,-24.1424484341533,-3.19209242200327));
#50070=CARTESIAN_POINT('Ctrl Pts',(374.899242299879,-24.340964551565,0.41386345517803));
#50071=CARTESIAN_POINT('Ctrl Pts',(372.691162615477,-24.5394806689767,3.63913229338162));
#50072=CARTESIAN_POINT('Ctrl Pts',(368.780914322106,-24.7379967863883,3.53525874572201));
#50073=CARTESIAN_POINT('Ctrl Pts',(366.754351055484,-24.9365573301418,0.185968557380015));
#50074=CARTESIAN_POINT('Ctrl Pts',(367.891688881044,-25.0689458347581,-2.14786546999769));
#50075=CARTESIAN_POINT('Ctrl Pts',(368.828794722171,-25.1351623002372,-2.81534147522438));
#50076=CARTESIAN_POINT('Ctrl Pts',(369.190862486101,0.136655319007707,3.3108507712978));
#50077=CARTESIAN_POINT('Ctrl Pts',(368.089617409777,0.0704832798704884,
2.76420966415609));
#50078=CARTESIAN_POINT('Ctrl Pts',(366.495293958499,-0.0618607984039484,
0.493071355638064));
#50079=CARTESIAN_POINT('Ctrl Pts',(368.068054667726,-0.260376915815605,
-3.38535151309038));
#50080=CARTESIAN_POINT('Ctrl Pts',(372.179191015148,-0.458893033227261,
-4.15661117900418));
#50081=CARTESIAN_POINT('Ctrl Pts',(375.056324177621,-0.657409150638917,
-1.12473844600715));
#50082=CARTESIAN_POINT('Ctrl Pts',(374.068182843686,-0.855925268050571,
2.93878077353021));
#50083=CARTESIAN_POINT('Ctrl Pts',(370.117970958957,-1.05444138546223,4.31023241252165));
#50084=CARTESIAN_POINT('Ctrl Pts',(366.8240453582,-1.25295750287388,1.73483524337741));
#50085=CARTESIAN_POINT('Ctrl Pts',(367.202521068174,-1.45147362028554,-2.4294743639333));
#50086=CARTESIAN_POINT('Ctrl Pts',(370.90698987549,-1.6499897376972,-4.36882913588193));
#50087=CARTESIAN_POINT('Ctrl Pts',(374.544876790316,-1.84850585510885,-2.30733594223771));
#50088=CARTESIAN_POINT('Ctrl Pts',(374.784718997833,-2.04702197252051,1.86719219114356));
#50089=CARTESIAN_POINT('Ctrl Pts',(371.406851946557,-2.24553808993216,4.33177130961586));
#50090=CARTESIAN_POINT('Ctrl Pts',(367.504672456816,-2.44405420734382,2.82940144868998));
#50091=CARTESIAN_POINT('Ctrl Pts',(366.651717247679,-2.64257032475548,-1.26408274702814));
#50092=CARTESIAN_POINT('Ctrl Pts',(369.629108901149,-2.84108644216713,-4.19994289465708));
#50093=CARTESIAN_POINT('Ctrl Pts',(373.71020760658,-3.03960255957878,-3.28957576797611));
#50094=CARTESIAN_POINT('Ctrl Pts',(375.157621364815,-3.23811867699044,0.633322531788789));
#50095=CARTESIAN_POINT('Ctrl Pts',(372.645835916477,-3.4366347944021,3.97623597901668));
#50096=CARTESIAN_POINT('Ctrl Pts',(368.475096727281,-3.63515091181375,3.67778821298252));
#50097=CARTESIAN_POINT('Ctrl Pts',(366.464887347464,-3.83366702922541,0.0112919313660596));
#50098=CARTESIAN_POINT('Ctrl Pts',(368.456119319384,-4.03218314663707,-3.66554527217185));
#50099=CARTESIAN_POINT('Ctrl Pts',(372.625260265666,-4.23069926404872,-3.98554584828585));
#50100=CARTESIAN_POINT('Ctrl Pts',(375.154290220285,-4.42921538146038,-0.655659346396582));
#50101=CARTESIAN_POINT('Ctrl Pts',(373.727171654621,-4.62773149887203,3.27466751138507));
#50102=CARTESIAN_POINT('Ctrl Pts',(369.650832606091,-4.82624761628369,4.20611615378073));
#50103=CARTESIAN_POINT('Ctrl Pts',(366.658306834349,-5.02476373369535,1.28568363099063));
#50104=CARTESIAN_POINT('Ctrl Pts',(367.490092517666,-5.22327985110699,-2.81215350458813));
#50105=CARTESIAN_POINT('Ctrl Pts',(371.384456149316,-5.42179596851866,-4.33467395358205));
#50106=CARTESIAN_POINT('Ctrl Pts',(374.775013594174,-5.62031208593031,-1.887582450086));
#50107=CARTESIAN_POINT('Ctrl Pts',(374.556756839438,-5.81882820334197,2.28812115555352));
#50108=CARTESIAN_POINT('Ctrl Pts',(370.929561269431,-6.01734432075362,4.36840693162621));
#50109=CARTESIAN_POINT('Ctrl Pts',(367.215143590582,-6.21586043816528,2.44818873562185));
#50110=CARTESIAN_POINT('Ctrl Pts',(366.815096857467,-6.41437655557694,-1.71403413497503));
#50111=CARTESIAN_POINT('Ctrl Pts',(370.095776258576,-6.61289267298859,-4.30657714914931));
#50112=CARTESIAN_POINT('Ctrl Pts',(374.052798003513,-6.81140879040025,-2.95523872991583));
#50113=CARTESIAN_POINT('Ctrl Pts',(375.0623968488,-7.0099249078119,1.10245110357299));
#50114=CARTESIAN_POINT('Ctrl Pts',(372.20000137653,-7.20844102522356,4.1505371872534));
#50115=CARTESIAN_POINT('Ctrl Pts',(368.086938911671,-7.40695714263521,3.397640266436));
#50116=CARTESIAN_POINT('Ctrl Pts',(366.489873820798,-7.60547326004687,-0.466750980412602));
#50117=CARTESIAN_POINT('Ctrl Pts',(368.871367934734,-7.80398937745853,-3.90370055794442));
#50118=CARTESIAN_POINT('Ctrl Pts',(373.050494244756,-8.00250549487018,-3.76571542076907));
#50119=CARTESIAN_POINT('Ctrl Pts',(375.200088371559,-8.20102161228184,-0.179159732756115));
#50120=CARTESIAN_POINT('Ctrl Pts',(373.351592903432,-8.3995377296935,3.57146703053541));
#50121=CARTESIAN_POINT('Ctrl Pts',(369.197824827974,-8.59805384710515,4.05141222376914));
#50122=CARTESIAN_POINT('Ctrl Pts',(366.542725935641,-8.7965699645168,0.82115116850726));
#50123=CARTESIAN_POINT('Ctrl Pts',(367.817785286697,-8.99508608192846,-3.1611045069221));
#50124=CARTESIAN_POINT('Ctrl Pts',(371.855327781645,-9.19360219934012,-4.24848080549583));
#50125=CARTESIAN_POINT('Ctrl Pts',(374.957848805812,-9.39211831675177,-1.44517919707054));
#50126=CARTESIAN_POINT('Ctrl Pts',(374.284118621476,-9.59063443416343,2.68159002980871));
#50127=CARTESIAN_POINT('Ctrl Pts',(370.451126515743,-9.78915055157509,4.35261011664025));
#50128=CARTESIAN_POINT('Ctrl Pts',(366.969053747804,-9.98766666898675,2.03759265407625));
#50129=CARTESIAN_POINT('Ctrl Pts',(367.026716322489,-10.1861827863983,-2.1434134019687));
#50130=CARTESIAN_POINT('Ctrl Pts',(370.57130795076,-10.38469890381,-4.36152223653687));
#50131=CARTESIAN_POINT('Ctrl Pts',(374.35675904473,-10.5832150212217,-2.58543197183465));
#50132=CARTESIAN_POINT('Ctrl Pts',(374.916425499454,-10.7817311386333,1.55834771254285));
#50133=CARTESIAN_POINT('Ctrl Pts',(371.737775421683,-10.980247256045,4.27502220469027));
#50134=CARTESIAN_POINT('Ctrl Pts',(367.731756088302,-11.1787633734566,3.07671268132734));
#50135=CARTESIAN_POINT('Ctrl Pts',(366.567003802255,-11.3772794908683,-0.939191790314244));
#50136=CARTESIAN_POINT('Ctrl Pts',(369.310176551165,-11.5757956082799,-4.09500228570826));
#50137=CARTESIAN_POINT('Ctrl Pts',(373.44912891226,-11.7743117256916,-3.50068758305369));
#50138=CARTESIAN_POINT('Ctrl Pts',(375.193487044471,-11.9728278431033,0.299490218022766));
#50139=CARTESIAN_POINT('Ctrl Pts',(372.945800951528,-12.1713439605149,3.82540057434197));
#50140=CARTESIAN_POINT('Ctrl Pts',(368.764458801828,-12.3698600779266,3.84808185151355));
#50141=CARTESIAN_POINT('Ctrl Pts',(366.478654198501,-12.5683761953382,0.346762967347356));
#50142=CARTESIAN_POINT('Ctrl Pts',(368.181683516663,-12.7668923127499,-3.4721148461845));
#50143=CARTESIAN_POINT('Ctrl Pts',(372.313944901792,-12.9654084301615,-4.11129593020815));
#50144=CARTESIAN_POINT('Ctrl Pts',(375.091191981334,-13.1639245475732,-0.985430406488218));
#50145=CARTESIAN_POINT('Ctrl Pts',(373.970074708685,-13.3624406649849,3.04287353861967));
#50146=CARTESIAN_POINT('Ctrl Pts',(369.977290956225,-13.5609567823965,4.28457177865185));
#50147=CARTESIAN_POINT('Ctrl Pts',(366.769356133657,-13.7594728998082,1.60254068499181));
#50148=CARTESIAN_POINT('Ctrl Pts',(367.284035930099,-13.9579890172198,-2.54706668442758));
#50149=CARTESIAN_POINT('Ctrl Pts',(371.049996378214,-14.1565051346315,-4.36411883459395));
#50150=CARTESIAN_POINT('Ctrl Pts',(374.618442535786,-14.3550212520431,-2.18459397038178));
#50151=CARTESIAN_POINT('Ctrl Pts',(374.721459290751,-14.5535373694548,1.99554049652239));
#50152=CARTESIAN_POINT('Ctrl Pts',(371.2647058585,-14.7520534868664,4.34819693591658));
#50153=CARTESIAN_POINT('Ctrl Pts',(367.413811277865,-14.9505696042781,2.71885733287438));
#50154=CARTESIAN_POINT('Ctrl Pts',(366.69535155401,-15.1490857216897,-1.40036009746382));
#50155=CARTESIAN_POINT('Ctrl Pts',(369.767278435489,-15.3476018391014,-4.2371543882182));
#50156=CARTESIAN_POINT('Ctrl Pts',(373.816379718487,-15.5461179565131,-3.19364328946513));
#50157=CARTESIAN_POINT('Ctrl Pts',(375.134565470109,-15.7446340739247,0.774545584243195));
#50158=CARTESIAN_POINT('Ctrl Pts',(372.514666253572,-15.9431501913364,4.03342034532087));
#50159=CARTESIAN_POINT('Ctrl Pts',(368.355935935611,-16.141666308748,3.59856547794402));
#50160=CARTESIAN_POINT('Ctrl Pts',(366.466860633978,-16.3401824261597,-0.1317872021603));
#50161=CARTESIAN_POINT('Ctrl Pts',(368.577419575885,-16.5386985435713,-3.74145166938463));
#50162=CARTESIAN_POINT('Ctrl Pts',(372.754803029422,-16.737214660983,-3.92476586774372));
#50163=CARTESIAN_POINT('Ctrl Pts',(375.173442690099,-16.9357307783947,-0.513854141386156));
#50164=CARTESIAN_POINT('Ctrl Pts',(373.618394364073,-17.1342468958063,3.36763543311066));
#50165=CARTESIAN_POINT('Ctrl Pts',(369.513741728162,-17.332763013218,4.16510853718315));
#50166=CARTESIAN_POINT('Ctrl Pts',(366.618447587562,-17.5312791306296,1.14825447166867));
#50167=CARTESIAN_POINT('Ctrl Pts',(367.5839672419,-17.7297952480413,-2.9201491968839));
#50168=CARTESIAN_POINT('Ctrl Pts',(371.526096157864,-17.9283113654529,-4.31433577805786));
#50169=CARTESIAN_POINT('Ctrl Pts',(374.834707661457,-18.1268274828646,-1.75753572105482));
#50170=CARTESIAN_POINT('Ctrl Pts',(374.479838274154,-18.3253436002762,2.40878211741571));
#50171=CARTESIAN_POINT('Ctrl Pts',(370.786470630515,-18.5238597176879,4.3691831126516));
#50172=CARTESIAN_POINT('Ctrl Pts',(367.136920563282,-18.7223758350996,2.32836932399598));
#50173=CARTESIAN_POINT('Ctrl Pts',(366.873376602224,-18.9208919525112,-1.84472080129315));
#50174=CARTESIAN_POINT('Ctrl Pts',(370.237187293741,-19.1194080699229,-4.32845070707088));
#50175=CARTESIAN_POINT('Ctrl Pts',(374.147838793003,-19.3179241873345,-2.84826779117091));
#50176=CARTESIAN_POINT('Ctrl Pts',(375.024030845472,-19.5164403047462,1.24030458807455));
#50177=CARTESIAN_POINT('Ctrl Pts',(372.063363436422,-19.7149564221578,4.19302961867807));
#50178=CARTESIAN_POINT('Ctrl Pts',(367.977159461227,-19.9134725395695,3.30585788433169));
#50179=CARTESIAN_POINT('Ctrl Pts',(366.507486792462,-20.1119886569812,-0.608755616307119));
#50180=CARTESIAN_POINT('Ctrl Pts',(369.000243704185,-20.3105047743928,-3.96588230348581));
#50181=CARTESIAN_POINT('Ctrl Pts',(373.17261083361,-20.5090208918045,-3.69112941580997));
#50182=CARTESIAN_POINT('Ctrl Pts',(375.203613731058,-20.7075370092161,-0.0361104226968403));
#50183=CARTESIAN_POINT('Ctrl Pts',(373.233298575554,-20.9060531266278,3.65197781036011));
#50184=CARTESIAN_POINT('Ctrl Pts',(369.066042509761,-21.1045692440394,3.99565422908433));
#50185=CARTESIAN_POINT('Ctrl Pts',(366.518139363681,-21.3030853614511,0.680186517656126));
#50186=CARTESIAN_POINT('Ctrl Pts',(367.922910383506,-21.5016014788627,-3.25818308354711));
#50187=CARTESIAN_POINT('Ctrl Pts',(371.9938929675,-21.7001175962744,-4.21277056207339));
#50188=CARTESIAN_POINT('Ctrl Pts',(375.002958751962,-21.898633713686,-1.30938296154235));
#50189=CARTESIAN_POINT('Ctrl Pts',(374.1944624296,-22.0971498310977,2.79311278550661));
#50190=CARTESIAN_POINT('Ctrl Pts',(370.30880976131,-22.2956659485093,4.33772868928835));
#50191=CARTESIAN_POINT('Ctrl Pts',(366.904407116324,-22.494182065921,1.90993576249118));
#50192=CARTESIAN_POINT('Ctrl Pts',(367.098942572746,-22.6926981833327,-2.26694122942334));
#50193=CARTESIAN_POINT('Ctrl Pts',(370.714262405752,-22.8912143007443,-4.36779402632158));
#50194=CARTESIAN_POINT('Ctrl Pts',(374.439529327177,-23.089730418156,-2.46870940170645));
#50195=CARTESIAN_POINT('Ctrl Pts',(374.863206782798,-23.2882465355676,1.69118324528528));
#50196=CARTESIAN_POINT('Ctrl Pts',(371.597315540312,-23.4867626529793,4.30229982344905));
#50197=CARTESIAN_POINT('Ctrl Pts',(367.632662422374,-23.6852787703909,2.97349896166417));
#50198=CARTESIAN_POINT('Ctrl Pts',(366.600072351229,-23.8837948878026,-1.07847291799555));
#50199=CARTESIAN_POINT('Ctrl Pts',(369.445024452623,-24.0823110052143,-4.14259823901896));
#50200=CARTESIAN_POINT('Ctrl Pts',(373.562470922641,-24.2808271226259,-3.41342878074717));
#50201=CARTESIAN_POINT('Ctrl Pts',(375.181099920727,-24.4793432400376,0.442560315442714));
#50202=CARTESIAN_POINT('Ctrl Pts',(372.819914294343,-24.6778593574493,3.89146593048189));
#50203=CARTESIAN_POINT('Ctrl Pts',(368.638533463245,-24.876375474861,3.7803898993822));
#50204=CARTESIAN_POINT('Ctrl Pts',(366.471450413703,-25.0749360186145,0.198863423157614));
#50205=CARTESIAN_POINT('Ctrl Pts',(367.687650057685,-25.2073245232308,-2.2967962211639));
#50206=CARTESIAN_POINT('Ctrl Pts',(368.689733840303,-25.2735409887098,-3.01055431632241));
#50207=CARTESIAN_POINT('Ctrl Pts',(369.084296200386,-0.00172336946492562,
3.52553568231652));
#50208=CARTESIAN_POINT('Ctrl Pts',(367.91164328434,-0.0678954086021442,
2.94344882254131));
#50209=CARTESIAN_POINT('Ctrl Pts',(366.213939399476,-0.200239486876582,
0.525043494348995));
#50210=CARTESIAN_POINT('Ctrl Pts',(367.888682353219,-0.398755604288238,
-3.60486726253322));
#50211=CARTESIAN_POINT('Ctrl Pts',(372.266396387737,-0.597271721699893,
-4.42613758256182));
#50212=CARTESIAN_POINT('Ctrl Pts',(375.330090987025,-0.79578783911155,-1.19766966214462));
#50213=CARTESIAN_POINT('Ctrl Pts',(374.277875779333,-0.994303956523205,
3.12933961548655));
#50214=CARTESIAN_POINT('Ctrl Pts',(370.071521003981,-1.19282007393486,4.58972005055539));
#50215=CARTESIAN_POINT('Ctrl Pts',(366.564007968047,-1.39133619134652,1.84732685824735));
#50216=CARTESIAN_POINT('Ctrl Pts',(366.967025111547,-1.58985230875817,-2.58700834044615));
#50217=CARTESIAN_POINT('Ctrl Pts',(370.911702134577,-1.78836842616983,-4.65211635088532));
#50218=CARTESIAN_POINT('Ctrl Pts',(374.785479907238,-1.98688454358148,-2.45695011867353));
#50219=CARTESIAN_POINT('Ctrl Pts',(375.0408741606,-2.18540066099314,1.9882662041693));
#50220=CARTESIAN_POINT('Ctrl Pts',(371.443976673514,-2.3839167784048,4.61265559054459));
#50221=CARTESIAN_POINT('Ctrl Pts',(367.288768849246,-2.58243289581645,3.01286782643016));
#50222=CARTESIAN_POINT('Ctrl Pts',(366.380505616332,-2.78094901322811,-1.34604944103277));
#50223=CARTESIAN_POINT('Ctrl Pts',(369.550959750218,-2.97946513063976,-4.4722790489893));
#50224=CARTESIAN_POINT('Ctrl Pts',(373.896688417238,-3.17798124805142,-3.50288114771708));
#50225=CARTESIAN_POINT('Ctrl Pts',(375.437956569813,-3.37649736546308,0.674388952710513));
#50226=CARTESIAN_POINT('Ctrl Pts',(372.763299861874,-3.57501348287473,4.23406634538199));
#50227=CARTESIAN_POINT('Ctrl Pts',(368.322118169056,-3.77352960028639,3.91626638363723));
#50228=CARTESIAN_POINT('Ctrl Pts',(366.181561137938,-3.97204571769804,0.0120241320746088));
#50229=CARTESIAN_POINT('Ctrl Pts',(368.301910212453,-4.1705618351097,-3.90322957598079));
#50230=CARTESIAN_POINT('Ctrl Pts',(372.741390027776,-4.36907795252135,-4.24397989285769));
#50231=CARTESIAN_POINT('Ctrl Pts',(375.434409424468,-4.56759406993301,-0.698174149437569));
#50232=CARTESIAN_POINT('Ctrl Pts',(373.914752462046,-4.76611018734466,3.48700619768048));
#50233=CARTESIAN_POINT('Ctrl Pts',(369.574092081518,-4.96462630475632,4.47885259966254));
#50234=CARTESIAN_POINT('Ctrl Pts',(366.387522490406,-5.16314242216798,1.36905098729384));
#50235=CARTESIAN_POINT('Ctrl Pts',(367.27324350568,-5.36165853957963,-2.99450147693928));
#50236=CARTESIAN_POINT('Ctrl Pts',(371.420128669554,-5.56017465699129,-4.61574645014013));
#50237=CARTESIAN_POINT('Ctrl Pts',(375.030539431168,-5.75869077440295,-2.00997862506626));
#50238=CARTESIAN_POINT('Ctrl Pts',(374.798130292284,-5.9572068918146,2.4364893909746));
#50239=CARTESIAN_POINT('Ctrl Pts',(370.935737121425,-6.15572300922625,4.65166676971372));
#50240=CARTESIAN_POINT('Ctrl Pts',(366.980466113943,-6.35423912663792,2.60693620482841));
#50241=CARTESIAN_POINT('Ctrl Pts',(366.554479221263,-6.55275524404956,-1.82517694725159));
#50242=CARTESIAN_POINT('Ctrl Pts',(370.04788713657,-6.75127136146123,-4.58582776958665));
#50243=CARTESIAN_POINT('Ctrl Pts',(374.261493342691,-6.94978747887288,-3.14686475222743));
#50244=CARTESIAN_POINT('Ctrl Pts',(375.336557427349,-7.14830359628454,1.17393714550662));
#50245=CARTESIAN_POINT('Ctrl Pts',(372.288556151701,-7.34681971369619,4.41966973603814));
#50246=CARTESIAN_POINT('Ctrl Pts',(367.908791104855,-7.54533583110785,3.61795285333871));
#50247=CARTESIAN_POINT('Ctrl Pts',(366.208167804746,-7.7438519485195,-0.497016431687658));
#50248=CARTESIAN_POINT('Ctrl Pts',(368.744084720329,-7.94236806593115,-4.15682752282947));
#50249=CARTESIAN_POINT('Ctrl Pts',(373.194197378567,-8.14088418334282,-4.00989503980782));
#50250=CARTESIAN_POINT('Ctrl Pts',(375.483177257165,-8.33940030075446,-0.19077695562173));
#50251=CARTESIAN_POINT('Ctrl Pts',(373.514820124317,-8.53791641816613,3.80305103556024));
#50252=CARTESIAN_POINT('Ctrl Pts',(369.091710000162,-8.73643253557777,4.31411723007756));
#50253=CARTESIAN_POINT('Ctrl Pts',(366.264446999925,-8.93494865298944,0.874396928501112));
#50254=CARTESIAN_POINT('Ctrl Pts',(367.622184798979,-9.13346477040109,-3.36607944740345));
#50255=CARTESIAN_POINT('Ctrl Pts',(371.921532947862,-9.33198088781275,-4.52396429499635));
#50256=CARTESIAN_POINT('Ctrl Pts',(375.225230194099,-9.5304970052244,-1.53888869615729));
#50257=CARTESIAN_POINT('Ctrl Pts',(374.507813442573,-9.72901312263606,2.85547189785572));
#50258=CARTESIAN_POINT('Ctrl Pts',(370.426279307617,-9.92752924004772,4.63484564464738));
#50259=CARTESIAN_POINT('Ctrl Pts',(366.718419111011,-10.1260453574593,2.1697159141836));
#50260=CARTESIAN_POINT('Ctrl Pts',(366.779820689829,-10.324561474871,-2.28239837811655));
#50261=CARTESIAN_POINT('Ctrl Pts',(370.55425364617,-10.5230775922827,-4.6443356515583));
#50262=CARTESIAN_POINT('Ctrl Pts',(374.585164075945,-10.7215937096943,-2.75307867993461));
#50263=CARTESIAN_POINT('Ctrl Pts',(375.181120883613,-10.920109827106,1.65939537766375));
#50264=CARTESIAN_POINT('Ctrl Pts',(371.796358161012,-11.1186259445176,4.55222671344473));
#50265=CARTESIAN_POINT('Ctrl Pts',(367.530577224486,-11.3171420619293,3.2762154175869));
#50266=CARTESIAN_POINT('Ctrl Pts',(366.290299111949,-11.5156581793409,-1.00009163747166));
#50267=CARTESIAN_POINT('Ctrl Pts',(369.211346926269,-11.7141742967526,-4.3605337946938));
#50268=CARTESIAN_POINT('Ctrl Pts',(373.618680643315,-11.9126904141642,-3.72768204888329));
#50269=CARTESIAN_POINT('Ctrl Pts',(375.476147881392,-12.1112065315759,0.31891000926328));
#50270=CARTESIAN_POINT('Ctrl Pts',(373.082715476643,-12.3097226489876,4.07345034723814));
#50271=CARTESIAN_POINT('Ctrl Pts',(368.630243297424,-12.5082387663992,4.09760234245405));
#50272=CARTESIAN_POINT('Ctrl Pts',(366.196220670465,-12.7067548838109,0.3692480571119));
#50273=CARTESIAN_POINT('Ctrl Pts',(368.009679217512,-12.9052710012225,-3.69725657509051));
#50274=CARTESIAN_POINT('Ctrl Pts',(372.409888096822,-13.1037871186342,-4.3778839651024));
#50275=CARTESIAN_POINT('Ctrl Pts',(375.367219717569,-13.3023032360458,-1.04932849605667));
#50276=CARTESIAN_POINT('Ctrl Pts',(374.173406035886,-13.5008193534575,3.24018204933326));
#50277=CARTESIAN_POINT('Ctrl Pts',(369.921718912714,-13.6993354708691,4.56239550874181));
#50278=CARTESIAN_POINT('Ctrl Pts',(366.505772539789,-13.8978515882808,1.70645394720947));
#50279=CARTESIAN_POINT('Ctrl Pts',(367.053825627246,-14.0963677056925,-2.71222567898131));
#50280=CARTESIAN_POINT('Ctrl Pts',(371.063981582666,-14.2948838231041,-4.64710062036397));
#50281=CARTESIAN_POINT('Ctrl Pts',(374.863815863332,-14.4933999405158,-2.32624921084424));
#50282=CARTESIAN_POINT('Ctrl Pts',(374.97351251552,-14.6919160579274,2.12493697601463));
#50283=CARTESIAN_POINT('Ctrl Pts',(371.29261343181,-14.8904321753391,4.63014630082654));
#50284=CARTESIAN_POINT('Ctrl Pts',(367.192015974937,-15.0889482927507,2.89515571806315));
#50285=CARTESIAN_POINT('Ctrl Pts',(366.426969294272,-15.2874644101624,-1.49116339960125));
#50286=CARTESIAN_POINT('Ctrl Pts',(369.698088587236,-15.485980527574,-4.51190344084632));
#50287=CARTESIAN_POINT('Ctrl Pts',(374.00974502862,-15.6844966449857,-3.40072813646827));
#50288=CARTESIAN_POINT('Ctrl Pts',(375.413405665806,-15.8830127623974,0.824769306579049));
#50289=CARTESIAN_POINT('Ctrl Pts',(372.623624787716,-16.081528879809,4.29495870743703));
#50290=CARTESIAN_POINT('Ctrl Pts',(368.195230655245,-16.2800449972207,3.83190662280167));
#50291=CARTESIAN_POINT('Ctrl Pts',(366.183662377922,-16.4785611146323,-0.140332656402569));
#50292=CARTESIAN_POINT('Ctrl Pts',(368.431075920034,-16.677077232044,-3.98405795828352));
#50293=CARTESIAN_POINT('Ctrl Pts',(372.879332710052,-16.8755933494556,-4.17925876678659));
#50294=CARTESIAN_POINT('Ctrl Pts',(375.454803794495,-17.0741094668673,-0.547173894597784));
#50295=CARTESIAN_POINT('Ctrl Pts',(373.798921744885,-17.272625584279,3.58600242191256));
#50296=CARTESIAN_POINT('Ctrl Pts',(369.428111844037,-17.4711417016906,4.43518593343438));
#50297=CARTESIAN_POINT('Ctrl Pts',(366.345078657529,-17.6696578191023,1.22271053329916));
#50298=CARTESIAN_POINT('Ctrl Pts',(367.373205332054,-17.8681739365139,-3.10949991481088));
#50299=CARTESIAN_POINT('Ctrl Pts',(371.570953016126,-18.0666900539256,-4.59408948989735));
#50300=CARTESIAN_POINT('Ctrl Pts',(375.094104230299,-18.2652061713372,-1.87149929898408));
#50301=CARTESIAN_POINT('Ctrl Pts',(374.716224110076,-18.4637222887489,2.56497435024718));
#50302=CARTESIAN_POINT('Ctrl Pts',(370.783368081515,-18.6622384061605,4.65249328050807));
#50303=CARTESIAN_POINT('Ctrl Pts',(366.897170884718,-18.8607545235722,2.47934736428527));
#50304=CARTESIAN_POINT('Ctrl Pts',(366.616537989202,-19.0592706409838,-1.96433770596103));
#50305=CARTESIAN_POINT('Ctrl Pts',(370.198467662479,-19.2577867583955,-4.60911967075604));
#50306=CARTESIAN_POINT('Ctrl Pts',(374.362696845284,-19.4563028758072,-3.03295751581995));
#50307=CARTESIAN_POINT('Ctrl Pts',(375.295703664052,-19.6548189932188,1.32072943912346));
#50308=CARTESIAN_POINT('Ctrl Pts',(372.143058221809,-19.8533351106305,4.46491749667864));
#50309=CARTESIAN_POINT('Ctrl Pts',(367.791893244921,-20.0518512280421,3.5202190424639));
#50310=CARTESIAN_POINT('Ctrl Pts',(366.226922851216,-20.2503673454538,-0.648229049073077));
#50311=CARTESIAN_POINT('Ctrl Pts',(368.881317158506,-20.4488834628655,-4.22304130829977));
#50312=CARTESIAN_POINT('Ctrl Pts',(373.324232351795,-20.6473995802771,-3.93047266772016));
#50313=CARTESIAN_POINT('Ctrl Pts',(375.486931210927,-20.8459156976888,-0.0384519244494463));
#50314=CARTESIAN_POINT('Ctrl Pts',(373.388855258257,-21.0444318151004,3.88878236164229));
#50315=CARTESIAN_POINT('Ctrl Pts',(368.951382544395,-21.2429479325121,4.25474372960455));
#50316=CARTESIAN_POINT('Ctrl Pts',(366.238266165228,-21.4414640499237,0.724291731725312));
#50317=CARTESIAN_POINT('Ctrl Pts',(367.734126503847,-21.6399801673354,-3.46945287300359));
#50318=CARTESIAN_POINT('Ctrl Pts',(372.069083091557,-21.838496284747,-4.48593849857525));
#50319=CARTESIAN_POINT('Ctrl Pts',(375.273265196508,-22.0370124021587,-1.39428704934514));
#50320=CARTESIAN_POINT('Ctrl Pts',(374.412343690105,-22.2355285195704,2.97422610387783));
#50321=CARTESIAN_POINT('Ctrl Pts',(370.274734333046,-22.434044636982,4.61899926353358));
#50322=CARTESIAN_POINT('Ctrl Pts',(366.649580609441,-22.6325607543937,2.0337813893544));
#50323=CARTESIAN_POINT('Ctrl Pts',(366.856730294058,-22.8310768718053,-2.41393609864016));
#50324=CARTESIAN_POINT('Ctrl Pts',(370.706477671604,-23.029592989217,-4.65101412189882));
#50325=CARTESIAN_POINT('Ctrl Pts',(374.673301417178,-23.2281091066286,-2.62878748883471));
#50326=CARTESIAN_POINT('Ctrl Pts',(375.124451315125,-23.4266252240403,1.80084434136301));
#50327=CARTESIAN_POINT('Ctrl Pts',(371.646790464395,-23.6251413414519,4.58127309001248));
#50328=CARTESIAN_POINT('Ctrl Pts',(367.425058045505,-23.8236574588636,3.1663090289536));
#50329=CARTESIAN_POINT('Ctrl Pts',(366.325511918996,-24.0221735762753,-1.14840414668247));
#50330=CARTESIAN_POINT('Ctrl Pts',(369.354938746353,-24.2206896936869,-4.41121600398739));
#50331=CARTESIAN_POINT('Ctrl Pts',(373.73937206963,-24.4192058110986,-3.63476513949107));
#50332=CARTESIAN_POINT('Ctrl Pts',(375.462957541574,-24.6177219285102,0.471257175707393));
#50333=CARTESIAN_POINT('Ctrl Pts',(372.948665973209,-24.8162380459219,4.14379956758217));
#50334=CARTESIAN_POINT('Ctrl Pts',(368.496152604384,-25.0147541633335,4.02552105304239));
#50335=CARTESIAN_POINT('Ctrl Pts',(366.188549771923,-25.2133147070871,0.211758288935219));
#50336=CARTESIAN_POINT('Ctrl Pts',(367.483611234327,-25.3457032117033,-2.44572697233012));
#50337=CARTESIAN_POINT('Ctrl Pts',(368.550672958437,-25.4119196771824,-3.20576715742043));
#50338=CARTESIAN_POINT('Ctrl Pts',(369.081337125798,-25.,3.52813093583777));
#50339=CARTESIAN_POINT('Ctrl Pts',(369.008004389183,-25.0000000000002,3.48377167173236));
#50340=CARTESIAN_POINT('Ctrl Pts',(368.936373634155,-25.0000000000002,3.43693146060399));
#50341=CARTESIAN_POINT('Ctrl Pts',(368.866583043242,-25.0000000000002,3.38761093025279));
#50342=CARTESIAN_POINT('Ctrl Pts',(368.768579307259,-25.0000000000002,3.31835236442314));
#50343=CARTESIAN_POINT('Ctrl Pts',(368.674202465802,-25.,3.24420420960068));
#50344=CARTESIAN_POINT('Ctrl Pts',(368.583606663623,-25.0000000000001,3.1655786709461));
#50345=CARTESIAN_POINT('Ctrl Pts',(368.490441324965,-25.0000000000001,3.08472310413516));
#50346=CARTESIAN_POINT('Ctrl Pts',(368.401273978833,-25.0000000000001,2.9991317898415));
#50347=CARTESIAN_POINT('Ctrl Pts',(368.316316523814,-25.,2.9092182158941));
#50348=CARTESIAN_POINT('Ctrl Pts',(368.231359068795,-25.,2.8193046419467));
#50349=CARTESIAN_POINT('Ctrl Pts',(368.150611123225,-24.9999999999999,2.72506785206802));
#50350=CARTESIAN_POINT('Ctrl Pts',(368.074335136508,-24.9999999999999,2.62690044695477));
#50351=CARTESIAN_POINT('Ctrl Pts',(368.051804137619,-24.9999999999999,2.59790298929197));
#50352=CARTESIAN_POINT('Ctrl Pts',(368.029663691347,-25.0000000000001,2.56856248344712));
#50353=CARTESIAN_POINT('Ctrl Pts',(368.007921481441,-25.0000000000001,2.5388888873865));
#50354=CARTESIAN_POINT('Ctrl Pts',(367.995462146392,-25.0000000000001,2.52188448548694));
#50355=CARTESIAN_POINT('Ctrl Pts',(367.983131721802,-25.0000000000001,2.50476791384));
#50356=CARTESIAN_POINT('Ctrl Pts',(367.970946292708,-25.0000000000001,2.48756205372084));
#50357=CARTESIAN_POINT('Ctrl Pts',(367.901749679588,-24.9999999999999,2.38985624156957));
#50358=CARTESIAN_POINT('Ctrl Pts',(367.837127619974,-25.0000000000001,2.28914348626008));
#50359=CARTESIAN_POINT('Ctrl Pts',(367.777242914735,-25.,2.18581597331342));
#50360=CARTESIAN_POINT('Ctrl Pts',(367.71761918203,-24.9999999999999,2.08293875302096));
#50361=CARTESIAN_POINT('Ctrl Pts',(367.66269132976,-25.,1.97746862871235));
#50362=CARTESIAN_POINT('Ctrl Pts',(367.612667283613,-25.,1.86977335561688));
#50363=CARTESIAN_POINT('Ctrl Pts',(367.563024060491,-25.,1.76289794502663));
#50364=CARTESIAN_POINT('Ctrl Pts',(367.518210030985,-25.,1.65383030873021));
#50365=CARTESIAN_POINT('Ctrl Pts',(367.478478768323,-24.9999999999999,1.54292354068813));
#50366=CARTESIAN_POINT('Ctrl Pts',(367.458684313889,-24.9999999999999,1.48766884150577));
#50367=CARTESIAN_POINT('Ctrl Pts',(367.440152269773,-25.,1.43195762663986));
#50368=CARTESIAN_POINT('Ctrl Pts',(367.42291898926,-25.0000000000001,1.3758339276038));
#50369=CARTESIAN_POINT('Ctrl Pts',(367.413229129654,-25.0000000000001,1.34427691999609));
#50370=CARTESIAN_POINT('Ctrl Pts',(367.403949941077,-25.0000000000001,1.31258951221787));
#50371=CARTESIAN_POINT('Ctrl Pts',(367.395088369449,-25.0000000000001,1.28077962509273));
#50372=CARTESIAN_POINT('Ctrl Pts',(367.389241343217,-25.0000000000001,1.25979088265963));
#50373=CARTESIAN_POINT('Ctrl Pts',(367.383576137904,-25.,1.23874881912547));
#50374=CARTESIAN_POINT('Ctrl Pts',(367.378094833834,-25.,1.2176557314011));
#50375=CARTESIAN_POINT('Ctrl Pts',(367.374400750062,-24.9999999999999,1.2034402031139));
#50376=CARTESIAN_POINT('Ctrl Pts',(367.37079089563,-24.9999999999998,1.18920406156008));
#50377=CARTESIAN_POINT('Ctrl Pts',(367.367267768483,-24.9999999999998,1.17495628199712));
#50378=CARTESIAN_POINT('Ctrl Pts',(367.339710086504,-24.9999999999998,1.06351103413865));
#50379=CARTESIAN_POINT('Ctrl Pts',(367.31741606077,-24.9999999999999,0.951207563746677));
#50380=CARTESIAN_POINT('Ctrl Pts',(367.300575616194,-24.9999999999999,0.838383113658457));
#50381=CARTESIAN_POINT('Ctrl Pts',(367.283952711426,-25.,0.727016095948555));
#50382=CARTESIAN_POINT('Ctrl Pts',(367.272643274885,-24.9999999999997,0.615140724577881));
#50383=CARTESIAN_POINT('Ctrl Pts',(367.26688064429,-24.9999999999999,0.503082333892389));
#50384=CARTESIAN_POINT('Ctrl Pts',(367.261118013696,-25.0000000000001,0.391023943206896));
#50385=CARTESIAN_POINT('Ctrl Pts',(367.260901956193,-25.,0.278781817875379));
#50386=CARTESIAN_POINT('Ctrl Pts',(367.266519668115,-24.9999999999999,0.16669318468162));
#50387=CARTESIAN_POINT('Ctrl Pts',(367.270046945812,-24.9999999999999,0.0963144003213416));
#50388=CARTESIAN_POINT('Ctrl Pts',(367.275875445267,-24.9999999999998,0.0259964001582221));
#50389=CARTESIAN_POINT('Ctrl Pts',(367.283964401729,-25.,-0.0441711994751926));
#50390=CARTESIAN_POINT('Ctrl Pts',(367.286810051659,-25.,-0.0688557710840931));
#50391=CARTESIAN_POINT('Ctrl Pts',(367.289935509814,-25.0000000000001,-0.0935216922831735));
#50392=CARTESIAN_POINT('Ctrl Pts',(367.293339176269,-25.0000000000001,-0.118164932406376));
#50393=CARTESIAN_POINT('Ctrl Pts',(367.295707273414,-25.0000000000002,-0.13531043927267));
#50394=CARTESIAN_POINT('Ctrl Pts',(367.298210043733,-24.9999999999999,-0.152444965532065));
#50395=CARTESIAN_POINT('Ctrl Pts',(367.300846972729,-24.9999999999998,-0.169567132184699));
#50396=CARTESIAN_POINT('Ctrl Pts',(367.303272993684,-24.9999999999998,-0.185319825996345));
#50397=CARTESIAN_POINT('Ctrl Pts',(367.305810982859,-24.9999999999999,-0.201051738242575));
#50398=CARTESIAN_POINT('Ctrl Pts',(367.308460062164,-25.,-0.216761568244168));
#50399=CARTESIAN_POINT('Ctrl Pts',(367.326841341943,-25.0000000000001,-0.325768037013256));
#50400=CARTESIAN_POINT('Ctrl Pts',(367.350567912994,-24.9999999999998,-0.433718326729101));
#50401=CARTESIAN_POINT('Ctrl Pts',(367.379395445099,-24.9999999999998,-0.54029437093727));
#50402=CARTESIAN_POINT('Ctrl Pts',(367.408704572919,-24.9999999999999,-0.648650885498511));
#50403=CARTESIAN_POINT('Ctrl Pts',(367.443286972773,-25.0000000000001,-0.755587671881746));
#50404=CARTESIAN_POINT('Ctrl Pts',(367.482934839879,-25.0000000000001,-0.86074938973287));
#50405=CARTESIAN_POINT('Ctrl Pts',(367.52224800911,-25.,-0.965023357345557));
#50406=CARTESIAN_POINT('Ctrl Pts',(367.566542101419,-25.0000000000002,-1.06755279241357));
#50407=CARTESIAN_POINT('Ctrl Pts',(367.615653947938,-25.0000000000001,-1.16795954601739));
#50408=CARTESIAN_POINT('Ctrl Pts',(367.652491193367,-25.,-1.24327148167718));
#50409=CARTESIAN_POINT('Ctrl Pts',(367.692039773092,-25.,-1.31738860793362));
#50410=CARTESIAN_POINT('Ctrl Pts',(367.734242507007,-25.,-1.39013596224847));
#50411=CARTESIAN_POINT('Ctrl Pts',(367.747211950558,-25.,-1.41249216095307));
#50412=CARTESIAN_POINT('Ctrl Pts',(367.760435499407,-25.0000000000001,-1.4347242132668));
#50413=CARTESIAN_POINT('Ctrl Pts',(367.773893192447,-25.0000000000001,-1.45679714311184));
#50414=CARTESIAN_POINT('Ctrl Pts',(367.831176407707,-25.0000000000002,-1.55075146261937));
#50415=CARTESIAN_POINT('Ctrl Pts',(367.892745302596,-25.,-1.64191051491612));
#50416=CARTESIAN_POINT('Ctrl Pts',(367.95841903902,-25.,-1.72992127878184));
#50417=CARTESIAN_POINT('Ctrl Pts',(368.026003592275,-25.0000000000001,-1.82049276871758));
#50418=CARTESIAN_POINT('Ctrl Pts',(368.097935785625,-25.0000000000002,-1.90773109063843));
#50419=CARTESIAN_POINT('Ctrl Pts',(368.174053320765,-25.0000000000001,-1.99120413362777));
#50420=CARTESIAN_POINT('Ctrl Pts',(368.208432762019,-25.0000000000001,-2.02890578243333));
#50421=CARTESIAN_POINT('Ctrl Pts',(368.243666428395,-25.,-2.06583859593258));
#50422=CARTESIAN_POINT('Ctrl Pts',(368.279741192986,-25.0000000000001,-2.10195888917106));
#50423=CARTESIAN_POINT('Ctrl Pts',(368.291644378927,-25.0000000000002,-2.1138770976905));
#50424=CARTESIAN_POINT('Ctrl Pts',(368.303638458318,-25.,-2.12570606365943));
#50425=CARTESIAN_POINT('Ctrl Pts',(368.315715640136,-25.,-2.13743730062655));
#50426=CARTESIAN_POINT('Ctrl Pts',(368.391540722707,-25.0000000000001,-2.21109041151526));
#50427=CARTESIAN_POINT('Ctrl Pts',(368.470715155507,-25.0000000000001,-2.28097119290546));
#50428=CARTESIAN_POINT('Ctrl Pts',(368.553093431011,-25.0000000000001,-2.34673408051994));
#50429=CARTESIAN_POINT('Ctrl Pts',(368.633211360681,-25.0000000000001,-2.41069252554136));
#50430=CARTESIAN_POINT('Ctrl Pts',(368.716360276367,-25.0000000000001,-2.47075627465853));
#50431=CARTESIAN_POINT('Ctrl Pts',(368.802425787939,-25.0000000000002,-2.52656271084893));
#50432=CARTESIAN_POINT('Ctrl Pts',(368.854788791589,-25.0000000000002,-2.56051583061294));
#50433=CARTESIAN_POINT('Ctrl Pts',(368.908231748608,-25.0000000000002,-2.59289216715227));
#50434=CARTESIAN_POINT('Ctrl Pts',(368.962731321485,-25.,-2.62360084935009));
#50435=CARTESIAN_POINT('Ctrl Pts',(368.958580243284,-1.20159524691354E-13,
-2.62730819722368));
#50436=CARTESIAN_POINT('Ctrl Pts',(368.896667223351,-3.12253651536795E-14,
-2.59284588111042));
#50437=CARTESIAN_POINT('Ctrl Pts',(368.836104112209,-1.8704388297858E-13,
-2.55627615699171));
#50438=CARTESIAN_POINT('Ctrl Pts',(368.777011016265,-1.30943866860633E-13,
-2.51762860130017));
#50439=CARTESIAN_POINT('Ctrl Pts',(368.691754001996,-4.95917179562384E-14,
-2.4618695459587));
#50440=CARTESIAN_POINT('Ctrl Pts',(368.609555629646,-1.32137019917602E-13,
-2.4017880170848));
#50441=CARTESIAN_POINT('Ctrl Pts',(368.530495563443,-1.30916111285018E-13,
-2.33778526550872));
#50442=CARTESIAN_POINT('Ctrl Pts',(368.449492513799,-1.29393310518178E-13,
-2.27220957967648));
#50443=CARTESIAN_POINT('Ctrl Pts',(368.371783421322,4.86435335969926E-14,
-2.2025171945328));
#50444=CARTESIAN_POINT('Ctrl Pts',(368.297473473753,3.3660574327854E-14,
-2.12908838121556));
#50445=CARTESIAN_POINT('Ctrl Pts',(368.221729114233,1.83158428439202E-14,
-2.05424216456431));
#50446=CARTESIAN_POINT('Ctrl Pts',(368.149515825788,-8.1812323111681E-14,
-1.97551336828871));
#50447=CARTESIAN_POINT('Ctrl Pts',(368.080973191528,-1.82603931975223E-13,
-1.89325888662171));
#50448=CARTESIAN_POINT('Ctrl Pts',(368.059248050056,-2.14700691140463E-13,
-1.86718766437808));
#50449=CARTESIAN_POINT('Ctrl Pts',(368.03789191569,-1.53909802920789E-13,
-1.84076193575357));
#50450=CARTESIAN_POINT('Ctrl Pts',(368.016909953942,-4.20774526332934E-14,
-1.81399226410803));
#50451=CARTESIAN_POINT('Ctrl Pts',(368.00698466764,1.09792968138055E-14,
-1.80132916527718));
#50452=CARTESIAN_POINT('Ctrl Pts',(367.99714281104,-1.84639436501056E-13,
-1.78858859232451));
#50453=CARTESIAN_POINT('Ctrl Pts',(367.987394394324,-1.58761892521397E-13,
-1.77578435380463));
#50454=CARTESIAN_POINT('Ctrl Pts',(367.92073258765,1.96712162946812E-14,
-1.68822616895041));
#50455=CARTESIAN_POINT('Ctrl Pts',(367.858328742098,-7.66173391862864E-14,
-1.59755706304694));
#50456=CARTESIAN_POINT('Ctrl Pts',(367.800281843188,-3.99680288865056E-15,
-1.50421981105859));
#50457=CARTESIAN_POINT('Ctrl Pts',(367.742234944279,6.86237334089853E-14,
-1.41088255907024));
#50458=CARTESIAN_POINT('Ctrl Pts',(367.688544517787,-2.3646706107268E-13,
-1.31487644576671));
#50459=CARTESIAN_POINT('Ctrl Pts',(367.639337755227,-2.30065966277948E-13,
-1.21659878608418));
#50460=CARTESIAN_POINT('Ctrl Pts',(367.589288906219,-2.24035458786638E-13,
-1.11663927860252));
#50461=CARTESIAN_POINT('Ctrl Pts',(367.543877872957,2.29330542649884E-14,
-1.01432914427311));
#50462=CARTESIAN_POINT('Ctrl Pts',(367.503276095346,1.75970349403087E-14,
-0.910049731540007));
#50463=CARTESIAN_POINT('Ctrl Pts',(367.48289670826,1.4660611493931E-14,
-0.857708414427849));
#50464=CARTESIAN_POINT('Ctrl Pts',(367.463729595381,-1.75345152813706E-13,
-0.804870454339346));
#50465=CARTESIAN_POINT('Ctrl Pts',(367.445800684405,-2.20712337295481E-13,
-0.751581520596565));
#50466=CARTESIAN_POINT('Ctrl Pts',(367.432652660306,-2.54138506807475E-13,
-0.712502505366526));
#50467=CARTESIAN_POINT('Ctrl Pts',(367.420170588684,-1.50535198818543E-13,
-0.673180926026252));
#50468=CARTESIAN_POINT('Ctrl Pts',(367.408365775792,-2.26846319506535E-13,
-0.633634372562032));
#50469=CARTESIAN_POINT('Ctrl Pts',(367.403898301248,-2.55619978963674E-13,
-0.61866817000582));
#50470=CARTESIAN_POINT('Ctrl Pts',(367.399528497761,-1.58501758860923E-13,
-0.603671792966296));
#50471=CARTESIAN_POINT('Ctrl Pts',(367.395259906534,-1.5512591211575E-13,
-0.588657214169824));
#50472=CARTESIAN_POINT('Ctrl Pts',(367.363762596442,-1.31200303611061E-13,
-0.477866834126048));
#50473=CARTESIAN_POINT('Ctrl Pts',(367.337723096572,8.68805780094438E-14,
-0.365923016810904));
#50474=CARTESIAN_POINT('Ctrl Pts',(367.317274728141,1.70696790036118E-14,
-0.253257167461436));
#50475=CARTESIAN_POINT('Ctrl Pts',(367.296972417425,-5.22425777530995E-14,
-0.14139606283405));
#50476=CARTESIAN_POINT('Ctrl Pts',(367.282181192585,1.1519324841062E-13,
-0.0288223438826056));
#50477=CARTESIAN_POINT('Ctrl Pts',(367.273072973574,4.86000129029662E-14,
0.084071210533729));
#50478=CARTESIAN_POINT('Ctrl Pts',(367.264525485063,-1.45421330099294E-14,
0.190014684024364));
#50479=CARTESIAN_POINT('Ctrl Pts',(367.260982825867,-1.85488797503548E-13,
0.296240640277909));
#50480=CARTESIAN_POINT('Ctrl Pts',(367.262626175817,-1.2356782264078E-13,
0.402438260595486));
#50481=CARTESIAN_POINT('Ctrl Pts',(367.263830822359,-7.84670444554026E-14,
0.480285706399798));
#50482=CARTESIAN_POINT('Ctrl Pts',(367.267822987318,4.24060545398861E-14,
0.558118233893516));
#50483=CARTESIAN_POINT('Ctrl Pts',(367.2745278326,7.17481629664007E-14,
0.635838377479383));
#50484=CARTESIAN_POINT('Ctrl Pts',(367.276457612589,8.02928709341649E-14,
0.65820768974695));
#50485=CARTESIAN_POINT('Ctrl Pts',(367.278612189094,7.0348597872745E-14,
0.680567693369209));
#50486=CARTESIAN_POINT('Ctrl Pts',(367.280989967383,1.7125190154843E-14,
0.702916061212433));
#50487=CARTESIAN_POINT('Ctrl Pts',(367.283332529267,-3.46588239178081E-14,
0.724933435554674));
#50488=CARTESIAN_POINT('Ctrl Pts',(367.285892448296,1.2455954399965E-13,
0.746944401464202));
#50489=CARTESIAN_POINT('Ctrl Pts',(367.288664178637,1.33587585438022E-13,
0.768916642339298));
#50490=CARTESIAN_POINT('Ctrl Pts',(367.302614038008,1.78981378037621E-13,
0.879500874045485));
#50491=CARTESIAN_POINT('Ctrl Pts',(367.321936335458,-1.24773023519911E-13,
0.989232886547642));
#50492=CARTESIAN_POINT('Ctrl Pts',(367.346325288731,-1.12854170453147E-13,
1.09782477106727));
#50493=CARTESIAN_POINT('Ctrl Pts',(367.371307395697,-1.0074091404704E-13,
1.20905767410888));
#50494=CARTESIAN_POINT('Ctrl Pts',(367.401605669227,-4.08269138960946E-14,
1.319094933492));
#50495=CARTESIAN_POINT('Ctrl Pts',(367.436945218641,-1.39610545346613E-13,
1.42763593264953));
#50496=CARTESIAN_POINT('Ctrl Pts',(367.473165204033,-2.40870682695136E-13,
1.53888108062296));
#50497=CARTESIAN_POINT('Ctrl Pts',(367.514680880354,1.44458975729594E-13,
1.64855523782715));
#50498=CARTESIAN_POINT('Ctrl Pts',(367.561250870734,1.25677246387568E-13,
1.75633336602783));
#50499=CARTESIAN_POINT('Ctrl Pts',(367.600265921544,1.10273611345618E-13,
1.84662690299669));
#50500=CARTESIAN_POINT('Ctrl Pts',(367.642829467058,-3.26636295549089E-14,
1.9355899035714));
#50501=CARTESIAN_POINT('Ctrl Pts',(367.688826929101,-1.28674848554056E-13,
2.02302448049586));
#50502=CARTESIAN_POINT('Ctrl Pts',(367.69883194909,-1.49484545206251E-13,
2.04204258825589));
#50503=CARTESIAN_POINT('Ctrl Pts',(367.7089995222,-1.28827627965532E-13,
2.06098834877383));
#50504=CARTESIAN_POINT('Ctrl Pts',(367.719328615054,-1.27398092075737E-13,
2.07985966126142));
#50505=CARTESIAN_POINT('Ctrl Pts',(367.728509214281,-1.26400725739923E-13,
2.09663266923727));
#50506=CARTESIAN_POINT('Ctrl Pts',(367.737813168611,-1.28517961198261E-14,
2.11333905951663));
#50507=CARTESIAN_POINT('Ctrl Pts',(367.747236849987,-3.51940698806175E-14,
2.12997310026321));
#50508=CARTESIAN_POINT('Ctrl Pts',(367.806624057047,-1.74409790917852E-13,
2.23479935473743));
#50509=CARTESIAN_POINT('Ctrl Pts',(367.870792434446,-7.64407390032732E-14,
2.33680885037705));
#50510=CARTESIAN_POINT('Ctrl Pts',(367.939467138126,-2.88657986402541E-15,
2.43566584941741));
#50511=CARTESIAN_POINT('Ctrl Pts',(368.008598405184,7.14984065523101E-14,
2.53518006986634));
#50512=CARTESIAN_POINT('Ctrl Pts',(368.082296431862,-3.67899973920985E-14,
2.63150057287638));
#50513=CARTESIAN_POINT('Ctrl Pts',(368.16033137017,-1.60982338570648E-14,
2.72427050132567));
#50514=CARTESIAN_POINT('Ctrl Pts',(368.195472296089,-6.73981254935445E-15,
2.76604693190711));
#50515=CARTESIAN_POINT('Ctrl Pts',(368.231493356358,9.84733976286278E-14,
2.80710306904633));
#50516=CARTESIAN_POINT('Ctrl Pts',(368.268376606191,2.91988655476416E-14,
2.8474046769452));
#50517=CARTESIAN_POINT('Ctrl Pts',(368.289617840286,-1.05235299652341E-14,
2.87061455925349));
#50518=CARTESIAN_POINT('Ctrl Pts',(368.311150090951,-4.03533354721523E-15,
2.89357920292765));
#50519=CARTESIAN_POINT('Ctrl Pts',(368.332943578336,2.33146835171283E-14,
2.91626474739458));
#50520=CARTESIAN_POINT('Ctrl Pts',(368.418412002948,1.30553930674682E-13,
3.00523158931483));
#50521=CARTESIAN_POINT('Ctrl Pts',(368.507948563201,8.15823027870669E-15,
3.08997044913753));
#50522=CARTESIAN_POINT('Ctrl Pts',(368.601298624144,-1.07136521876328E-14,
3.17012489733602));
#50523=CARTESIAN_POINT('Ctrl Pts',(368.693422616792,-2.88627181492191E-14,
3.24922658963247));
#50524=CARTESIAN_POINT('Ctrl Pts',(368.789261074837,1.23156603782099E-13,
3.32386425813697));
#50525=CARTESIAN_POINT('Ctrl Pts',(368.888611897156,1.69086966650411E-13,
3.3936691068897));
#50526=CARTESIAN_POINT('Ctrl Pts',(368.95282952375,1.98583755561227E-13,
3.43878903249292));
#50527=CARTESIAN_POINT('Ctrl Pts',(369.018515449972,6.92162971711572E-14,
3.4818892617252));
#50528=CARTESIAN_POINT('Ctrl Pts',(369.085623377893,3.05311331771918E-15,
3.52286199445089));
#50529=CARTESIAN_POINT('Ctrl Pts',(373.11810396585,0.412130952468996,-3.20610701674044));
#50530=CARTESIAN_POINT('Ctrl Pts',(374.185302789364,0.34591310276681,-2.44600546672676));
#50531=CARTESIAN_POINT('Ctrl Pts',(375.480525080075,0.213523213927405,0.211751707408718));
#50532=CARTESIAN_POINT('Ctrl Pts',(373.172696361849,0.0149612859507822,
4.02588784127813));
#50533=CARTESIAN_POINT('Ctrl Pts',(368.719776930065,-0.183554831460874,
4.14417747187957));
#50534=CARTESIAN_POINT('Ctrl Pts',(366.205256212803,-0.382070948872529,
0.471300063467854));
#50535=CARTESIAN_POINT('Ctrl Pts',(367.928998792514,-0.580587066284185,
-3.63509646070476));
#50536=CARTESIAN_POINT('Ctrl Pts',(372.313831828821,-0.779103183695841,
-4.4116181741134));
#50537=CARTESIAN_POINT('Ctrl Pts',(375.343534831733,-0.977619301107497,
-1.14850882859149));
#50538=CARTESIAN_POINT('Ctrl Pts',(374.24388846515,-1.17613541851915,3.16659767841453));
#50539=CARTESIAN_POINT('Ctrl Pts',(370.021771173424,-1.37465153593081,4.58169074422432));
#50540=CARTESIAN_POINT('Ctrl Pts',(366.543793281998,-1.57316765334246,1.80100851318485));
#50541=CARTESIAN_POINT('Ctrl Pts',(366.994984309258,-1.77168377075412,-2.62902714077588));
#50542=CARTESIAN_POINT('Ctrl Pts',(370.96216968929,-1.97019988816577,-4.65143813111721));
#50543=CARTESIAN_POINT('Ctrl Pts',(374.812268028382,-2.16871600557743,-2.41415616437785));
#50544=CARTESIAN_POINT('Ctrl Pts',(375.019436597687,-2.36723212298908,2.03396679848696));
#50545=CARTESIAN_POINT('Ctrl Pts',(371.393952387734,-2.56574824040074,4.61942035370964));
#50546=CARTESIAN_POINT('Ctrl Pts',(367.255965826352,-2.7642643578124,2.97449724855164));
#50547=CARTESIAN_POINT('Ctrl Pts',(366.39496583423,-2.96278047522405,-1.39441415921852));
#50548=CARTESIAN_POINT('Ctrl Pts',(369.599440047773,-3.16129659263571,-4.48634745823798));
#50549=CARTESIAN_POINT('Ctrl Pts',(373.934791830905,-3.35981271004736,-3.46976916495197));
#50550=CARTESIAN_POINT('Ctrl Pts',(375.430788539321,-3.55832882745902,0.724357761628879));
#50551=CARTESIAN_POINT('Ctrl Pts',(372.717424819462,-3.75684494487067,4.25513161243665));
#50552=CARTESIAN_POINT('Ctrl Pts',(368.279547564317,-3.95536106228233,3.88913688168041));
#50553=CARTESIAN_POINT('Ctrl Pts',(366.181280340988,-4.15387717969399,-0.0384554299109293));
#50554=CARTESIAN_POINT('Ctrl Pts',(368.344176362114,-4.35239329710564,-3.93083098844711));
#50555=CARTESIAN_POINT('Ctrl Pts',(372.787496592847,-4.5509094145173,-4.22342630098604));
#50556=CARTESIAN_POINT('Ctrl Pts',(375.442132887444,-4.74942553192896,-0.6482881447401));
#50557=CARTESIAN_POINT('Ctrl Pts',(373.877019823537,-4.94794164934061,3.52053996250392));
#50558=CARTESIAN_POINT('Ctrl Pts',(369.525458173596,-5.14645776675227,4.46532453995758));
#50559=CARTESIAN_POINT('Ctrl Pts',(366.372525321083,-5.34497388416392,1.32084984314923));
#50560=CARTESIAN_POINT('Ctrl Pts',(367.305617197225,-5.54349000157558,-3.03323401476381));
#50561=CARTESIAN_POINT('Ctrl Pts',(371.470226011121,-5.74200611898723,-4.60953986019632));
#50562=CARTESIAN_POINT('Ctrl Pts',(375.052482230274,-5.94052223639889,-1.96451678440118));
#50563=CARTESIAN_POINT('Ctrl Pts',(374.771823750919,-6.13903835381055,2.47957339347431));
#50564=CARTESIAN_POINT('Ctrl Pts',(370.885272269759,-6.3375544712222,4.65291742409449));
#50565=CARTESIAN_POINT('Ctrl Pts',(366.952057703193,-6.53607058863387,2.56520818560264));
#50566=CARTESIAN_POINT('Ctrl Pts',(366.574143133607,-6.73458670604551,-1.87166991383015));
#50567=CARTESIAN_POINT('Ctrl Pts',(370.09761553513,-6.93310282345717,-4.59450830911431));
#50568=CARTESIAN_POINT('Ctrl Pts',(374.295745906001,-7.13161894086883,-3.10978339172664));
#50569=CARTESIAN_POINT('Ctrl Pts',(375.323966309482,-7.33013505828048,1.22282200145175));
#50570=CARTESIAN_POINT('Ctrl Pts',(372.240652058892,-7.52865117569214,4.43559026624153));
#50571=CARTESIAN_POINT('Ctrl Pts',(367.869443694065,-7.7271672931038,3.58632933908072));
#50572=CARTESIAN_POINT('Ctrl Pts',(366.21341068631,-7.92568341051545,-0.547223777592583));
#50573=CARTESIAN_POINT('Ctrl Pts',(368.789116563041,-8.1241995279271,-4.1796397680466));
#50574=CARTESIAN_POINT('Ctrl Pts',(373.237778877468,-8.32271564533876,-3.9844211641022));
#50575=CARTESIAN_POINT('Ctrl Pts',(375.48539730457,-8.52123176275041,-0.140345449800097));
#50576=CARTESIAN_POINT('Ctrl Pts',(373.473645643041,-8.71974788016207,3.83225595777542));
#50577=CARTESIAN_POINT('Ctrl Pts',(369.044847796937,-8.91826399757373,4.29535025645813));
#50578=CARTESIAN_POINT('Ctrl Pts',(366.25481258905,-9.11678011498538,0.824844496502067));
#50579=CARTESIAN_POINT('Ctrl Pts',(367.658601190669,-9.31529623239705,-3.40103816314458));
#50580=CARTESIAN_POINT('Ctrl Pts',(371.970650703318,-9.5138123498087,-4.51231476758915));
#50581=CARTESIAN_POINT('Ctrl Pts',(375.242068207196,-9.71232846722035,-1.49129934120374));
#50582=CARTESIAN_POINT('Ctrl Pts',(374.476951781207,-9.91084458463201,2.89541965433465));
#50583=CARTESIAN_POINT('Ctrl Pts',(370.375980494218,-10.1093607020436,4.63056840715521));
#50584=CARTESIAN_POINT('Ctrl Pts',(366.694745842105,-10.3078768194553,2.12513069545394));
#50585=CARTESIAN_POINT('Ctrl Pts',(366.804452494766,-10.5063929368669,-2.32646128287183));
#50586=CARTESIAN_POINT('Ctrl Pts',(370.604633186536,-10.7049090542786,-4.64752427232966));
#50587=CARTESIAN_POINT('Ctrl Pts',(374.615154726994,-10.9034251716902,-2.71247293847364));
#50588=CARTESIAN_POINT('Ctrl Pts',(375.163257777597,-11.1019412891019,1.70660951573022));
#50589=CARTESIAN_POINT('Ctrl Pts',(371.746999990629,-11.3004574065136,4.56281143858355));
#50590=CARTESIAN_POINT('Ctrl Pts',(367.49492526328,-11.4989735239252,3.24047743985877));
#50591=CARTESIAN_POINT('Ctrl Pts',(366.301002747821,-11.6974896413369,-1.04942415787176));
#50592=CARTESIAN_POINT('Ctrl Pts',(369.258603973092,-11.8960057587485,-4.37828307398747));
#50593=CARTESIAN_POINT('Ctrl Pts',(373.659213996533,-12.0945218761602,-3.6975936347205));
#50594=CARTESIAN_POINT('Ctrl Pts',(375.472837867153,-12.2930379935718,0.369281719534577));
#50595=CARTESIAN_POINT('Ctrl Pts',(373.038593343025,-12.4915541109835,4.09797589952302));
#50596=CARTESIAN_POINT('Ctrl Pts',(368.585715255102,-12.6900702283951,4.07382170249547));
#50597=CARTESIAN_POINT('Ctrl Pts',(366.192064653583,-12.8885863458068,0.318939082628224));
#50598=CARTESIAN_POINT('Ctrl Pts',(368.049701227277,-13.0871024632185,-3.72802188224533));
#50599=CARTESIAN_POINT('Ctrl Pts',(372.457436737988,-13.2856185806301,-4.36093132185416));
#50600=CARTESIAN_POINT('Ctrl Pts',(375.378750849028,-13.4841346980418,-1.00018281061867));
#50601=CARTESIAN_POINT('Ctrl Pts',(374.138359666792,-13.6826508154534,3.27651409308701));
#50602=CARTESIAN_POINT('Ctrl Pts',(369.872189841231,-13.8811669328651,4.55264171625033));
#50603=CARTESIAN_POINT('Ctrl Pts',(366.487118547438,-14.0796830502768,1.65954665609971));
#50604=CARTESIAN_POINT('Ctrl Pts',(367.083129685385,-14.2781991676884,-2.75332966378236));
#50605=CARTESIAN_POINT('Ctrl Pts',(371.114407592274,-14.4767152851001,-4.64475905145618));
#50606=CARTESIAN_POINT('Ctrl Pts',(374.889184644014,-14.6752314025117,-2.28260645249201));
#50607=CARTESIAN_POINT('Ctrl Pts',(374.950591820493,-14.8737475199233,2.16991371588561));
#50608=CARTESIAN_POINT('Ctrl Pts',(371.242393597581,-15.072263637335,4.63526817939077));
#50609=CARTESIAN_POINT('Ctrl Pts',(367.160487370411,-15.2707797547467,2.85573221635991));
#50610=CARTESIAN_POINT('Ctrl Pts',(366.443005215735,-15.4692958721583,-1.53902898862659));
#50611=CARTESIAN_POINT('Ctrl Pts',(369.747003642848,-15.66781198957,-4.52437672126445));
#50612=CARTESIAN_POINT('Ctrl Pts',(374.046743740915,-15.8663281069816,-3.36638631533918));
#50613=CARTESIAN_POINT('Ctrl Pts',(375.404605317853,-16.0648442243933,0.874476642716028));
#50614=CARTESIAN_POINT('Ctrl Pts',(372.577084570772,-16.2633603418049,4.31451052568145));
#50615=CARTESIAN_POINT('Ctrl Pts',(368.153571214698,-16.4618764592166,3.80339773992032));
#50616=CARTESIAN_POINT('Ctrl Pts',(366.185034636979,-16.6603925766283,-0.190794347763422));
#50617=CARTESIAN_POINT('Ctrl Pts',(368.474223189953,-16.8589086940399,-4.01026060105872));
#50618=CARTESIAN_POINT('Ctrl Pts',(372.924741541791,-17.0574248114516,-4.15720647914977));
#50619=CARTESIAN_POINT('Ctrl Pts',(375.460889643715,-17.2559409288632,-0.497061742087704));
#50620=CARTESIAN_POINT('Ctrl Pts',(373.760111306634,-17.4544570462749,3.61828268326134));
#50621=CARTESIAN_POINT('Ctrl Pts',(369.379946979415,-17.6529731636865,4.42007265431438));
#50622=CARTESIAN_POINT('Ctrl Pts',(366.331667833362,-17.8514892810982,1.17404416724334));
#50623=CARTESIAN_POINT('Ctrl Pts',(367.406829926015,-18.0500053985099,-3.1471516355009));
#50624=CARTESIAN_POINT('Ctrl Pts',(371.620820264673,-18.2485215159215,-4.58624583562557));
#50625=CARTESIAN_POINT('Ctrl Pts',(375.114546655788,-18.4470376333332,-1.82534333913001));
#50626=CARTESIAN_POINT('Ctrl Pts',(374.688520928102,-18.6455537507448,2.60717386562768));
#50627=CARTESIAN_POINT('Ctrl Pts',(370.732889339158,-18.8440698681565,4.65209083795145));
#50628=CARTESIAN_POINT('Ctrl Pts',(366.870144054024,-19.0425859855681,2.43671151302536));
#50629=CARTESIAN_POINT('Ctrl Pts',(366.63771372761,-19.2411021029798,-2.01016186435141));
#50630=CARTESIAN_POINT('Ctrl Pts',(370.248453631574,-19.4396182203914,-4.61616724370937));
#50631=CARTESIAN_POINT('Ctrl Pts',(374.395716845375,-19.6381343378031,-2.9947744700463));
#50632=CARTESIAN_POINT('Ctrl Pts',(375.281518607221,-19.8366504552148,1.36917579654363));
#50633=CARTESIAN_POINT('Ctrl Pts',(372.094658513152,-20.0351665726264,4.47926091333222));
#50634=CARTESIAN_POINT('Ctrl Pts',(367.753602417219,-20.2336826900381,3.48732408987848));
#50635=CARTESIAN_POINT('Ctrl Pts',(366.233806915586,-20.4321988074497,-0.698237798339605));
#50636=CARTESIAN_POINT('Ctrl Pts',(368.927071820833,-20.6307149248614,-4.24436679440525));
#50637=CARTESIAN_POINT('Ctrl Pts',(373.366956360414,-20.8292310422731,-3.90358541309778));
#50638=CARTESIAN_POINT('Ctrl Pts',(375.487498736112,-21.0277471596847,0.0120252282541951));
#50639=CARTESIAN_POINT('Ctrl Pts',(373.346746561559,-21.2262632770964,3.91662340924706));
#50640=CARTESIAN_POINT('Ctrl Pts',(368.905159989326,-21.424779394508,4.23445234317155));
#50641=CARTESIAN_POINT('Ctrl Pts',(366.230259446871,-21.6232955119197,0.674450433223809));
#50642=CARTESIAN_POINT('Ctrl Pts',(367.77166810882,-21.8218116293313,-3.50320048712016));
#50643=CARTESIAN_POINT('Ctrl Pts',(372.117792953331,-22.020327746743,-4.47268676344431));
#50644=CARTESIAN_POINT('Ctrl Pts',(375.288536120941,-22.2188438641546,-1.34617215323029));
#50645=CARTESIAN_POINT('Ctrl Pts',(374.380190086528,-22.4173599815663,3.01314249366513));
#50646=CARTESIAN_POINT('Ctrl Pts',(370.224603453362,-22.6158760989779,4.61307610279703));
#50647=CARTESIAN_POINT('Ctrl Pts',(366.627378056288,-22.8143922163896,1.98844746315212));
#50648=CARTESIAN_POINT('Ctrl Pts',(366.882795591862,-23.0129083338012,-2.45717410429654));
#50649=CARTESIAN_POINT('Ctrl Pts',(370.756926517952,-23.2114244512129,-4.65254046342319));
#50650=CARTESIAN_POINT('Ctrl Pts',(374.701963154568,-23.4099405686247,-2.58724417820185));
#50651=CARTESIAN_POINT('Ctrl Pts',(375.105017042159,-23.6084566860362,1.84749525744088));
#50652=CARTESIAN_POINT('Ctrl Pts',(371.597184240534,-23.8069728034479,4.59013849390895));
#50653=CARTESIAN_POINT('Ctrl Pts',(367.390445996853,-24.0054889208595,3.12962485931625));
#50654=CARTESIAN_POINT('Ctrl Pts',(366.338134868135,-24.2040050382713,-1.19777877140987));
#50655=CARTESIAN_POINT('Ctrl Pts',(369.402108736586,-24.4025211556828,-4.42654123220031));
#50656=CARTESIAN_POINT('Ctrl Pts',(373.780221960378,-24.6010372730946,-3.60519568839286));
#50657=CARTESIAN_POINT('Ctrl Pts',(375.455117166712,-24.7995533905062,0.525090591169996));
#50658=CARTESIAN_POINT('Ctrl Pts',(373.757258810431,-24.9318974687806,2.94371710434112));
#50659=CARTESIAN_POINT('Ctrl Pts',(372.584499012473,-24.9980695079178,3.52585701865193));
#50660=CARTESIAN_POINT('Ctrl Pts',(372.978942820004,0.273648433802759,-3.01074479622233));
#50661=CARTESIAN_POINT('Ctrl Pts',(373.981112519162,0.207430584100572,-2.29695958120762));
#50662=CARTESIAN_POINT('Ctrl Pts',(375.197411211422,0.0750406952611682,
0.198848743302471));
#50663=CARTESIAN_POINT('Ctrl Pts',(373.030208660887,-0.123521232715456,
3.78057276473135));
#50664=CARTESIAN_POINT('Ctrl Pts',(368.848625221144,-0.322037350127111,
3.89165448718187));
#50665=CARTESIAN_POINT('Ctrl Pts',(366.487325325364,-0.520553467538767,
0.442581674952212));
#50666=CARTESIAN_POINT('Ctrl Pts',(368.106032678174,-0.719069584950422,
-3.41359402405725));
#50667=CARTESIAN_POINT('Ctrl Pts',(372.223678526374,-0.917585702362079,
-4.14279884959533));
#50668=CARTESIAN_POINT('Ctrl Pts',(375.06876838223,-1.11610181977374,-1.07852512752762));
#50669=CARTESIAN_POINT('Ctrl Pts',(374.036128311705,-1.31461793718539,2.9736429358834));
#50670=CARTESIAN_POINT('Ctrl Pts',(370.071283221154,-1.51313405459705,4.30250814899426));
#50671=CARTESIAN_POINT('Ctrl Pts',(366.805233839984,-1.71165017200871,1.69126513267051));
#50672=CARTESIAN_POINT('Ctrl Pts',(367.228931810867,-1.91016628942036,-2.46882893861279));
#50673=CARTESIAN_POINT('Ctrl Pts',(370.954379113847,-2.10868240683202,-4.36800552042992));
#50674=CARTESIAN_POINT('Ctrl Pts',(374.569874004953,-2.30719852424367,-2.26705099711807));
#50675=CARTESIAN_POINT('Ctrl Pts',(374.764418880942,-2.50571464165533,1.91002824367964));
#50676=CARTESIAN_POINT('Ctrl Pts',(371.359851390864,-2.70423075906698,4.33793872720901));
#50677=CARTESIAN_POINT('Ctrl Pts',(367.474010574738,-2.90274687647864,2.79324803123983));
#50678=CARTESIAN_POINT('Ctrl Pts',(366.665475104059,-3.10126299389029,-1.30944636337006));
#50679=CARTESIAN_POINT('Ctrl Pts',(369.674686590973,-3.29977911130195,-4.21297454932363));
#50680=CARTESIAN_POINT('Ctrl Pts',(373.745866296675,-3.4982952287136,-3.25834084855114));
#50681=CARTESIAN_POINT('Ctrl Pts',(375.15070533714,-3.69681134612527,0.680219453075119));
#50682=CARTESIAN_POINT('Ctrl Pts',(372.602678818635,-3.89532746353692,3.99584770330267));
#50683=CARTESIAN_POINT('Ctrl Pts',(368.435220969462,-4.09384358094858,3.65215464336561));
#50684=CARTESIAN_POINT('Ctrl Pts',(366.464810409011,-4.29235969836023,-0.0361121712052552));
#50685=CARTESIAN_POINT('Ctrl Pts',(368.495911649978,-4.49087581577189,-3.69130814458238));
#50686=CARTESIAN_POINT('Ctrl Pts',(372.668480810263,-4.68939193318354,-3.96607433611181));
#50687=CARTESIAN_POINT('Ctrl Pts',(375.16135842417,-4.8879080505952,-0.60878509296087));
#50688=CARTESIAN_POINT('Ctrl Pts',(373.691614592148,-5.08642416800685,3.30601795780906));
#50689=CARTESIAN_POINT('Ctrl Pts',(369.605212758213,-5.28494028541851,4.19323265004089));
#50690=CARTESIAN_POINT('Ctrl Pts',(366.644401990209,-5.48345640283016,1.24036464506279));
#50691=CARTESIAN_POINT('Ctrl Pts',(367.520636468914,-5.68197252024182,-2.84840570760466));
#50692=CARTESIAN_POINT('Ctrl Pts',(371.431477326463,-5.88048863765348,-4.32866029568004));
#50693=CARTESIAN_POINT('Ctrl Pts',(374.795450897599,-6.07900475506513,-1.84481012481627));
#50694=CARTESIAN_POINT('Ctrl Pts',(374.531894175436,-6.27752087247679,2.32848206634227));
#50695=CARTESIAN_POINT('Ctrl Pts',(370.882167392752,-6.47603698988844,4.36939467357115));
#50696=CARTESIAN_POINT('Ctrl Pts',(367.188620911962,-6.6745531073001,2.40889875344273));
#50697=CARTESIAN_POINT('Ctrl Pts',(366.833734341472,-6.87306922471176,-1.75762082297527));
#50698=CARTESIAN_POINT('Ctrl Pts',(370.142506051877,-7.07158534212341,-4.31454468320579));
#50699=CARTESIAN_POINT('Ctrl Pts',(374.0848258503,-7.27010145953507,-2.92029059389866));
#50700=CARTESIAN_POINT('Ctrl Pts',(375.050392256219,-7.46861757694672,1.14831007148355));
#50701=CARTESIAN_POINT('Ctrl Pts',(372.154957922116,-7.66713369435838,4.16531021657482));
#50702=CARTESIAN_POINT('Ctrl Pts',(368.050106534158,-7.86564981177004,3.36779849792858));
#50703=CARTESIAN_POINT('Ctrl Pts',(366.494982910887,-8.06416592918169,-0.513879022800399));
#50704=CARTESIAN_POINT('Ctrl Pts',(368.913739684905,-8.26268204659335,-3.92495590946429));
#50705=CARTESIAN_POINT('Ctrl Pts',(373.091325412199,-8.461198164005,-3.74163283481876));
#50706=CARTESIAN_POINT('Ctrl Pts',(375.201986549821,-8.65971428141666,-0.131793583449574));
#50707=CARTESIAN_POINT('Ctrl Pts',(373.312819776967,-8.85823039882831,3.59873972466296));
#50708=CARTESIAN_POINT('Ctrl Pts',(369.153888088456,-9.05674651623997,4.03361564821732));
#50709=CARTESIAN_POINT('Ctrl Pts',(366.533862013356,-9.25526263365163,0.774583088639681));
#50710=CARTESIAN_POINT('Ctrl Pts',(367.852111593064,-9.45377875106327,-3.19379792938153));
#50711=CARTESIAN_POINT('Ctrl Pts',(371.901408938249,-9.65229486847494,-4.2373595561536));
#50712=CARTESIAN_POINT('Ctrl Pts',(374.973484565992,-9.85081098588659,-1.40042790452567));
#50713=CARTESIAN_POINT('Ctrl Pts',(374.254990053484,-10.0493271032982,2.71898898310347));
#50714=CARTESIAN_POINT('Ctrl Pts',(370.403909008062,-10.2478432207099,4.3484074806611));
#50715=CARTESIAN_POINT('Ctrl Pts',(366.946988195795,-10.4463593381215,1.99563712291025));
#50716=CARTESIAN_POINT('Ctrl Pts',(367.050009938952,-10.6448754555332,-2.18469975095852));
#50717=CARTESIAN_POINT('Ctrl Pts',(370.618628884829,-10.8433915729448,-4.36433015029528));
#50718=CARTESIAN_POINT('Ctrl Pts',(374.384771685124,-11.0419076903565,-2.54719001635388));
#50719=CARTESIAN_POINT('Ctrl Pts',(374.899476402958,-11.2404238077681,1.60261828187263));
#50720=CARTESIAN_POINT('Ctrl Pts',(371.691386248461,-11.4389399251798,4.28477924259238));
#50721=CARTESIAN_POINT('Ctrl Pts',(367.698409160776,-11.6374560425915,3.04302087808957));
#50722=CARTESIAN_POINT('Ctrl Pts',(366.577237602327,-11.8359721600031,-0.98547812217283));
#50723=CARTESIAN_POINT('Ctrl Pts',(369.354619159398,-12.0344882774148,-4.11149500393091));
#50724=CARTESIAN_POINT('Ctrl Pts',(373.48708063342,-12.2330043948264,-3.47228297001692));
#50725=CARTESIAN_POINT('Ctrl Pts',(375.190192414239,-12.4315205122381,0.346779758012944));
#50726=CARTESIAN_POINT('Ctrl Pts',(372.904277129601,-12.6300366296497,3.84826818010499));
#50727=CARTESIAN_POINT('Ctrl Pts',(368.722732514457,-12.8285527470614,3.82558580467959));
#50728=CARTESIAN_POINT('Ctrl Pts',(366.474937585944,-13.027068864473,0.299504719686812));
#50729=CARTESIAN_POINT('Ctrl Pts',(368.219380182002,-13.2255849818847,-3.5008570904113));
#50730=CARTESIAN_POINT('Ctrl Pts',(372.358532955975,-13.4241010992964,-4.09520057047378));
#50731=CARTESIAN_POINT('Ctrl Pts',(375.101838532497,-13.622617216708,-0.939237267071211));
#50732=CARTESIAN_POINT('Ctrl Pts',(373.93702984779,-13.8211333341197,3.07686165932794));
#50733=CARTESIAN_POINT('Ctrl Pts',(369.930816538302,-14.0196494515313,4.2752292062293));
#50734=CARTESIAN_POINT('Ctrl Pts',(366.752012546602,-14.218165568943,1.55842316954849));
#50735=CARTESIAN_POINT('Ctrl Pts',(367.311706101026,-14.4166816863546,-2.58555716145282));
#50736=CARTESIAN_POINT('Ctrl Pts',(371.097340490933,-14.6151978037663,-4.3617334265079));
#50737=CARTESIAN_POINT('Ctrl Pts',(374.642103752447,-14.8137139211779,-2.14351718853437));
#50738=CARTESIAN_POINT('Ctrl Pts',(374.699769119222,-15.0122300385896,2.03769131667855));
#50739=CARTESIAN_POINT('Ctrl Pts',(371.217527745275,-15.2107461560013,4.35282087507611));
#50740=CARTESIAN_POINT('Ctrl Pts',(367.384350041614,-15.4092622734129,2.68171987551159));
#50741=CARTESIAN_POINT('Ctrl Pts',(366.710587234479,-15.6077783908246,-1.44524917432538));
#50742=CARTESIAN_POINT('Ctrl Pts',(369.813258486318,-15.8062945082362,-4.24868652186954));
#50743=CARTESIAN_POINT('Ctrl Pts',(373.85099648376,-16.0048106256479,-3.16125757127277));
#50744=CARTESIAN_POINT('Ctrl Pts',(375.126117574671,-16.2033267430595,0.821190929600369));
#50745=CARTESIAN_POINT('Ctrl Pts',(372.470890119367,-16.4018428604712,4.05160839785332));
#50746=CARTESIAN_POINT('Ctrl Pts',(368.316920913637,-16.6003589778829,3.57163996511596));
#50747=CARTESIAN_POINT('Ctrl Pts',(366.468335939212,-16.7988750952945,-0.179168407878488));
#50748=CARTESIAN_POINT('Ctrl Pts',(368.618034151859,-16.9973912127062,-3.7658977610823));
#50749=CARTESIAN_POINT('Ctrl Pts',(372.79736282003,-17.1959073301178,-3.90388957965816));
#50750=CARTESIAN_POINT('Ctrl Pts',(375.178972248675,-17.3944234475295,-0.46677358103697));
#50751=CARTESIAN_POINT('Ctrl Pts',(373.581829826057,-17.5929395649411,3.39780478412287));
#50752=CARTESIAN_POINT('Ctrl Pts',(369.468568201937,-17.7914556823528,4.15073816108335));
#50753=CARTESIAN_POINT('Ctrl Pts',(366.606034129154,-17.9899717997644,1.10250448553545));
#50754=CARTESIAN_POINT('Ctrl Pts',(367.615681860389,-18.1884879171761,-2.95538182600663));
#50755=CARTESIAN_POINT('Ctrl Pts',(371.572895208915,-18.3870040345878,-4.3067856786154));
#50756=CARTESIAN_POINT('Ctrl Pts',(374.853733464329,-18.5855201519994,-1.71411713049803));
#50757=CARTESIAN_POINT('Ctrl Pts',(374.453667360487,-18.7840362694111,2.4483072797632));
#50758=CARTESIAN_POINT('Ctrl Pts',(370.739069825219,-18.9825523868227,4.36861845496217));
#50759=CARTESIAN_POINT('Ctrl Pts',(367.111698622193,-19.1810685042344,2.28823194903666));
#50760=CARTESIAN_POINT('Ctrl Pts',(366.893431299211,-19.379584621646,-1.88767384902007));
#50761=CARTESIAN_POINT('Ctrl Pts',(370.284152918798,-19.5781007390577,-4.33488384352804));
#50762=CARTESIAN_POINT('Ctrl Pts',(374.178705120057,-19.7766168564694,-2.81228967232609));
#50763=CARTESIAN_POINT('Ctrl Pts',(375.010531079402,-19.975132973881,1.28574588528499));
#50764=CARTESIAN_POINT('Ctrl Pts',(372.017860406087,-20.1736490912927,4.20631981880876));
#50765=CARTESIAN_POINT('Ctrl Pts',(367.941323976487,-20.3721652087043,3.2748260745884));
#50766=CARTESIAN_POINT('Ctrl Pts',(366.514136308087,-20.570681326116,-0.655691094183771));
#50767=CARTESIAN_POINT('Ctrl Pts',(369.043288721271,-20.7691974435276,-3.98573883304316));
#50768=CARTESIAN_POINT('Ctrl Pts',(373.2126315422,-20.9677135609393,-3.66572276213106));
#50769=CARTESIAN_POINT('Ctrl Pts',(375.203959931884,-21.1662296783509,0.0112924781364861));
#50770=CARTESIAN_POINT('Ctrl Pts',(373.193653215394,-21.3647457957626,3.67796629575447));
#50771=CARTESIAN_POINT('Ctrl Pts',(369.02271207416,-21.5632619131742,3.97642851298726));
#50772=CARTESIAN_POINT('Ctrl Pts',(366.510805002264,-21.7617780305859,0.633353197986158));
#50773=CARTESIAN_POINT('Ctrl Pts',(367.958288845935,-21.9602941479975,-3.28973505302508));
#50774=CARTESIAN_POINT('Ctrl Pts',(372.039585162939,-22.1588102654092,-4.20014626082667));
#50775=CARTESIAN_POINT('Ctrl Pts',(375.017120985105,-22.3573263828208,-1.26414395526884));
#50776=CARTESIAN_POINT('Ctrl Pts',(374.164124475008,-22.5558425002325,2.82953845137142));
#50777=CARTESIAN_POINT('Ctrl Pts',(370.261756036983,-22.7543586176442,4.33198105944515));
#50778=CARTESIAN_POINT('Ctrl Pts',(366.883725425863,-22.9528747350558,1.86728260191802));
#50779=CARTESIAN_POINT('Ctrl Pts',(367.123579246112,-23.1513908524675,-2.30744766450261));
#50780=CARTESIAN_POINT('Ctrl Pts',(370.761642312849,-23.3499069698792,-4.36904068277373));
#50781=CARTESIAN_POINT('Ctrl Pts',(374.466290492894,-23.5484230872908,-2.42959199596435));
#50782=CARTESIAN_POINT('Ctrl Pts',(374.844784532027,-23.7469392047025,1.73491923486719));
#50783=CARTESIAN_POINT('Ctrl Pts',(371.550699431823,-23.9454553221141,4.31044114008596));
#50784=CARTESIAN_POINT('Ctrl Pts',(367.600296276188,-24.1439714395258,2.9389230334844));
#50785=CARTESIAN_POINT('Ctrl Pts',(366.612107099017,-24.3424875569374,-1.1247928357408));
#50786=CARTESIAN_POINT('Ctrl Pts',(369.489379545642,-24.5410036743491,-4.15681258003051));
#50787=CARTESIAN_POINT('Ctrl Pts',(373.600715049098,-24.7395197917607,-3.38551523748801));
#50788=CARTESIAN_POINT('Ctrl Pts',(375.173551514119,-24.9380359091724,0.493094508903115));
#50789=CARTESIAN_POINT('Ctrl Pts',(373.579151145009,-25.0703799874468,2.76434345677467));
#50790=CARTESIAN_POINT('Ctrl Pts',(372.477852766483,-25.1365520265841,3.31101102230916));
#50791=CARTESIAN_POINT('Ctrl Pts',(372.83978167416,0.135165915136521,-2.81538257570422));
#50792=CARTESIAN_POINT('Ctrl Pts',(373.776922248958,0.0689480654343353,
-2.14791369568849));
#50793=CARTESIAN_POINT('Ctrl Pts',(374.91429734277,-0.0634418234050692,
0.185945779196225));
#50794=CARTESIAN_POINT('Ctrl Pts',(372.887720959923,-0.262003751381692,
3.53525768818457));
#50795=CARTESIAN_POINT('Ctrl Pts',(368.977473512224,-0.460519868793348,
3.63913150248418));
#50796=CARTESIAN_POINT('Ctrl Pts',(366.769394437926,-0.659035986205004,
0.413863286436573));
#50797=CARTESIAN_POINT('Ctrl Pts',(368.283066563833,-0.85755210361666,-3.19209158740974));
#50798=CARTESIAN_POINT('Ctrl Pts',(372.133525223925,-1.05606822102832,-3.87397952507726));
#50799=CARTESIAN_POINT('Ctrl Pts',(374.794001932725,-1.25458433843997,-1.00854142646374));
#50800=CARTESIAN_POINT('Ctrl Pts',(373.82836815826,-1.45310045585163,2.78068819335224));
#50801=CARTESIAN_POINT('Ctrl Pts',(370.120795268885,-1.65161657326328,4.02332555376421));
#50802=CARTESIAN_POINT('Ctrl Pts',(367.066674397972,-1.85013269067494,1.58152175215617));
#50803=CARTESIAN_POINT('Ctrl Pts',(367.462879312477,-2.04864880808659,-2.30863073644972));
#50804=CARTESIAN_POINT('Ctrl Pts',(370.946588538405,-2.24716492549825,-4.08457290974263));
#50805=CARTESIAN_POINT('Ctrl Pts',(374.327479981526,-2.44568104290991,-2.11994582985829));
#50806=CARTESIAN_POINT('Ctrl Pts',(374.509401164196,-2.64419716032156,1.78608968887232));
#50807=CARTESIAN_POINT('Ctrl Pts',(371.325750393995,-2.84271327773322,4.05645710070838));
#50808=CARTESIAN_POINT('Ctrl Pts',(367.692055323125,-3.04122939514487,2.61199881392804));
#50809=CARTESIAN_POINT('Ctrl Pts',(366.935984373887,-3.23974551255653,-1.2244785675216));
#50810=CARTESIAN_POINT('Ctrl Pts',(369.749933134175,-3.43826162996819,-3.93960164040927));
#50811=CARTESIAN_POINT('Ctrl Pts',(373.556940762444,-3.63677774737984,-3.04691253215032));
#50812=CARTESIAN_POINT('Ctrl Pts',(374.870622134959,-3.8352938647915,0.636081144521366));
#50813=CARTESIAN_POINT('Ctrl Pts',(372.487932817806,-4.03380998220315,3.7365637941687));
#50814=CARTESIAN_POINT('Ctrl Pts',(368.590894374608,-4.23232609961481,3.4151724050508));
#50815=CARTESIAN_POINT('Ctrl Pts',(366.748340477034,-4.43084221702647,-0.033768912499581));
#50816=CARTESIAN_POINT('Ctrl Pts',(368.647646937842,-4.62935833443813,-3.45178530071766));
#50817=CARTESIAN_POINT('Ctrl Pts',(372.549465027681,-4.82787445184977,-3.70872237123758));
#50818=CARTESIAN_POINT('Ctrl Pts',(374.880583960898,-5.02639056926144,-0.569282041181633));
#50819=CARTESIAN_POINT('Ctrl Pts',(373.506209360759,-5.22490668667309,3.0914959531142));
#50820=CARTESIAN_POINT('Ctrl Pts',(369.684967342831,-5.42342280408475,3.9211407601242));
#50821=CARTESIAN_POINT('Ctrl Pts',(366.916278659333,-5.6219389214964,1.15987944697635));
#50822=CARTESIAN_POINT('Ctrl Pts',(367.735655740605,-5.82045503890806,-2.66357740044551));
#50823=CARTESIAN_POINT('Ctrl Pts',(371.392728641804,-6.01897115631971,-4.04778073116377));
#50824=CARTESIAN_POINT('Ctrl Pts',(374.538419564924,-6.21748727373136,-1.72510346523135));
#50825=CARTESIAN_POINT('Ctrl Pts',(374.291964599955,-6.41600339114303,2.17739073921023));
#50826=CARTESIAN_POINT('Ctrl Pts',(370.879062515744,-6.61451950855468,4.08587192304781));
#50827=CARTESIAN_POINT('Ctrl Pts',(367.425184120733,-6.81303562596634,2.25258932128282));
#50828=CARTESIAN_POINT('Ctrl Pts',(367.093325549337,-7.01155174337799,-1.64357173212039));
#50829=CARTESIAN_POINT('Ctrl Pts',(370.187396568622,-7.21006786078965,-4.03458105729727));
#50830=CARTESIAN_POINT('Ctrl Pts',(373.873905794599,-7.4085839782013,-2.73079779607067));
#50831=CARTESIAN_POINT('Ctrl Pts',(374.776818202958,-7.60710009561296,1.07379814151536));
#50832=CARTESIAN_POINT('Ctrl Pts',(372.06926378534,-7.80561621302462,3.89503016690812));
#50833=CARTESIAN_POINT('Ctrl Pts',(368.230769374253,-8.00413233043627,3.14926765677645));
#50834=CARTESIAN_POINT('Ctrl Pts',(366.776555135465,-8.20264844784792,-0.480534268008217));
#50835=CARTESIAN_POINT('Ctrl Pts',(369.038362806769,-8.40116456525959,-3.67027205088198));
#50836=CARTESIAN_POINT('Ctrl Pts',(372.94487194693,-8.59968068267123,-3.49884450553532));
#50837=CARTESIAN_POINT('Ctrl Pts',(374.918575795071,-8.7981968000829,-0.123241717099051));
#50838=CARTESIAN_POINT('Ctrl Pts',(373.151993910893,-8.99671291749455,3.3652234915505));
#50839=CARTESIAN_POINT('Ctrl Pts',(369.262928379975,-9.19522903490621,3.77188103997652));
#50840=CARTESIAN_POINT('Ctrl Pts',(366.812911437662,-9.39374515231786,0.724321680777291));
#50841=CARTESIAN_POINT('Ctrl Pts',(368.045621995459,-9.59226126972952,-2.98655769561848));
#50842=CARTESIAN_POINT('Ctrl Pts',(371.832167173178,-9.79077738714117,-3.96240434471807));
#50843=CARTESIAN_POINT('Ctrl Pts',(374.704900924791,-9.98929350455282,-1.30955646784761));
#50844=CARTESIAN_POINT('Ctrl Pts',(374.033028325759,-10.1878096219645,2.54255831187231));
#50845=CARTESIAN_POINT('Ctrl Pts',(370.431837521906,-10.3863257393761,4.06624655416697));
#50846=CARTESIAN_POINT('Ctrl Pts',(367.199230549486,-10.5848418567878,1.86614355036656));
#50847=CARTESIAN_POINT('Ctrl Pts',(367.295567383138,-10.7833579741994,-2.04293821904521));
#50848=CARTESIAN_POINT('Ctrl Pts',(370.632624583124,-10.9818740916111,-4.0811360282609));
#50849=CARTESIAN_POINT('Ctrl Pts',(374.154388643254,-11.1803902090227,-2.38190709423413));
#50850=CARTESIAN_POINT('Ctrl Pts',(374.635695028319,-11.3789063264344,1.49862704801505));
#50851=CARTESIAN_POINT('Ctrl Pts',(371.635772506293,-11.577422443846,4.00674704660121));
#50852=CARTESIAN_POINT('Ctrl Pts',(367.901893058271,-11.7759385612577,2.84556431632038));
#50853=CARTESIAN_POINT('Ctrl Pts',(366.853472456833,-11.9744546786694,-0.921532086473897));
#50854=CARTESIAN_POINT('Ctrl Pts',(369.450634345702,-12.172970796081,-3.84470693387437));
#50855=CARTESIAN_POINT('Ctrl Pts',(373.314947270308,-12.3714869134927,-3.24697230531333));
#50856=CARTESIAN_POINT('Ctrl Pts',(374.907546961325,-12.5700030309043,0.32427779649131));
#50857=CARTESIAN_POINT('Ctrl Pts',(372.769960916176,-12.768519148316,3.59856046068695));
#50858=CARTESIAN_POINT('Ctrl Pts',(368.859749773812,-12.9670352657276,3.57734990686372));
#50859=CARTESIAN_POINT('Ctrl Pts',(366.757810518306,-13.1655513831393,0.280070356745402));
#50860=CARTESIAN_POINT('Ctrl Pts',(368.389059136727,-13.3640675005509,-3.27369229857728));
#50861=CARTESIAN_POINT('Ctrl Pts',(372.259629173963,-13.5625836179626,-3.82946981909339));
#50862=CARTESIAN_POINT('Ctrl Pts',(374.824926215964,-13.7610997353743,-0.878291723523751));
#50863=CARTESIAN_POINT('Ctrl Pts',(373.735700028787,-13.9596158527859,2.87720922556887));
#50864=CARTESIAN_POINT('Ctrl Pts',(369.989443235373,-14.1581319701976,3.99781669620827));
#50865=CARTESIAN_POINT('Ctrl Pts',(367.016906545766,-14.3566480876092,1.45729968299728));
#50866=CARTESIAN_POINT('Ctrl Pts',(367.540282516669,-14.5551642050209,-2.4177846591233));
#50867=CARTESIAN_POINT('Ctrl Pts',(371.080273389593,-14.7536803224325,-4.07870780155963));
#50868=CARTESIAN_POINT('Ctrl Pts',(374.395022860881,-14.9521964398442,-2.00442792457674));
#50869=CARTESIAN_POINT('Ctrl Pts',(374.448946417949,-15.1507125572558,1.90546891747149));
#50870=CARTESIAN_POINT('Ctrl Pts',(371.192661892969,-15.3492286746675,4.07037357076146));
#50871=CARTESIAN_POINT('Ctrl Pts',(367.608212712817,-15.5477447920791,2.50770753466329));
#50872=CARTESIAN_POINT('Ctrl Pts',(366.978169253223,-15.7462609094908,-1.35146936002416));
#50873=CARTESIAN_POINT('Ctrl Pts',(369.879513329788,-15.9447770269025,-3.97299632247464));
#50874=CARTESIAN_POINT('Ctrl Pts',(373.655249226607,-16.1432931443141,-2.95612882720637));
#50875=CARTESIAN_POINT('Ctrl Pts',(374.847629831487,-16.3418092617258,0.767905216484709));
#50876=CARTESIAN_POINT('Ctrl Pts',(372.364695667963,-16.5403253791375,3.78870627002517));
#50877=CARTESIAN_POINT('Ctrl Pts',(368.480270612574,-16.7388414965491,3.33988219031162));
#50878=CARTESIAN_POINT('Ctrl Pts',(366.751637241445,-16.9373576139608,-0.167542467993559));
#50879=CARTESIAN_POINT('Ctrl Pts',(368.761845113765,-17.1358737313724,-3.52153492110588));
#50880=CARTESIAN_POINT('Ctrl Pts',(372.669984098268,-17.3343898487841,-3.65057268016657));
#50881=CARTESIAN_POINT('Ctrl Pts',(374.897054853636,-17.5329059661957,-0.436485419986235));
#50882=CARTESIAN_POINT('Ctrl Pts',(373.403548345479,-17.7314220836074,3.1773268849844));
#50883=CARTESIAN_POINT('Ctrl Pts',(369.557189424461,-17.929938201019,3.88140366785233));
#50884=CARTESIAN_POINT('Ctrl Pts',(366.880400424947,-18.1284543184307,1.03096480382756));
#50885=CARTESIAN_POINT('Ctrl Pts',(367.824533794764,-18.3269704358423,-2.76361201651236));
#50886=CARTESIAN_POINT('Ctrl Pts',(371.524970153157,-18.525486553254,-4.02732552160523));
#50887=CARTESIAN_POINT('Ctrl Pts',(374.592920272871,-18.7240026706656,-1.60289092186605));
#50888=CARTESIAN_POINT('Ctrl Pts',(374.218813792873,-18.9225187880773,2.28944069389871));
#50889=CARTESIAN_POINT('Ctrl Pts',(370.745250311282,-19.121034905489,4.08514607197289));
#50890=CARTESIAN_POINT('Ctrl Pts',(367.353253190361,-19.3195510229006,2.13975238504796));
#50891=CARTESIAN_POINT('Ctrl Pts',(367.149148870813,-19.5180671403123,-1.76518583368873));
#50892=CARTESIAN_POINT('Ctrl Pts',(370.319852206023,-19.7165832577239,-4.05360044334672));
#50893=CARTESIAN_POINT('Ctrl Pts',(373.961693394738,-19.9150993751356,-2.62980487460589));
#50894=CARTESIAN_POINT('Ctrl Pts',(374.739543551583,-20.1136154925472,1.20231597402637));
#50895=CARTESIAN_POINT('Ctrl Pts',(371.941062299023,-20.3121316099589,3.9333787242853));
#50896=CARTESIAN_POINT('Ctrl Pts',(368.129045535755,-20.5106477273706,3.0623280592983));
#50897=CARTESIAN_POINT('Ctrl Pts',(366.794465700587,-20.7091638447822,-0.613144390027927));
#50898=CARTESIAN_POINT('Ctrl Pts',(369.159505621711,-20.9076799621939,-3.72711087168108));
#50899=CARTESIAN_POINT('Ctrl Pts',(373.058306723985,-21.1061960796055,-3.42786011116434));
#50900=CARTESIAN_POINT('Ctrl Pts',(374.920421127656,-21.3047121970172,0.0105597280187822));
#50901=CARTESIAN_POINT('Ctrl Pts',(373.040559869231,-21.5032283144288,3.43930918226188));
#50902=CARTESIAN_POINT('Ctrl Pts',(369.140264158995,-21.7017444318405,3.71840468280298));
#50903=CARTESIAN_POINT('Ctrl Pts',(366.791350557657,-21.9002605492521,0.592255962748499));
#50904=CARTESIAN_POINT('Ctrl Pts',(368.144909583051,-22.0987766666638,-3.07626961892998));
#50905=CARTESIAN_POINT('Ctrl Pts',(371.961377372549,-22.2972927840755,-3.92760575820903));
#50906=CARTESIAN_POINT('Ctrl Pts',(374.74570584927,-22.4958089014871,-1.1821157573074));
#50907=CARTESIAN_POINT('Ctrl Pts',(373.948058863487,-22.6943250188988,2.6459344090777));
#50908=CARTESIAN_POINT('Ctrl Pts',(370.298908620604,-22.8928411363104,4.05088601609329));
#50909=CARTESIAN_POINT('Ctrl Pts',(367.140072795436,-23.0913572537221,1.74611774068392));
#50910=CARTESIAN_POINT('Ctrl Pts',(367.364362900362,-23.2898733711337,-2.15772122470869));
#50911=CARTESIAN_POINT('Ctrl Pts',(370.766358107745,-23.4883894885454,-4.08554090212426));
#50912=CARTESIAN_POINT('Ctrl Pts',(374.23061783122,-23.686905605957,-2.27193981372685));
#50913=CARTESIAN_POINT('Ctrl Pts',(374.584552021897,-23.8854217233687,1.62234321229351));
#50914=CARTESIAN_POINT('Ctrl Pts',(371.504214623111,-24.0839378407804,4.03074378626298));
#50915=CARTESIAN_POINT('Ctrl Pts',(367.810146555523,-24.282453958192,2.74822120765254));
#50916=CARTESIAN_POINT('Ctrl Pts',(366.8860793299,-24.4809700756037,-1.05180690007172));
#50917=CARTESIAN_POINT('Ctrl Pts',(369.576650354699,-24.6794861930153,-3.88708392786071));
#50918=CARTESIAN_POINT('Ctrl Pts',(373.421208137819,-24.878002310427,-3.16583478658316));
#50919=CARTESIAN_POINT('Ctrl Pts',(374.891985861526,-25.0765184278386,0.461098426636236));
#50920=CARTESIAN_POINT('Ctrl Pts',(373.401043479588,-25.2088625061131,2.58496980920822));
#50921=CARTESIAN_POINT('Ctrl Pts',(372.371206520492,-25.2750345452503,3.0961650259664));
#50922=CARTESIAN_POINT('Ctrl Pts',(372.700620528315,-0.00331660352971614,
-2.62002035518612));
#50923=CARTESIAN_POINT('Ctrl Pts',(373.572731978756,-0.0695344532319021,
-1.99886781016935));
#50924=CARTESIAN_POINT('Ctrl Pts',(374.631183474116,-0.201924342071306,
0.17304281508998));
#50925=CARTESIAN_POINT('Ctrl Pts',(372.74523325896,-0.40048627004793,3.28994261163778));
#50926=CARTESIAN_POINT('Ctrl Pts',(369.106321803303,-0.599002387459585,
3.38660851778649));
#50927=CARTESIAN_POINT('Ctrl Pts',(367.051463550486,-0.797518504871242,
0.385144897920928));
#50928=CARTESIAN_POINT('Ctrl Pts',(368.460100449493,-0.996034622282897,
-2.97058915076221));
#50929=CARTESIAN_POINT('Ctrl Pts',(372.043371921479,-1.19455073969455,-3.60516020055919));
#50930=CARTESIAN_POINT('Ctrl Pts',(374.519235483222,-1.39306685710621,-0.938557725399869));
#50931=CARTESIAN_POINT('Ctrl Pts',(373.620608004816,-1.59158297451786,2.5877334508211));
#50932=CARTESIAN_POINT('Ctrl Pts',(370.170307316614,-1.79009909192952,3.74414295853415));
#50933=CARTESIAN_POINT('Ctrl Pts',(367.328114955959,-1.98861520934117,1.47177837164182));
#50934=CARTESIAN_POINT('Ctrl Pts',(367.696826814086,-2.18713132675283,-2.14843253428664));
#50935=CARTESIAN_POINT('Ctrl Pts',(370.938797962963,-2.38564744416449,-3.80114029905533));
#50936=CARTESIAN_POINT('Ctrl Pts',(374.085085958097,-2.58416356157614,-1.9728406625985));
#50937=CARTESIAN_POINT('Ctrl Pts',(374.254383447452,-2.7826796789878,1.662151134065));
#50938=CARTESIAN_POINT('Ctrl Pts',(371.291649397126,-2.98119579639945,3.77497547420775));
#50939=CARTESIAN_POINT('Ctrl Pts',(367.910100071512,-3.17971191381111,2.43074959661624));
#50940=CARTESIAN_POINT('Ctrl Pts',(367.206493643716,-3.37822803122276,-1.13951077167314));
#50941=CARTESIAN_POINT('Ctrl Pts',(369.825179677376,-3.57674414863442,-3.66622873149492));
#50942=CARTESIAN_POINT('Ctrl Pts',(373.368015228213,-3.77526026604607,-2.83548421574951));
#50943=CARTESIAN_POINT('Ctrl Pts',(374.59053893278,-3.97377638345773,0.591942835967605));
#50944=CARTESIAN_POINT('Ctrl Pts',(372.373186816978,-4.17229250086939,3.47727988503472));
#50945=CARTESIAN_POINT('Ctrl Pts',(368.746567779752,-4.37080861828104,3.178190166736));
#50946=CARTESIAN_POINT('Ctrl Pts',(367.031870545056,-4.5693247356927,-0.031425653793909));
#50947=CARTESIAN_POINT('Ctrl Pts',(368.799382225706,-4.76784085310436,-3.21226245685293));
#50948=CARTESIAN_POINT('Ctrl Pts',(372.430449245098,-4.96635697051602,-3.45137040636336));
#50949=CARTESIAN_POINT('Ctrl Pts',(374.599809497624,-5.16487308792767,-0.529778989402399));
#50950=CARTESIAN_POINT('Ctrl Pts',(373.320804129371,-5.36338920533932,2.87697394841934));
#50951=CARTESIAN_POINT('Ctrl Pts',(369.764721927448,-5.56190532275099,3.64904887020751));
#50952=CARTESIAN_POINT('Ctrl Pts',(367.188155328459,-5.76042144016263,1.0793942488899));
#50953=CARTESIAN_POINT('Ctrl Pts',(367.950675012294,-5.95893755757429,-2.47874909328636));
#50954=CARTESIAN_POINT('Ctrl Pts',(371.353979957146,-6.15745367498596,-3.76690116664749));
#50955=CARTESIAN_POINT('Ctrl Pts',(374.281388232249,-6.35596979239761,-1.60539680564643));
#50956=CARTESIAN_POINT('Ctrl Pts',(374.052035024472,-6.55448590980927,2.02629941207819));
#50957=CARTESIAN_POINT('Ctrl Pts',(370.875957638737,-6.75300202722092,3.80234917252447));
#50958=CARTESIAN_POINT('Ctrl Pts',(367.661747329502,-6.95151814463257,2.09627988912292));
#50959=CARTESIAN_POINT('Ctrl Pts',(367.352916757201,-7.15003426204424,-1.52952264126551));
#50960=CARTESIAN_POINT('Ctrl Pts',(370.232287085369,-7.34855037945589,-3.75461743138875));
#50961=CARTESIAN_POINT('Ctrl Pts',(373.662985738898,-7.54706649686753,-2.54130499824269));
#50962=CARTESIAN_POINT('Ctrl Pts',(374.503244149697,-7.7455826142792,0.999286211547149));
#50963=CARTESIAN_POINT('Ctrl Pts',(371.983569648564,-7.94409873169085,3.62475011724142));
#50964=CARTESIAN_POINT('Ctrl Pts',(368.411432214348,-8.1426148491025,2.93073681562431));
#50965=CARTESIAN_POINT('Ctrl Pts',(367.058127360042,-8.34113096651416,-0.447189513216034));
#50966=CARTESIAN_POINT('Ctrl Pts',(369.162985928634,-8.53964708392582,-3.41558819229966));
#50967=CARTESIAN_POINT('Ctrl Pts',(372.798418481661,-8.73816320133748,-3.25605617625187));
#50968=CARTESIAN_POINT('Ctrl Pts',(374.635165040323,-8.93667931874914,-0.114689850748527));
#50969=CARTESIAN_POINT('Ctrl Pts',(372.991168044819,-9.13519543616079,3.13170725843804));
#50970=CARTESIAN_POINT('Ctrl Pts',(369.371968671495,-9.33371155357245,3.51014643173571));
#50971=CARTESIAN_POINT('Ctrl Pts',(367.091960861967,-9.5322276709841,0.674060272914903));
#50972=CARTESIAN_POINT('Ctrl Pts',(368.239132397856,-9.73074378839575,-2.77931746185542));
#50973=CARTESIAN_POINT('Ctrl Pts',(371.762925408109,-9.92925990580742,-3.68744913328253));
#50974=CARTESIAN_POINT('Ctrl Pts',(374.436317283588,-10.127776023219,-1.21868503116956));
#50975=CARTESIAN_POINT('Ctrl Pts',(373.811066598035,-10.3262921406307,2.36612764064113));
#50976=CARTESIAN_POINT('Ctrl Pts',(370.459766035749,-10.5248082580423,3.78408562767285));
#50977=CARTESIAN_POINT('Ctrl Pts',(367.451472903177,-10.723324375454,1.73664997782286));
#50978=CARTESIAN_POINT('Ctrl Pts',(367.541124827323,-10.9218404928657,-1.90117668713189));
#50979=CARTESIAN_POINT('Ctrl Pts',(370.646620281417,-11.1203566102773,-3.79794190622653));
#50980=CARTESIAN_POINT('Ctrl Pts',(373.924005601385,-11.318872727689,-2.21662417211437));
#50981=CARTESIAN_POINT('Ctrl Pts',(374.37191365368,-11.5173888451006,1.39463581415746));
#50982=CARTESIAN_POINT('Ctrl Pts',(371.580158764127,-11.7159049625123,3.72871485061005));
#50983=CARTESIAN_POINT('Ctrl Pts',(368.105376955766,-11.9144210799239,2.64810775455118));
#50984=CARTESIAN_POINT('Ctrl Pts',(367.129707311339,-12.1129371973356,-0.857586050774963));
#50985=CARTESIAN_POINT('Ctrl Pts',(369.546649532006,-12.3114533147473,-3.57791886381781));
#50986=CARTESIAN_POINT('Ctrl Pts',(373.142813907196,-12.5099694321589,-3.02166164060975));
#50987=CARTESIAN_POINT('Ctrl Pts',(374.62490150841,-12.7084855495706,0.301775834969675));
#50988=CARTESIAN_POINT('Ctrl Pts',(372.635644702753,-12.9070016669822,3.34885274126892));
#50989=CARTESIAN_POINT('Ctrl Pts',(368.996767033167,-13.1055177843939,3.32911400904782));
#50990=CARTESIAN_POINT('Ctrl Pts',(367.040683450667,-13.3040339018055,0.260635993803994));
#50991=CARTESIAN_POINT('Ctrl Pts',(368.558738091451,-13.5025500192172,-3.04652750674325));
#50992=CARTESIAN_POINT('Ctrl Pts',(372.16072539195,-13.7010661366288,-3.563739067713));
#50993=CARTESIAN_POINT('Ctrl Pts',(374.548013899432,-13.8995822540405,-0.817346179976291));
#50994=CARTESIAN_POINT('Ctrl Pts',(373.534370209785,-14.0980983714522,2.6775567918098));
#50995=CARTESIAN_POINT('Ctrl Pts',(370.048069932442,-14.2966144888638,3.72040418618724));
#50996=CARTESIAN_POINT('Ctrl Pts',(367.28180054493,-14.4951306062755,1.35617619644608));
#50997=CARTESIAN_POINT('Ctrl Pts',(367.76885893231,-14.6936467236871,-2.25001215679377));
#50998=CARTESIAN_POINT('Ctrl Pts',(371.063206288251,-14.8921628410988,-3.79568217661135));
#50999=CARTESIAN_POINT('Ctrl Pts',(374.147941969315,-15.0906789585104,-1.86533866061911));
#51000=CARTESIAN_POINT('Ctrl Pts',(374.198123716677,-15.2891950759221,1.77324651826443));
#51001=CARTESIAN_POINT('Ctrl Pts',(371.167796040662,-15.4877111933338,3.78792626644679));
#51002=CARTESIAN_POINT('Ctrl Pts',(367.83207538402,-15.6862273107454,2.33369519381498));
#51003=CARTESIAN_POINT('Ctrl Pts',(367.245751271968,-15.8847434281571,-1.25768954572296));
#51004=CARTESIAN_POINT('Ctrl Pts',(369.945768173257,-16.0832595455687,-3.69730612307973));
#51005=CARTESIAN_POINT('Ctrl Pts',(373.459501969453,-16.2817756629804,-2.75100008313996));
#51006=CARTESIAN_POINT('Ctrl Pts',(374.569142088304,-16.480291780392,0.71461950336905));
#51007=CARTESIAN_POINT('Ctrl Pts',(372.25850121656,-16.6788078978037,3.52580414219704));
#51008=CARTESIAN_POINT('Ctrl Pts',(368.643620311512,-16.8773240152153,3.10812441550726));
#51009=CARTESIAN_POINT('Ctrl Pts',(367.03493854368,-17.075840132627,-0.155916528108624));
#51010=CARTESIAN_POINT('Ctrl Pts',(368.90565607567,-17.2743562500386,-3.27717208112946));
#51011=CARTESIAN_POINT('Ctrl Pts',(372.542605376507,-17.4728723674503,-3.39725578067497));
#51012=CARTESIAN_POINT('Ctrl Pts',(374.615137458596,-17.671388484862,-0.406197258935498));
#51013=CARTESIAN_POINT('Ctrl Pts',(373.225266864901,-17.8699046022736,2.95684898584591));
#51014=CARTESIAN_POINT('Ctrl Pts',(369.645810646984,-18.0684207196853,3.61206917462133));
#51015=CARTESIAN_POINT('Ctrl Pts',(367.154766720739,-18.2669368370969,0.959425122119662));
#51016=CARTESIAN_POINT('Ctrl Pts',(368.033385729139,-18.4654529545086,-2.5718422070181));
#51017=CARTESIAN_POINT('Ctrl Pts',(371.477045097399,-18.6639690719202,-3.74786536459506));
#51018=CARTESIAN_POINT('Ctrl Pts',(374.332107081412,-18.8624851893319,-1.49166471323407));
#51019=CARTESIAN_POINT('Ctrl Pts',(373.983960225258,-19.0610013067436,2.13057410803424));
#51020=CARTESIAN_POINT('Ctrl Pts',(370.751430797345,-19.2595174241552,3.80167368898359));
#51021=CARTESIAN_POINT('Ctrl Pts',(367.59480775853,-19.4580335415669,1.99127282105928));
#51022=CARTESIAN_POINT('Ctrl Pts',(367.404866442415,-19.6565496589785,-1.6426978183574));
#51023=CARTESIAN_POINT('Ctrl Pts',(370.355551493247,-19.8550657763902,-3.7723170431654));
#51024=CARTESIAN_POINT('Ctrl Pts',(373.744681669421,-20.0535818938018,-2.44732007688568));
#51025=CARTESIAN_POINT('Ctrl Pts',(374.468556023763,-20.2520980112135,1.11888606276775));
#51026=CARTESIAN_POINT('Ctrl Pts',(371.864264191958,-20.4506141286251,3.66043762976184));
#51027=CARTESIAN_POINT('Ctrl Pts',(368.316767095023,-20.6491302460368,2.84983004400823));
#51028=CARTESIAN_POINT('Ctrl Pts',(367.074795093088,-20.8476463634485,-0.570597685872091));
#51029=CARTESIAN_POINT('Ctrl Pts',(369.275722522151,-21.0461624808601,-3.468482910319));
#51030=CARTESIAN_POINT('Ctrl Pts',(372.903981905771,-21.2446785982718,-3.18999746019762));
#51031=CARTESIAN_POINT('Ctrl Pts',(374.636882323428,-21.4431947156834,0.0098269779010755));
#51032=CARTESIAN_POINT('Ctrl Pts',(372.887466523066,-21.6417108330951,3.20065206876929));
#51033=CARTESIAN_POINT('Ctrl Pts',(369.25781624383,-21.8402269505067,3.46038085261869));
#51034=CARTESIAN_POINT('Ctrl Pts',(367.071896113049,-22.0387430679184,0.551158727510847));
#51035=CARTESIAN_POINT('Ctrl Pts',(368.331530320168,-22.23725918533,-2.86280418483489));
#51036=CARTESIAN_POINT('Ctrl Pts',(371.883169582157,-22.4357753027417,-3.65506525559138));
#51037=CARTESIAN_POINT('Ctrl Pts',(374.474290713434,-22.6342914201533,-1.10008755934594));
#51038=CARTESIAN_POINT('Ctrl Pts',(373.731993251966,-22.832807537565,2.46233036678399));
#51039=CARTESIAN_POINT('Ctrl Pts',(370.336061204226,-23.0313236549767,3.76979097274141));
#51040=CARTESIAN_POINT('Ctrl Pts',(367.396420165011,-23.2298397723883,1.62495287944981));
#51041=CARTESIAN_POINT('Ctrl Pts',(367.605146554612,-23.4283558898,-2.00799478491476));
#51042=CARTESIAN_POINT('Ctrl Pts',(370.771073902642,-23.6268720072116,-3.80204112147478));
#51043=CARTESIAN_POINT('Ctrl Pts',(373.994945169546,-23.8253881246233,-2.11428763148934));
#51044=CARTESIAN_POINT('Ctrl Pts',(374.324319511765,-24.0239042420349,1.50976718971982));
#51045=CARTESIAN_POINT('Ctrl Pts',(371.457729814399,-24.2224203594466,3.75104643243998));
#51046=CARTESIAN_POINT('Ctrl Pts',(368.019996834858,-24.4209364768583,2.5575193818207));
#51047=CARTESIAN_POINT('Ctrl Pts',(367.160051560781,-24.6194525942699,-0.978820964402642));
#51048=CARTESIAN_POINT('Ctrl Pts',(369.663921163755,-24.8179687116816,-3.61735527569092));
#51049=CARTESIAN_POINT('Ctrl Pts',(373.24170122654,-25.0164848290932,-2.9461543356783));
#51050=CARTESIAN_POINT('Ctrl Pts',(374.610420208933,-25.2150009465049,0.429102344369353));
#51051=CARTESIAN_POINT('Ctrl Pts',(373.222935814167,-25.3473450247793,2.40559616164177));
#51052=CARTESIAN_POINT('Ctrl Pts',(372.264560274501,-25.4135170639165,2.88131902962364));
#51053=CARTESIAN_POINT('',(372.708327421072,-25.0015807238107,-2.6251510527254));
#51054=CARTESIAN_POINT('Ctrl Pts',(372.710055492832,-25.,-2.62730824261312));
#51055=CARTESIAN_POINT('Ctrl Pts',(372.771968511579,-25.,-2.59284592995977));
#51056=CARTESIAN_POINT('Ctrl Pts',(372.832531621219,-25.,-2.5562762099857));
#51057=CARTESIAN_POINT('Ctrl Pts',(372.891624715321,-25.,-2.5176286591942));
#51058=CARTESIAN_POINT('Ctrl Pts',(372.976881734171,-25.,-2.46186960618737));
#51059=CARTESIAN_POINT('Ctrl Pts',(373.059080109873,-24.9999999999999,-2.40178808048538));
#51060=CARTESIAN_POINT('Ctrl Pts',(373.138140178334,-24.9999999999999,-2.33778533264371));
#51061=CARTESIAN_POINT('Ctrl Pts',(373.219143227778,-24.9999999999998,-2.27220965267224));
#51062=CARTESIAN_POINT('Ctrl Pts',(373.29685231911,-25.0000000000001,-2.2025172742355));
#51063=CARTESIAN_POINT('Ctrl Pts',(373.371162264727,-25.0000000000001,-2.12908846814534));
#51064=CARTESIAN_POINT('Ctrl Pts',(373.446906619678,-25.,-2.05424226141092));
#51065=CARTESIAN_POINT('Ctrl Pts',(373.519119902956,-24.9999999999998,-1.97551347585753));
#51066=CARTESIAN_POINT('Ctrl Pts',(373.587662531599,-24.9999999999999,-1.89325900534171));
#51067=CARTESIAN_POINT('Ctrl Pts',(373.609387670299,-24.9999999999999,-1.86718778782262));
#51068=CARTESIAN_POINT('Ctrl Pts',(373.630743801882,-24.9999999999998,-1.84076206399809));
#51069=CARTESIAN_POINT('Ctrl Pts',(373.651725760841,-24.9999999999999,-1.81399239721465));
#51070=CARTESIAN_POINT('Ctrl Pts',(373.661651039041,-24.9999999999999,-1.80132930933652));
#51071=CARTESIAN_POINT('Ctrl Pts',(373.671492887642,-25.,-1.78858874746849));
#51072=CARTESIAN_POINT('Ctrl Pts',(373.681241296488,-25.,-1.77578452013048));
#51073=CARTESIAN_POINT('Ctrl Pts',(373.747047602416,-24.9999999999999,-1.68935001428228));
#51074=CARTESIAN_POINT('Ctrl Pts',(373.808704481108,-24.9999999999999,-1.59988381928839));
#51075=CARTESIAN_POINT('Ctrl Pts',(373.866116865864,-24.9999999999999,-1.50781218801566));
#51076=CARTESIAN_POINT('Ctrl Pts',(373.925146451428,-24.9999999999999,-1.41314706899431));
#51077=CARTESIAN_POINT('Ctrl Pts',(373.979689680909,-25.0000000000001,-1.31572714412399));
#51078=CARTESIAN_POINT('Ctrl Pts',(374.029613735414,-24.9999999999999,-1.21596807661173));
#51079=CARTESIAN_POINT('Ctrl Pts',(374.079537789919,-24.9999999999998,-1.11620900909947));
#51080=CARTESIAN_POINT('Ctrl Pts',(374.124843192826,-24.9999999999998,-1.01411001628537));
#51081=CARTESIAN_POINT('Ctrl Pts',(374.165359541272,-24.9999999999999,-0.910050010489073));
#51082=CARTESIAN_POINT('Ctrl Pts',(374.185738924586,-25.,-0.857708700695329));
#51083=CARTESIAN_POINT('Ctrl Pts',(374.204906033823,-24.9999999999999,-0.804870747703794));
#51084=CARTESIAN_POINT('Ctrl Pts',(374.222834941311,-25.,-0.751581820778674));
#51085=CARTESIAN_POINT('Ctrl Pts',(374.235982960149,-25.,-0.712502818585623));
#51086=CARTESIAN_POINT('Ctrl Pts',(374.248465026867,-25.,-0.673181252231886));
#51087=CARTESIAN_POINT('Ctrl Pts',(374.260269835228,-25.,-0.633634711670137));
#51088=CARTESIAN_POINT('Ctrl Pts',(374.264737309274,-25.,-0.618668509920597));
#51089=CARTESIAN_POINT('Ctrl Pts',(374.269107112265,-24.9999999999997,-0.603672133656458));
#51090=CARTESIAN_POINT('Ctrl Pts',(374.273375702996,-24.9999999999997,-0.588657555605075));
#51091=CARTESIAN_POINT('Ctrl Pts',(374.304873007746,-24.9999999999999,-0.477867186990406));
#51092=CARTESIAN_POINT('Ctrl Pts',(374.330912502926,-24.9999999999999,-0.365923379558715));
#51093=CARTESIAN_POINT('Ctrl Pts',(374.351360867503,-25.,-0.253257538102531));
#51094=CARTESIAN_POINT('Ctrl Pts',(374.37166317464,-25.0000000000001,-0.141396439953867));
#51095=CARTESIAN_POINT('Ctrl Pts',(374.386454396591,-25.0000000000001,-0.0288227255026901));
#51096=CARTESIAN_POINT('Ctrl Pts',(374.395562613578,-25.,0.0840708268164784));
#51097=CARTESIAN_POINT('Ctrl Pts',(374.404110100215,-24.9999999999998,0.190014298653879));
#51098=CARTESIAN_POINT('Ctrl Pts',(374.407652758268,-25.,0.296240255371398));
#51099=CARTESIAN_POINT('Ctrl Pts',(374.406009408055,-25.,0.402437878630536));
#51100=CARTESIAN_POINT('Ctrl Pts',(374.404804761328,-25.,0.480285326001078));
#51101=CARTESIAN_POINT('Ctrl Pts',(374.400812596699,-25.0000000000001,0.558117856392796));
#51102=CARTESIAN_POINT('Ctrl Pts',(374.394107752198,-24.9999999999999,0.635838004036831));
#51103=CARTESIAN_POINT('Ctrl Pts',(374.392177972379,-24.9999999999998,0.658207318113189));
#51104=CARTESIAN_POINT('Ctrl Pts',(374.390023396068,-24.9999999999998,0.680567323639902));
#51105=CARTESIAN_POINT('Ctrl Pts',(374.387645617996,-24.9999999999999,0.702915693478943));
#51106=CARTESIAN_POINT('Ctrl Pts',(374.385303056528,-24.9999999999999,0.724933067883653));
#51107=CARTESIAN_POINT('Ctrl Pts',(374.382743137976,-24.9999999999998,0.746944033946365));
#51108=CARTESIAN_POINT('Ctrl Pts',(374.379971408169,-24.9999999999998,0.768916275062687));
#51109=CARTESIAN_POINT('Ctrl Pts',(374.365851915879,-24.9999999999999,0.880845254649348));
#51110=CARTESIAN_POINT('Ctrl Pts',(374.34622863719,-25.,0.991901140183087));
#51111=CARTESIAN_POINT('Ctrl Pts',(374.321418324306,-24.9999999999999,1.10178546480141));
#51112=CARTESIAN_POINT('Ctrl Pts',(374.296608011421,-24.9999999999998,1.21166978941972));
#51113=CARTESIAN_POINT('Ctrl Pts',(374.266610392464,-24.9999999999999,1.32038318853165));
#51114=CARTESIAN_POINT('Ctrl Pts',(374.231690381868,-25.,1.42763565289335));
#51115=CARTESIAN_POINT('Ctrl Pts',(374.195470399576,-25.0000000000001,1.53888081845062));
#51116=CARTESIAN_POINT('Ctrl Pts',(374.153954726584,-24.9999999999999,1.64855499433829));
#51117=CARTESIAN_POINT('Ctrl Pts',(374.10738473957,-25.,1.75633314173944));
#51118=CARTESIAN_POINT('Ctrl Pts',(374.068369693084,-25.0000000000001,1.84662669130948));
#51119=CARTESIAN_POINT('Ctrl Pts',(374.025806152196,-24.9999999999998,1.93558970495143));
#51120=CARTESIAN_POINT('Ctrl Pts',(373.979808694952,-24.9999999999999,2.02302429509298));
#51121=CARTESIAN_POINT('Ctrl Pts',(373.969803663349,-25.,2.04204242979044));
#51122=CARTESIAN_POINT('Ctrl Pts',(373.959636078221,-25.0000000000001,2.06098821706984));
#51123=CARTESIAN_POINT('Ctrl Pts',(373.949306972949,-24.9999999999999,2.07985955613166));
#51124=CARTESIAN_POINT('Ctrl Pts',(373.940126387568,-24.9999999999998,2.09663254226612));
#51125=CARTESIAN_POINT('Ctrl Pts',(373.930822447483,-24.9999999999999,2.1133389108301));
#51126=CARTESIAN_POINT('Ctrl Pts',(373.921398780686,-24.9999999999999,2.12997293009874));
#51127=CARTESIAN_POINT('Ctrl Pts',(373.861778008854,-24.9999999999999,2.23521148413278));
#51128=CARTESIAN_POINT('Ctrl Pts',(373.797338418164,-24.9999999999999,2.33761108513235));
#51129=CARTESIAN_POINT('Ctrl Pts',(373.728358005558,-25.,2.43683199938061));
#51130=CARTESIAN_POINT('Ctrl Pts',(373.659461266479,-25.0000000000001,2.53593255824786));
#51131=CARTESIAN_POINT('Ctrl Pts',(373.58603433585,-25.,2.63186294750434));
#51132=CARTESIAN_POINT('Ctrl Pts',(373.508304284397,-25.,2.7242704384121));
#51133=CARTESIAN_POINT('Ctrl Pts',(373.473163357405,-24.9999999999999,2.76604687919357));
#51134=CARTESIAN_POINT('Ctrl Pts',(373.437142295832,-24.9999999999999,2.80710302614759));
#51135=CARTESIAN_POINT('Ctrl Pts',(373.400259044447,-25.,2.84740464341324));
#51136=CARTESIAN_POINT('Ctrl Pts',(373.379017824292,-25.,2.87061451490727));
#51137=CARTESIAN_POINT('Ctrl Pts',(373.357485587894,-24.9999999999999,2.89357914795995));
#51138=CARTESIAN_POINT('Ctrl Pts',(373.33569211506,-24.9999999999999,2.91626468202821));
#51139=CARTESIAN_POINT('Ctrl Pts',(373.250223696163,-24.9999999999999,3.00523153661808));
#51140=CARTESIAN_POINT('Ctrl Pts',(373.160687141109,-24.9999999999999,3.08997040744572));
#51141=CARTESIAN_POINT('Ctrl Pts',(373.067337084626,-25.,3.17012486440459));
#51142=CARTESIAN_POINT('Ctrl Pts',(372.975213103972,-25.,3.24922655882652));
#51143=CARTESIAN_POINT('Ctrl Pts',(372.879374657813,-24.9999999999999,3.32386422800678));
#51144=CARTESIAN_POINT('Ctrl Pts',(372.780023847006,-24.9999999999999,3.39366907551449));
#51145=CARTESIAN_POINT('Ctrl Pts',(372.715806208875,-25.,3.43878901364673));
#51146=CARTESIAN_POINT('Ctrl Pts',(372.650120270092,-25.,3.48188925341228));
#51147=CARTESIAN_POINT('Ctrl Pts',(372.583012328556,-25.,3.52286199445037));
#51148=CARTESIAN_POINT('Ctrl Pts',(372.667675165437,-25.,-2.65045628680304));
#51149=CARTESIAN_POINT('Ctrl Pts',(372.680776617905,-25.0005269079369,-2.6413938307266));
#51150=CARTESIAN_POINT('Ctrl Pts',(372.693810874283,-25.0010538158738,-2.63223423032627));
#51151=CARTESIAN_POINT('Ctrl Pts',(372.706776501453,-25.0015807238107,-2.62297849270138));
#51152=CARTESIAN_POINT('Ctrl Pts',(372.587298607636,-5.39100014629312E-14,
3.52813099626156));
#51153=CARTESIAN_POINT('Ctrl Pts',(372.660631342051,-1.32574515254873E-13,
3.48377173581607));
#51154=CARTESIAN_POINT('Ctrl Pts',(372.732262094389,8.46232978098733E-15,
3.43693152907772));
#51155=CARTESIAN_POINT('Ctrl Pts',(372.802052682076,3.00003077935429E-14,
3.38761100392567));
#51156=CARTESIAN_POINT('Ctrl Pts',(372.900596037527,5.99499074761691E-14,
3.31797109685311));
#51157=CARTESIAN_POINT('Ctrl Pts',(372.995472482377,7.01230023383802E-14,
3.24338764266986));
#51158=CARTESIAN_POINT('Ctrl Pts',(373.086525205177,-1.39194211712379E-14,
3.16427958978847));
#51159=CARTESIAN_POINT('Ctrl Pts',(373.177577927977,-9.7961844680856E-14,
3.08517153690708));
#51160=CARTESIAN_POINT('Ctrl Pts',(373.264807269228,4.54506319836866E-15,
3.00153800855235));
#51161=CARTESIAN_POINT('Ctrl Pts',(373.348015410421,6.32341401463066E-14,
2.91376566625183));
#51162=CARTESIAN_POINT('Ctrl Pts',(373.434550766167,1.24185787802521E-13,
2.82248360230161));
#51163=CARTESIAN_POINT('Ctrl Pts',(373.516737634603,-8.04236111962304E-15,
2.72672427203484));
#51164=CARTESIAN_POINT('Ctrl Pts',(373.594300525691,6.13259443227321E-14,
2.62690061959373));
#51165=CARTESIAN_POINT('Ctrl Pts',(373.616831523276,8.1423522838862E-14,
2.59790316423139));
#51166=CARTESIAN_POINT('Ctrl Pts',(373.638971968167,-1.88987798754606E-13,
2.56856266068163));
#51167=CARTESIAN_POINT('Ctrl Pts',(373.660714176623,-9.96563942479156E-14,
2.53888906690075));
#51168=CARTESIAN_POINT('Ctrl Pts',(373.673173508902,-4.83195549220742E-14,
2.52188466895384));
#51169=CARTESIAN_POINT('Ctrl Pts',(373.685503930738,6.89077272075961E-14,
2.50476810129091));
#51170=CARTESIAN_POINT('Ctrl Pts',(373.697689357101,4.89330798103538E-14,
2.48756224517728));
#51171=CARTESIAN_POINT('Ctrl Pts',(373.766942548858,-6.44251217543604E-14,
2.38977654467579));
#51172=CARTESIAN_POINT('Ctrl Pts',(373.831613708245,-7.49003207069224E-15,
2.28897898450612));
#51173=CARTESIAN_POINT('Ctrl Pts',(373.891539616009,2.38559172416331E-14,
2.18556270252441));
#51174=CARTESIAN_POINT('Ctrl Pts',(373.951341035714,5.52268502057201E-14,
2.0823612540371));
#51175=CARTESIAN_POINT('Ctrl Pts',(374.006417194121,-1.68658709948127E-13,
1.97655106277686));
#51176=CARTESIAN_POINT('Ctrl Pts',(374.056558100354,-1.69197988952874E-13,
1.86850329695167));
#51177=CARTESIAN_POINT('Ctrl Pts',(374.105966497165,-1.69494372126335E-13,
1.76203400292719));
#51178=CARTESIAN_POINT('Ctrl Pts',(374.15058295894,-8.058753574167E-14,
1.65339120735355));
#51179=CARTESIAN_POINT('Ctrl Pts',(374.190156812769,2.93653990013354E-14,
1.54292382115721));
#51180=CARTESIAN_POINT('Ctrl Pts',(374.209951262687,8.41462754648355E-14,
1.48766912816844));
#51181=CARTESIAN_POINT('Ctrl Pts',(374.228483302472,2.62490338558534E-14,
1.43195791926079));
#51182=CARTESIAN_POINT('Ctrl Pts',(374.245716578873,-2.16493489801906E-15,
1.37583422589407));
#51183=CARTESIAN_POINT('Ctrl Pts',(374.255406439774,-1.82167105339991E-14,
1.34427720972637));
#51184=CARTESIAN_POINT('Ctrl Pts',(374.26468562941,9.69296388603166E-14,
1.31258979319956));
#51185=CARTESIAN_POINT('Ctrl Pts',(374.273547201858,1.28952404310212E-13,
1.28077989713641));
#51186=CARTESIAN_POINT('Ctrl Pts',(374.279394300744,1.49776578270487E-13,
1.25979088994735));
#51187=CARTESIAN_POINT('Ctrl Pts',(374.285059574122,-3.35614282714963E-14,
1.23874856025971));
#51188=CARTESIAN_POINT('Ctrl Pts',(374.290540941591,7.76601005725297E-14,
1.21765520506871));
#51189=CARTESIAN_POINT('Ctrl Pts',(374.294235079404,1.52743960408112E-13,
1.20343945298671));
#51190=CARTESIAN_POINT('Ctrl Pts',(374.297844985085,5.19606561357509E-14,
1.18920308752562));
#51191=CARTESIAN_POINT('Ctrl Pts',(374.301368160791,4.47697434680094E-14,
1.17495508353966));
#51192=CARTESIAN_POINT('Ctrl Pts',(374.328925788284,-1.24175715681814E-14,
1.06350983666338));
#51193=CARTESIAN_POINT('Ctrl Pts',(374.351219759732,1.10643004235819E-13,
0.951206367372526));
#51194=CARTESIAN_POINT('Ctrl Pts',(374.368060150219,1.57318602589385E-13,
0.838381918102844));
#51195=CARTESIAN_POINT('Ctrl Pts',(374.384682963229,2.03446625873874E-13,
0.727015158252954));
#51196=CARTESIAN_POINT('Ctrl Pts',(374.395992332712,-5.01658879784927E-14,
0.615140046817444));
#51197=CARTESIAN_POINT('Ctrl Pts',(374.401754922618,-6.86395384974503E-14,
0.503081915528177));
#51198=CARTESIAN_POINT('Ctrl Pts',(374.407517512524,-8.69669429602971E-14,
0.391023784238904));
#51199=CARTESIAN_POINT('Ctrl Pts',(374.407733555706,-1.17552468830718E-13,
0.278781917773848));
#51200=CARTESIAN_POINT('Ctrl Pts',(374.402115858007,-1.03805852802452E-14,
0.166693540191318));
#51201=CARTESIAN_POINT('Ctrl Pts',(374.398588581057,5.67276483668388E-14,
0.0963147530500085));
#51202=CARTESIAN_POINT('Ctrl Pts',(374.39276008294,1.39712369924032E-13,
0.0259967490998595));
#51203=CARTESIAN_POINT('Ctrl Pts',(374.384671128337,-8.08242361927114E-14,
-0.0441708552043921));
#51204=CARTESIAN_POINT('Ctrl Pts',(374.381825479191,-1.58284413966769E-13,
-0.0688554273247632));
#51205=CARTESIAN_POINT('Ctrl Pts',(374.378700021911,-2.6431705795843E-14,
-0.0935213491463014));
#51206=CARTESIAN_POINT('Ctrl Pts',(374.375296356418,7.01105840050786E-14,
-0.118164589998438));
#51207=CARTESIAN_POINT('Ctrl Pts',(374.372928259175,1.3693355931467E-13,
-0.135310102927504));
#51208=CARTESIAN_POINT('Ctrl Pts',(374.370425488713,-4.5796502390556E-14,
-0.152444635294189));
#51209=CARTESIAN_POINT('Ctrl Pts',(374.367788559528,-8.68471961013029E-14,
-0.169566808095477));
#51210=CARTESIAN_POINT('Ctrl Pts',(374.365362539547,-1.24705269334985E-13,
-0.185319500110263));
#51211=CARTESIAN_POINT('Ctrl Pts',(374.362824551415,-1.30601033380312E-13,
-0.201051410598341));
#51212=CARTESIAN_POINT('Ctrl Pts',(374.360175473219,-1.28230759344206E-13,
-0.216761238893641));
#51213=CARTESIAN_POINT('Ctrl Pts',(374.341794196345,-1.13023381999282E-13,
-0.325767724235194));
#51214=CARTESIAN_POINT('Ctrl Pts',(374.318067628613,1.32714687406766E-14,
-0.433718032245795));
#51215=CARTESIAN_POINT('Ctrl Pts',(374.289240099998,-3.88578058618805E-16,
-0.540294095901434));
#51216=CARTESIAN_POINT('Ctrl Pts',(374.259930978086,-1.48504455298718E-14,
-0.648650621509259));
#51217=CARTESIAN_POINT('Ctrl Pts',(374.225348585167,-2.11349790313351E-14,
-0.755587420359765));
#51218=CARTESIAN_POINT('Ctrl Pts',(374.185700725717,7.91033905045424E-14,
-0.86074915159152));
#51219=CARTESIAN_POINT('Ctrl Pts',(374.146387566555,1.78495565273169E-13,
-0.965023125898503));
#51220=CARTESIAN_POINT('Ctrl Pts',(374.102093485652,1.83869541908598E-13,
-1.06755256877881));
#51221=CARTESIAN_POINT('Ctrl Pts',(374.052981651546,-2.38697950294409E-15,
-1.16795933088895));
#51222=CARTESIAN_POINT('Ctrl Pts',(374.016144412419,-1.42166948976216E-13,
-1.24327127908106));
#51223=CARTESIAN_POINT('Ctrl Pts',(373.976595839122,1.28712068496929E-13,
-1.31738841806524));
#51224=CARTESIAN_POINT('Ctrl Pts',(373.934393111636,1.64535052249448E-13,
-1.39013578508038));
#51225=CARTESIAN_POINT('Ctrl Pts',(373.921423669026,1.75436459773538E-13,
-1.41249198947007));
#51226=CARTESIAN_POINT('Ctrl Pts',(373.908200121078,2.23317344162524E-13,
-1.43472404744811));
#51227=CARTESIAN_POINT('Ctrl Pts',(373.894742428895,1.59205981731247E-13,
-1.45679698291906));
#51228=CARTESIAN_POINT('Ctrl Pts',(373.837459225495,-1.12167093464855E-13,
-1.55075131290849));
#51229=CARTESIAN_POINT('Ctrl Pts',(373.775890342919,1.17621846843771E-13,
-1.64191037580254));
#51230=CARTESIAN_POINT('Ctrl Pts',(373.710216618943,1.41386902186014E-13,
-1.72992114994153));
#51231=CARTESIAN_POINT('Ctrl Pts',(373.642632073462,1.66117424912312E-13,
-1.82049265719666));
#51232=CARTESIAN_POINT('Ctrl Pts',(373.570699887383,1.05988939062973E-13,
-1.90773099559844));
#51233=CARTESIAN_POINT('Ctrl Pts',(373.494582358701,3.09197112358106E-14,
-1.99120405364651));
#51234=CARTESIAN_POINT('Ctrl Pts',(373.460202923462,-3.19607888373383E-15,
-2.02890570585487));
#51235=CARTESIAN_POINT('Ctrl Pts',(373.42496926309,-5.5061817914234E-15,
-2.06583852260486));
#51236=CARTESIAN_POINT('Ctrl Pts',(373.388894504457,7.68274333040608E-14,
-2.10195881889829));
#51237=CARTESIAN_POINT('Ctrl Pts',(373.376991319632,1.04065623732737E-13,
-2.11387702927611));
#51238=CARTESIAN_POINT('Ctrl Pts',(373.364997241332,-6.20600606500304E-14,
-2.12570599707654));
#51239=CARTESIAN_POINT('Ctrl Pts',(373.352920060586,-3.73034936274053E-14,
-2.13743723583697));
#51240=CARTESIAN_POINT('Ctrl Pts',(373.277094993757,1.16986319815685E-13,
-2.21109034923226));
#51241=CARTESIAN_POINT('Ctrl Pts',(373.197920576716,-7.37054647652644E-14,
-2.28097113257338));
#51242=CARTESIAN_POINT('Ctrl Pts',(373.115542316673,-3.1641356201817E-15,
-2.34673402124385));
#51243=CARTESIAN_POINT('Ctrl Pts',(373.035424405369,6.55000650524509E-14,
-2.41069246463416));
#51244=CARTESIAN_POINT('Ctrl Pts',(372.952275508019,1.89627060006236E-13,
-2.47075621159766));
#51245=CARTESIAN_POINT('Ctrl Pts',(372.866210014442,7.55506768257419E-14,
-2.52656264484576));
#51246=CARTESIAN_POINT('Ctrl Pts',(372.813846980641,5.84722174892913E-15,
-2.56051578946911));
#51247=CARTESIAN_POINT('Ctrl Pts',(372.76040399165,1.33441461253479E-13,
-2.59289214810169));
#51248=CARTESIAN_POINT('Ctrl Pts',(372.705904384963,4.44089209850063E-15,
-2.62360084935057));
#51249=CARTESIAN_POINT('Origin',(370.834317853224,-25.,0.));
#51250=CARTESIAN_POINT('Origin',(370.834317853224,0.,0.));
#51251=CARTESIAN_POINT('',(0.,0.,0.));
#51252=CARTESIAN_POINT('Origin',(376.324799934857,-11.9861373773513,-27.0570908269895));
#51253=CARTESIAN_POINT('',(339.771799934857,-10.9861373773513,-29.8855179517357));
#51254=CARTESIAN_POINT('',(339.771799934857,-8.98613737735134,-27.0570908269895));
#51255=CARTESIAN_POINT('Origin',(339.771799934857,-11.9861373773513,-27.0570908269895));
#51256=CARTESIAN_POINT('',(380.681799934857,-8.98613737735134,-27.0570908269895));
#51257=CARTESIAN_POINT('',(376.324799934857,-8.98613737735134,-27.0570908269895));
#51258=CARTESIAN_POINT('',(380.681799934857,-10.9861373773513,-29.8855179517357));
#51259=CARTESIAN_POINT('Origin',(380.681799934857,-11.9861373773513,-27.0570908269895));
#51260=CARTESIAN_POINT('',(380.681635380396,-10.9861373773513,-29.8855179517357));
#51261=CARTESIAN_POINT('',(376.324799934857,-10.9861373773513,-29.8855179517357));
#51262=CARTESIAN_POINT('',(380.681635380396,-11.9861373773513,-30.0570908269895));
#51263=CARTESIAN_POINT('Origin',(380.681635380396,-11.9861373773513,-27.0570908269895));
#51264=CARTESIAN_POINT('',(339.720861706803,-11.9861373773513,-30.0570908269895));
#51265=CARTESIAN_POINT('',(376.324799934857,-11.9861373773513,-30.0570908269895));
#51266=CARTESIAN_POINT('Ctrl Pts',(339.720861706803,-11.9861373773513,-30.0570908269895));
#51267=CARTESIAN_POINT('Ctrl Pts',(339.753951191729,-11.6599132580678,-30.0570908269895));
#51268=CARTESIAN_POINT('Ctrl Pts',(339.771447804716,-11.3135279162041,-30.0012679867952));
#51269=CARTESIAN_POINT('Ctrl Pts',(339.771447804716,-10.9861373773513,-29.8855179517357));
#51270=CARTESIAN_POINT('Origin',(380.681635380396,-15.0708658676184,-30.0570908269895));
#51271=CARTESIAN_POINT('',(380.681635380396,-10.9861373773513,-27.5570908269895));
#51272=CARTESIAN_POINT('',(380.681635380396,-10.9861373773513,-30.0570908269895));
#51273=CARTESIAN_POINT('',(380.681635380396,-11.4861373773513,-28.0570908269895));
#51274=CARTESIAN_POINT('Origin',(380.681635380396,-11.4861373773513,-27.5570908269895));
#51275=CARTESIAN_POINT('',(380.681635380396,-15.0708658676184,-28.0570908269895));
#51276=CARTESIAN_POINT('',(380.681635380396,-15.0708658676184,-28.0570908269895));
#51277=CARTESIAN_POINT('',(380.681635380396,-15.0708658676184,-30.0570908269895));
#51278=CARTESIAN_POINT('',(380.681635380396,-15.0708658676184,-30.0570908269895));
#51279=CARTESIAN_POINT('',(380.681635380396,-15.0708658676184,-30.0570908269895));
#51280=CARTESIAN_POINT('Origin',(330.604799934857,-10.9861373773513,-30.0570908269895));
#51281=CARTESIAN_POINT('',(380.681799934857,-10.9861373773513,0.820909173010471));
#51282=CARTESIAN_POINT('',(380.681799934857,-10.9861373773513,-30.0570908269895));
#51283=CARTESIAN_POINT('',(371.681799934857,-10.9861373773513,9.82090917301047));
#51284=CARTESIAN_POINT('Origin',(371.681799934857,-10.9861373773512,0.820909173010471));
#51285=CARTESIAN_POINT('',(370.321612719089,-10.9861373773513,9.82090917301047));
#51286=CARTESIAN_POINT('',(391.564799934857,-10.9861373773513,9.82090917301047));
#51287=CARTESIAN_POINT('',(361.330051062071,-10.9861373773513,1.21054870903725));
#51288=CARTESIAN_POINT('Origin',(370.321612719089,-10.9861373773513,0.820909173010471));
#51289=CARTESIAN_POINT('',(342.448997804234,-10.9861373773513,-21.7410591318785));
#51290=CARTESIAN_POINT('Origin',(336.6390287719,-10.9861373773513,2.28050728087887));
#51291=CARTESIAN_POINT('',(339.771799934857,-10.9861373773513,-25.1429698676036));
#51292=CARTESIAN_POINT('Origin',(343.271799934857,-10.9861373773513,-25.1429698676036));
#51293=CARTESIAN_POINT('',(339.771799934857,-10.9861373773513,-27.5570908269895));
#51294=CARTESIAN_POINT('',(339.771799934857,-10.9861373773513,-30.0570908269895));
#51295=CARTESIAN_POINT('',(345.844799934857,-10.9861373773513,-27.5570908269895));
#51296=CARTESIAN_POINT('',(366.389317853224,-10.9861373773513,0.));
#51297=CARTESIAN_POINT('Origin',(370.834317853224,-10.9861373773513,0.));
#51298=CARTESIAN_POINT('Origin',(380.681799934857,-10.9861373773514,-30.0570908269895));
#51299=CARTESIAN_POINT('',(380.681799934857,-8.98613737735134,0.820909173010471));
#51300=CARTESIAN_POINT('',(380.681799934857,-8.98613737735134,-30.0570908269895));
#51301=CARTESIAN_POINT('',(380.681799934857,-10.4861373773513,0.820909173010471));
#51302=CARTESIAN_POINT('Origin',(391.564799934857,-8.98613737735134,-30.0570908269895));
#51303=CARTESIAN_POINT('',(339.771799934857,-8.98613737735134,-25.1429698676036));
#51304=CARTESIAN_POINT('',(339.771799934857,-8.98613737735134,-30.0570908269895));
#51305=CARTESIAN_POINT('',(342.448997804234,-8.98613737735134,-21.7410591318785));
#51306=CARTESIAN_POINT('Origin',(343.271799934857,-8.98613737735134,-25.1429698676036));
#51307=CARTESIAN_POINT('',(361.330051062071,-8.98613737735134,1.21054870903725));
#51308=CARTESIAN_POINT('Origin',(336.6390287719,-8.98613737735134,2.28050728087887));
#51309=CARTESIAN_POINT('',(370.321612719089,-8.98613737735134,9.82090917301047));
#51310=CARTESIAN_POINT('Origin',(370.321612719089,-8.98613737735134,0.820909173010471));
#51311=CARTESIAN_POINT('',(371.681799934857,-8.98613737735134,9.82090917301047));
#51312=CARTESIAN_POINT('',(330.604799934857,-8.98613737735134,9.82090917301047));
#51313=CARTESIAN_POINT('Origin',(371.681799934857,-8.98613737735143,0.820909173010471));
#51314=CARTESIAN_POINT('',(366.389317853224,-8.98613737735134,0.));
#51315=CARTESIAN_POINT('Origin',(370.834317853224,-8.98613737735134,0.));
#51316=CARTESIAN_POINT('Origin',(345.844799934857,-11.4861373773513,-27.5570908269895));
#51317=CARTESIAN_POINT('',(339.771799934857,-11.4861373773513,-28.0570908269895));
#51318=CARTESIAN_POINT('Origin',(339.771799934857,-11.4861373773513,-27.5570908269895));
#51319=CARTESIAN_POINT('',(345.844799934857,-11.4861373773513,-28.0570908269895));
#51320=CARTESIAN_POINT('Origin',(343.271799934857,-10.9861373773513,-25.1429698676036));
#51321=CARTESIAN_POINT('',(339.771799934857,-10.9861373773513,-25.1429698676036));
#51322=CARTESIAN_POINT('',(342.448997804234,-10.9861373773513,-21.7410591318785));
#51323=CARTESIAN_POINT('Origin',(336.6390287719,-10.9861373773513,2.28050728087887));
#51324=CARTESIAN_POINT('',(361.330051062071,-10.9861373773513,1.21054870903726));
#51325=CARTESIAN_POINT('Origin',(371.681799934857,-10.4861373773514,0.820909173010471));
#51326=CARTESIAN_POINT('',(371.681799934857,-10.4861373773514,9.82090917301047));
#51327=CARTESIAN_POINT('Origin',(361.084799934857,-9.98613737735134,9.82090917301047));
#51328=CARTESIAN_POINT('',(370.321612719089,-10.9861373773513,9.82090917301047));
#51329=CARTESIAN_POINT('Origin',(370.321612719089,-10.9861373773513,0.820909173010471));
#51330=CARTESIAN_POINT('Origin',(370.834317853224,-10.9861373773513,0.));
#51331=CARTESIAN_POINT('',(366.389317853224,-10.9861373773513,5.44355502220999E-16));
#51332=CARTESIAN_POINT('Origin',(339.771799934857,-8.98613737735134,-30.0570908269895));
#51333=CARTESIAN_POINT('',(339.771799934857,-10.9861373773513,-28.0570908269895));
#51334=CARTESIAN_POINT('',(339.771799934857,-10.9861373773513,-30.0570908269895));
#51335=CARTESIAN_POINT('',(339.771799934857,-15.8361373773513,-28.0570908269895));
#51336=CARTESIAN_POINT('Origin',(339.301914228765,-26.9411392547891,-30.0570908269895));
#51337=CARTESIAN_POINT('',(334.856914228765,-26.9411392547891,-30.0570908269895));
#51338=CARTESIAN_POINT('Origin',(339.301914228765,-26.9411392547891,-30.0570908269895));
#51339=CARTESIAN_POINT('',(334.856914228765,-26.9411392547891,-28.0570908269895));
#51340=CARTESIAN_POINT('',(334.856914228765,-26.9411392547891,-30.0570908269895));
#51341=CARTESIAN_POINT('Origin',(339.301914228765,-26.9411392547891,-28.0570908269895));
#51342=CARTESIAN_POINT('Origin',(387.676491751218,-26.4627140227474,-30.0570908269895));
#51343=CARTESIAN_POINT('',(387.676491751218,-26.4627140227474,-30.0570908269895));
#51344=CARTESIAN_POINT('',(387.676491751218,-27.3527140227474,-30.0570908269895));
#51345=CARTESIAN_POINT('',(387.676491751218,-26.4627140227474,-30.0570908269895));
#51346=CARTESIAN_POINT('',(387.676491751218,-27.3527140227474,-28.0570908269895));
#51347=CARTESIAN_POINT('',(387.676491751218,-27.3527140227474,-30.0570908269895));
#51348=CARTESIAN_POINT('',(387.676491751218,-26.4627140227474,-28.0570908269895));
#51349=CARTESIAN_POINT('',(387.676491751218,-26.4627140227474,-28.0570908269895));
#51350=CARTESIAN_POINT('',(387.676491751218,-26.4627140227474,-30.0570908269895));
#51351=CARTESIAN_POINT('Origin',(383.676491751218,-26.4627140227474,-30.0570908269895));
#51352=CARTESIAN_POINT('',(383.676491751218,-22.4627140227474,-30.0570908269895));
#51353=CARTESIAN_POINT('Origin',(383.676491751218,-26.4627140227474,-30.0570908269895));
#51354=CARTESIAN_POINT('',(383.676491751218,-22.4627140227474,-28.0570908269895));
#51355=CARTESIAN_POINT('Origin',(383.676491751218,-26.4627140227474,-28.0570908269895));
#51356=CARTESIAN_POINT('',(383.676491751218,-22.4627140227474,-30.0570908269895));
#51357=CARTESIAN_POINT('Origin',(380.246491751218,-22.4627140227474,-30.0570908269895));
#51358=CARTESIAN_POINT('',(380.246491751218,-22.4627140227474,-30.0570908269895));
#51359=CARTESIAN_POINT('',(380.246491751218,-22.4627140227474,-30.0570908269895));
#51360=CARTESIAN_POINT('',(380.246491751218,-22.4627140227474,-28.0570908269895));
#51361=CARTESIAN_POINT('',(380.246491751218,-22.4627140227474,-28.0570908269895));
#51362=CARTESIAN_POINT('',(380.246491751218,-22.4627140227474,-30.0570908269895));
#51363=CARTESIAN_POINT('Origin',(380.246491751218,-26.4627140227474,-30.0570908269895));
#51364=CARTESIAN_POINT('',(376.246491751218,-26.4627140227474,-30.0570908269895));
#51365=CARTESIAN_POINT('Origin',(380.246491751218,-26.4627140227474,-30.0570908269895));
#51366=CARTESIAN_POINT('',(376.246491751218,-26.4627140227474,-28.0570908269895));
#51367=CARTESIAN_POINT('Origin',(380.246491751218,-26.4627140227474,-28.0570908269895));
#51368=CARTESIAN_POINT('',(376.246491751218,-26.4627140227474,-30.0570908269895));
#51369=CARTESIAN_POINT('Origin',(376.246491751218,-27.3527140227474,-30.0570908269895));
#51370=CARTESIAN_POINT('',(376.246491751218,-27.3527140227474,-30.0570908269895));
#51371=CARTESIAN_POINT('',(376.246491751218,-27.3527140227474,-30.0570908269895));
#51372=CARTESIAN_POINT('',(376.246491751218,-27.3527140227474,-28.0570908269895));
#51373=CARTESIAN_POINT('',(376.246491751218,-27.3527140227474,-28.0570908269895));
#51374=CARTESIAN_POINT('',(376.246491751218,-27.3527140227474,-30.0570908269895));
#51375=CARTESIAN_POINT('Origin',(380.246491751218,-27.3527140227474,-30.0570908269895));
#51376=CARTESIAN_POINT('',(380.246491751218,-31.3527140227474,-30.0570908269895));
#51377=CARTESIAN_POINT('Origin',(380.246491751218,-27.3527140227474,-30.0570908269895));
#51378=CARTESIAN_POINT('',(380.246491751218,-31.3527140227474,-28.0570908269895));
#51379=CARTESIAN_POINT('Origin',(380.246491751218,-27.3527140227474,-28.0570908269895));
#51380=CARTESIAN_POINT('',(380.246491751218,-31.3527140227474,-30.0570908269895));
#51381=CARTESIAN_POINT('Origin',(383.676491751218,-31.3527140227474,-30.0570908269895));
#51382=CARTESIAN_POINT('',(383.676491751218,-31.3527140227474,-30.0570908269895));
#51383=CARTESIAN_POINT('',(383.676491751218,-31.3527140227474,-30.0570908269895));
#51384=CARTESIAN_POINT('',(383.676491751218,-31.3527140227474,-28.0570908269895));
#51385=CARTESIAN_POINT('',(383.676491751218,-31.3527140227474,-28.0570908269895));
#51386=CARTESIAN_POINT('',(383.676491751218,-31.3527140227474,-30.0570908269895));
#51387=CARTESIAN_POINT('Origin',(383.676491751218,-27.3527140227474,-30.0570908269895));
#51388=CARTESIAN_POINT('Origin',(383.676491751218,-27.3527140227474,-30.0570908269895));
#51389=CARTESIAN_POINT('Origin',(383.676491751218,-27.3527140227474,-28.0570908269895));
#51390=CARTESIAN_POINT('Origin',(337.604799934857,-25.8442305588067,-30.0570908269895));
#51391=CARTESIAN_POINT('',(335.409111459553,-19.197505642021,-30.0570908269895));
#51392=CARTESIAN_POINT('',(330.604799934857,-25.8442305588067,-30.0570908269895));
#51393=CARTESIAN_POINT('Origin',(337.604799934857,-25.8442305588067,-30.0570908269895));
#51394=CARTESIAN_POINT('',(330.604799934857,-25.8442305588067,-28.0570908269895));
#51395=CARTESIAN_POINT('',(330.604799934857,-25.8442305588067,-30.0570908269895));
#51396=CARTESIAN_POINT('',(335.409111459553,-19.197505642021,-28.0570908269895));
#51397=CARTESIAN_POINT('Origin',(337.604799934857,-25.8442305588067,-28.0570908269895));
#51398=CARTESIAN_POINT('',(335.409111459553,-19.197505642021,-30.0570908269895));
#51399=CARTESIAN_POINT('Origin',(329.862016215124,-10.9861373773514,-30.0570908269895));
#51400=CARTESIAN_POINT('Origin',(329.862016215124,-10.9861373773514,-30.0570908269895));
#51401=CARTESIAN_POINT('Origin',(329.862016215124,-10.9861373773514,-28.0570908269895));
#51402=CARTESIAN_POINT('Origin',(385.681635380396,-15.0708658676184,-30.0570908269895));
#51403=CARTESIAN_POINT('',(385.681635380396,-20.0708658676184,-30.0570908269895));
#51404=CARTESIAN_POINT('Origin',(385.681635380396,-15.0708658676184,-30.0570908269895));
#51405=CARTESIAN_POINT('',(385.681635380396,-20.0708658676184,-28.0570908269895));
#51406=CARTESIAN_POINT('Origin',(385.681635380396,-15.0708658676184,-28.0570908269895));
#51407=CARTESIAN_POINT('',(385.681635380396,-20.0708658676184,-30.0570908269895));
#51408=CARTESIAN_POINT('Origin',(385.564799934857,-20.0708658676184,-30.0570908269895));
#51409=CARTESIAN_POINT('',(385.564799934857,-20.0708658676184,-30.0570908269895));
#51410=CARTESIAN_POINT('',(385.564799934857,-20.0708658676184,-30.0570908269895));
#51411=CARTESIAN_POINT('',(385.564799934857,-20.0708658676184,-28.0570908269895));
#51412=CARTESIAN_POINT('',(385.564799934857,-20.0708658676184,-28.0570908269895));
#51413=CARTESIAN_POINT('',(385.564799934857,-20.0708658676184,-30.0570908269895));
#51414=CARTESIAN_POINT('Origin',(385.564799934857,-26.0708658676183,-30.0570908269895));
#51415=CARTESIAN_POINT('',(391.564799934857,-26.0708658676183,-30.0570908269895));
#51416=CARTESIAN_POINT('Origin',(385.564799934857,-26.0708658676183,-30.0570908269895));
#51417=CARTESIAN_POINT('',(391.564799934857,-26.0708658676183,-28.0570908269895));
#51418=CARTESIAN_POINT('Origin',(385.564799934857,-26.0708658676183,-28.0570908269895));
#51419=CARTESIAN_POINT('',(391.564799934857,-26.0708658676183,-30.0570908269895));
#51420=CARTESIAN_POINT('Origin',(391.564799934857,-28.3861373773513,-30.0570908269895));
#51421=CARTESIAN_POINT('',(391.564799934857,-28.3861373773513,-30.0570908269895));
#51422=CARTESIAN_POINT('',(391.564799934857,-34.3861373773513,-30.0570908269895));
#51423=CARTESIAN_POINT('',(391.564799934857,-28.3861373773513,-28.0570908269895));
#51424=CARTESIAN_POINT('',(391.564799934857,-34.3861373773513,-28.0570908269895));
#51425=CARTESIAN_POINT('',(391.564799934857,-28.3861373773513,-30.0570908269895));
#51426=CARTESIAN_POINT('Origin',(385.564799934857,-28.3861373773514,-30.0570908269895));
#51427=CARTESIAN_POINT('',(385.564799934857,-34.3861373773513,-30.0570908269895));
#51428=CARTESIAN_POINT('Origin',(385.564799934857,-28.3861373773514,-30.0570908269895));
#51429=CARTESIAN_POINT('',(385.564799934857,-34.3861373773513,-28.0570908269895));
#51430=CARTESIAN_POINT('Origin',(385.564799934857,-28.3861373773514,-28.0570908269895));
#51431=CARTESIAN_POINT('',(385.564799934857,-34.3861373773513,-30.0570908269895));
#51432=CARTESIAN_POINT('Origin',(337.604799934857,-34.3861373773513,-30.0570908269895));
#51433=CARTESIAN_POINT('',(337.604799934857,-34.3861373773513,-30.0570908269895));
#51434=CARTESIAN_POINT('',(330.604799934857,-34.3861373773513,-30.0570908269895));
#51435=CARTESIAN_POINT('',(337.604799934857,-34.3861373773513,-28.0570908269895));
#51436=CARTESIAN_POINT('',(330.604799934857,-34.3861373773513,-28.0570908269895));
#51437=CARTESIAN_POINT('',(337.604799934857,-34.3861373773513,-30.0570908269895));
#51438=CARTESIAN_POINT('Origin',(337.604799934857,-27.3861373773513,-30.0570908269895));
#51439=CARTESIAN_POINT('',(330.604799934857,-27.3861373773513,-30.0570908269895));
#51440=CARTESIAN_POINT('Origin',(337.604799934857,-27.3861373773513,-30.0570908269895));
#51441=CARTESIAN_POINT('',(330.604799934857,-27.3861373773513,-28.0570908269895));
#51442=CARTESIAN_POINT('Origin',(337.604799934857,-27.3861373773513,-28.0570908269895));
#51443=CARTESIAN_POINT('',(330.604799934857,-27.3861373773513,-30.0570908269895));
#51444=CARTESIAN_POINT('Origin',(330.604799934857,-25.8442305588067,-30.0570908269895));
#51445=CARTESIAN_POINT('',(330.604799934857,-25.8442305588067,-30.0570908269895));
#51446=CARTESIAN_POINT('',(330.604799934857,-25.8442305588067,-28.0570908269895));
#51447=CARTESIAN_POINT('Origin',(361.084799934857,-22.6861373773513,-28.0570908269895));
#51448=CARTESIAN_POINT('Origin',(361.084799934857,-22.6861373773513,-30.0570908269895));
#51449=CARTESIAN_POINT('',(0.,0.,0.));
#51450=CARTESIAN_POINT('Origin',(6.37917532067789,0.,0.));
#51451=CARTESIAN_POINT('',(6.37917532067789,-4.06856249956639,2.90633776205073));
#51452=CARTESIAN_POINT('',(6.37917532067789,-4.06856249956639,9.03402352829016E-16));
#51453=CARTESIAN_POINT('',(6.37917532067789,-4.06856249956639,9.03402352829016E-16));
#51454=CARTESIAN_POINT('',(6.37917532067789,-5.,6.12323399573677E-16));
#51455=CARTESIAN_POINT('Origin',(6.37917532067789,0.,0.));
#51456=CARTESIAN_POINT('',(6.37917532067789,4.06856249956639,2.90633776205073));
#51457=CARTESIAN_POINT('Origin',(6.37917532067789,0.,0.));
#51458=CARTESIAN_POINT('',(6.37917532067789,4.06856249956639,-9.03402352829016E-16));
#51459=CARTESIAN_POINT('',(6.37917532067789,4.06856249956639,-9.03402352829016E-16));
#51460=CARTESIAN_POINT('',(6.37917532067789,0.,0.));
#51461=CARTESIAN_POINT('Origin',(206.833344075386,0.,0.));
#51462=CARTESIAN_POINT('',(24.6022815711059,-5.,6.12323399573677E-16));
#51463=CARTESIAN_POINT('Origin',(24.6022815711059,0.,0.));
#51464=CARTESIAN_POINT('',(206.833344075386,-5.,6.12323399573677E-16));
#51465=CARTESIAN_POINT('',(8.95646910621821,8.6937196433654E-16,5.));
#51466=CARTESIAN_POINT('Ctrl Pts',(8.95646910621821,1.17961196366423E-15,
5.));
#51467=CARTESIAN_POINT('Ctrl Pts',(8.95646910621821,-0.606820989968836,
5.));
#51468=CARTESIAN_POINT('Ctrl Pts',(8.82673713165736,-1.22898791230303,4.88231525391355));
#51469=CARTESIAN_POINT('Ctrl Pts',(8.35235281675177,-2.33060974443834,4.46269756160066));
#51470=CARTESIAN_POINT('Ctrl Pts',(8.00907805487115,-2.81135208202597,4.16259123013233));
#51471=CARTESIAN_POINT('Ctrl Pts',(7.27957085481457,-3.54085928208256,3.56072689165552));
#51472=CARTESIAN_POINT('Ctrl Pts',(6.8497028394201,-3.84620234546864,3.21761823198537));
#51473=CARTESIAN_POINT('Ctrl Pts',(6.37917532067789,-4.06856249956639,2.90633776205073));
#51474=CARTESIAN_POINT('Ctrl Pts',(6.37917532067789,4.06856249956639,2.90633776205073));
#51475=CARTESIAN_POINT('Ctrl Pts',(6.84970283942009,3.84620234546864,3.21761823198536));
#51476=CARTESIAN_POINT('Ctrl Pts',(7.27957085481456,3.54085928208256,3.56072689165552));
#51477=CARTESIAN_POINT('Ctrl Pts',(8.00907805487115,2.81135208202597,4.16259123013233));
#51478=CARTESIAN_POINT('Ctrl Pts',(8.35235281675177,2.33060974443835,4.46269756160066));
#51479=CARTESIAN_POINT('Ctrl Pts',(8.82673713165736,1.22898791230303,4.88231525391354));
#51480=CARTESIAN_POINT('Ctrl Pts',(8.95646910621821,0.60682098996884,5.));
#51481=CARTESIAN_POINT('Ctrl Pts',(8.95646910621821,8.32667268468867E-16,
5.));
#51482=CARTESIAN_POINT('Origin',(4.45646910621825,0.,0.));
#51483=CARTESIAN_POINT('Origin',(4.45646910621825,0.,0.));
#51484=CARTESIAN_POINT('Origin',(24.6022815711059,-5.62967641351579,1.25003927509488E-15));
#51485=CARTESIAN_POINT('',(24.6022815711059,5.62967641351579,-5.60602755090134E-16));
#51486=CARTESIAN_POINT('Origin',(24.6022815711059,0.,0.));
#51487=CARTESIAN_POINT('Origin',(4.45646910621825,0.,0.));
#51488=CARTESIAN_POINT('',(8.95646910621821,1.96909841056726E-15,6.38613737735135));
#51489=CARTESIAN_POINT('Origin',(4.45646910621825,1.41800735095096E-15,
6.38613737735135));
#51490=CARTESIAN_POINT('',(8.95646910621821,-5.51091059616304E-16,1.22366796610219E-31));
#51491=CARTESIAN_POINT('Origin',(17.2376725011568,0.,0.));
#51492=CARTESIAN_POINT('',(9.87306343120764,5.62967641351579,-5.60602755090133E-16));
#51493=CARTESIAN_POINT('',(17.2376725011568,5.62967641351579,-5.60602755090133E-16));
#51494=CARTESIAN_POINT('',(9.87306343120764,-5.60602755090134E-16,-5.62967641351579));
#51495=CARTESIAN_POINT('Origin',(9.87306343120764,0.,0.));
#51496=CARTESIAN_POINT('Origin',(9.87306343120764,0.,0.));
#51497=CARTESIAN_POINT('Origin',(4.45646910621825,0.,0.));
#51498=CARTESIAN_POINT('',(-3.35587693081848,-3.21444381174749E-32,7.67432839081512E-17));
#51499=CARTESIAN_POINT('Origin',(4.45646910621825,0.,0.));
#51500=CARTESIAN_POINT('Origin',(187.645393479721,0.,0.));
#51501=CARTESIAN_POINT('',(350.688505388337,6.07706845554618E-16,4.9623029756639));
#51502=CARTESIAN_POINT('Origin',(350.688505388337,0.,0.));
#51503=CARTESIAN_POINT('',(206.833344075386,-6.07706845554618E-16,4.9623029756639));
#51504=CARTESIAN_POINT('',(187.645393479721,-6.07706845554618E-16,4.9623029756639));
#51505=CARTESIAN_POINT('Origin',(206.833344075386,0.,0.));
#51506=CARTESIAN_POINT('Origin',(370.834317853224,0.,0.));
#51507=CARTESIAN_POINT('',(365.417723528235,5.62967641351579,6.89436520004747E-16));
#51508=CARTESIAN_POINT('',(365.417723528235,-6.89436520004746E-16,5.62967641351579));
#51509=CARTESIAN_POINT('Origin',(365.417723528235,0.,0.));
#51510=CARTESIAN_POINT('Origin',(365.417723528235,0.,0.));
#51511=CARTESIAN_POINT('',(378.646663890261,4.78368228404427E-16,1.17166423945854E-31));
#51512=CARTESIAN_POINT('Origin',(370.834317853224,0.,0.));
#51513=CARTESIAN_POINT('',(366.334317853224,-6.38613737735135,5.51091059616304E-16));
#51514=CARTESIAN_POINT('Origin',(370.834317853224,-6.38613737735135,0.));
#51515=CARTESIAN_POINT('Origin',(358.053114458286,0.,0.));
#51516=CARTESIAN_POINT('',(350.688505388337,-6.89436520004747E-16,5.62967641351579));
#51517=CARTESIAN_POINT('',(358.053114458286,-6.89436520004746E-16,5.62967641351579));
#51518=CARTESIAN_POINT('Origin',(350.688505388337,0.,0.));
#51519=CARTESIAN_POINT('Origin',(370.834317853224,0.,0.));
#51520=CARTESIAN_POINT('',(366.334317853224,0.,5.51091059616304E-16));
#51521=CARTESIAN_POINT('Origin',(370.834317853224,0.,0.));
#51522=CARTESIAN_POINT('Origin',(370.834317853224,0.,0.));
#51523=CARTESIAN_POINT('',(366.334317853224,0.,-5.51091059616304E-16));
#51524=CARTESIAN_POINT('Origin',(350.688505388337,0.,-5.62967641351579));
#51525=CARTESIAN_POINT('Origin',(206.833344075386,0.,0.));
#51526=CARTESIAN_POINT('',(0.,0.,0.));
#51527=CARTESIAN_POINT('',(0.,0.,0.));
#51528=CARTESIAN_POINT('',(0.,0.,0.));
#51529=CARTESIAN_POINT('',(0.,0.,0.));
#51530=CARTESIAN_POINT('',(0.,0.,0.));
#51531=CARTESIAN_POINT('',(0.,0.,0.));
#51532=CARTESIAN_POINT('',(0.,0.,0.));
#51533=CARTESIAN_POINT('',(0.,0.,0.));
#51534=UNCERTAINTY_MEASURE_WITH_UNIT(LENGTH_MEASURE(0.01),#51554,
'DISTANCE_ACCURACY_VALUE',
'Maximum model space distance between geometric entities at asserted c
onnectivities');
#51535=UNCERTAINTY_MEASURE_WITH_UNIT(LENGTH_MEASURE(0.01),#51554,
'DISTANCE_ACCURACY_VALUE',
'Maximum model space distance between geometric entities at asserted c
onnectivities');
#51536=UNCERTAINTY_MEASURE_WITH_UNIT(LENGTH_MEASURE(0.01),#51554,
'DISTANCE_ACCURACY_VALUE',
'Maximum model space distance between geometric entities at asserted c
onnectivities');
#51537=UNCERTAINTY_MEASURE_WITH_UNIT(LENGTH_MEASURE(0.01),#51554,
'DISTANCE_ACCURACY_VALUE',
'Maximum model space distance between geometric entities at asserted c
onnectivities');
#51538=UNCERTAINTY_MEASURE_WITH_UNIT(LENGTH_MEASURE(0.01),#51554,
'DISTANCE_ACCURACY_VALUE',
'Maximum model space distance between geometric entities at asserted c
onnectivities');
#51539=UNCERTAINTY_MEASURE_WITH_UNIT(LENGTH_MEASURE(0.01),#51554,
'DISTANCE_ACCURACY_VALUE',
'Maximum model space distance between geometric entities at asserted c
onnectivities');
#51540=UNCERTAINTY_MEASURE_WITH_UNIT(LENGTH_MEASURE(0.01),#51554,
'DISTANCE_ACCURACY_VALUE',
'Maximum model space distance between geometric entities at asserted c
onnectivities');
#51541=UNCERTAINTY_MEASURE_WITH_UNIT(LENGTH_MEASURE(0.01),#51554,
'DISTANCE_ACCURACY_VALUE',
'Maximum model space distance between geometric entities at asserted c
onnectivities');
#51542=UNCERTAINTY_MEASURE_WITH_UNIT(LENGTH_MEASURE(0.01),#51554,
'DISTANCE_ACCURACY_VALUE',
'Maximum model space distance between geometric entities at asserted c
onnectivities');
#51543=UNCERTAINTY_MEASURE_WITH_UNIT(LENGTH_MEASURE(0.01),#51554,
'DISTANCE_ACCURACY_VALUE',
'Maximum model space distance between geometric entities at asserted c
onnectivities');
#51544=(
GEOMETRIC_REPRESENTATION_CONTEXT(3)
GLOBAL_UNCERTAINTY_ASSIGNED_CONTEXT((#51534))
GLOBAL_UNIT_ASSIGNED_CONTEXT((#51554,#51556,#51557))
REPRESENTATION_CONTEXT('','3D')
);
#51545=(
GEOMETRIC_REPRESENTATION_CONTEXT(3)
GLOBAL_UNCERTAINTY_ASSIGNED_CONTEXT((#51535))
GLOBAL_UNIT_ASSIGNED_CONTEXT((#51554,#51556,#51557))
REPRESENTATION_CONTEXT('','3D')
);
#51546=(
GEOMETRIC_REPRESENTATION_CONTEXT(3)
GLOBAL_UNCERTAINTY_ASSIGNED_CONTEXT((#51536))
GLOBAL_UNIT_ASSIGNED_CONTEXT((#51554,#51556,#51557))
REPRESENTATION_CONTEXT('','3D')
);
#51547=(
GEOMETRIC_REPRESENTATION_CONTEXT(3)
GLOBAL_UNCERTAINTY_ASSIGNED_CONTEXT((#51537))
GLOBAL_UNIT_ASSIGNED_CONTEXT((#51554,#51556,#51557))
REPRESENTATION_CONTEXT('','3D')
);
#51548=(
GEOMETRIC_REPRESENTATION_CONTEXT(3)
GLOBAL_UNCERTAINTY_ASSIGNED_CONTEXT((#51538))
GLOBAL_UNIT_ASSIGNED_CONTEXT((#51554,#51556,#51557))
REPRESENTATION_CONTEXT('','3D')
);
#51549=(
GEOMETRIC_REPRESENTATION_CONTEXT(3)
GLOBAL_UNCERTAINTY_ASSIGNED_CONTEXT((#51539))
GLOBAL_UNIT_ASSIGNED_CONTEXT((#51554,#51556,#51557))
REPRESENTATION_CONTEXT('','3D')
);
#51550=(
GEOMETRIC_REPRESENTATION_CONTEXT(3)
GLOBAL_UNCERTAINTY_ASSIGNED_CONTEXT((#51540))
GLOBAL_UNIT_ASSIGNED_CONTEXT((#51554,#51556,#51557))
REPRESENTATION_CONTEXT('','3D')
);
#51551=(
GEOMETRIC_REPRESENTATION_CONTEXT(3)
GLOBAL_UNCERTAINTY_ASSIGNED_CONTEXT((#51541))
GLOBAL_UNIT_ASSIGNED_CONTEXT((#51554,#51556,#51557))
REPRESENTATION_CONTEXT('','3D')
);
#51552=(
GEOMETRIC_REPRESENTATION_CONTEXT(3)
GLOBAL_UNCERTAINTY_ASSIGNED_CONTEXT((#51542))
GLOBAL_UNIT_ASSIGNED_CONTEXT((#51554,#51556,#51557))
REPRESENTATION_CONTEXT('','3D')
);
#51553=(
GEOMETRIC_REPRESENTATION_CONTEXT(3)
GLOBAL_UNCERTAINTY_ASSIGNED_CONTEXT((#51543))
GLOBAL_UNIT_ASSIGNED_CONTEXT((#51554,#51556,#51557))
REPRESENTATION_CONTEXT('','3D')
);
#51554=(
LENGTH_UNIT()
NAMED_UNIT(*)
SI_UNIT(.MILLI.,.METRE.)
);
#51555=(
LENGTH_UNIT()
NAMED_UNIT(*)
SI_UNIT($,.METRE.)
);
#51556=(
NAMED_UNIT(*)
PLANE_ANGLE_UNIT()
SI_UNIT($,.RADIAN.)
);
#51557=(
NAMED_UNIT(*)
SI_UNIT($,.STERADIAN.)
SOLID_ANGLE_UNIT()
);
#51558=SHAPE_DEFINITION_REPRESENTATION(#51567,#51584);
#51559=SHAPE_DEFINITION_REPRESENTATION(#51568,#51585);
#51560=SHAPE_DEFINITION_REPRESENTATION(#51569,#51586);
#51561=SHAPE_DEFINITION_REPRESENTATION(#51570,#51587);
#51562=SHAPE_DEFINITION_REPRESENTATION(#51571,#51588);
#51563=SHAPE_DEFINITION_REPRESENTATION(#51572,#51589);
#51564=SHAPE_DEFINITION_REPRESENTATION(#51573,#51590);
#51565=SHAPE_DEFINITION_REPRESENTATION(#51574,#51591);
#51566=SHAPE_DEFINITION_REPRESENTATION(#51575,#51592);
#51567=PRODUCT_DEFINITION_SHAPE('',$,#51594);
#51568=PRODUCT_DEFINITION_SHAPE('',$,#51595);
#51569=PRODUCT_DEFINITION_SHAPE('',$,#51596);
#51570=PRODUCT_DEFINITION_SHAPE('',$,#51597);
#51571=PRODUCT_DEFINITION_SHAPE('',$,#51598);
#51572=PRODUCT_DEFINITION_SHAPE('',$,#51599);
#51573=PRODUCT_DEFINITION_SHAPE('',$,#51600);
#51574=PRODUCT_DEFINITION_SHAPE('',$,#51601);
#51575=PRODUCT_DEFINITION_SHAPE('',$,#51602);
#51576=PRODUCT_DEFINITION_SHAPE($,$,#35);
#51577=PRODUCT_DEFINITION_SHAPE($,$,#36);
#51578=PRODUCT_DEFINITION_SHAPE($,$,#37);
#51579=PRODUCT_DEFINITION_SHAPE($,$,#38);
#51580=PRODUCT_DEFINITION_SHAPE($,$,#39);
#51581=PRODUCT_DEFINITION_SHAPE($,$,#40);
#51582=PRODUCT_DEFINITION_SHAPE($,$,#41);
#51583=PRODUCT_DEFINITION_SHAPE($,$,#42);
#51584=SHAPE_REPRESENTATION('',(#4357,#4663,#4664,#4665,#4666,#4667,#4668,
#4669,#4670),#51544);
#51585=SHAPE_REPRESENTATION('',(#4358),#51545);
#51586=SHAPE_REPRESENTATION('',(#4430),#51546);
#51587=SHAPE_REPRESENTATION('',(#4466),#51547);
#51588=SHAPE_REPRESENTATION('',(#4489),#51548);
#51589=SHAPE_REPRESENTATION('',(#4507),#51549);
#51590=SHAPE_REPRESENTATION('',(#4530),#51550);
#51591=SHAPE_REPRESENTATION('',(#4559),#51551);
#51592=SHAPE_REPRESENTATION('',(#4631),#51552);
#51593=PRODUCT_DEFINITION_CONTEXT('part definition',#51622,'design');
#51594=PRODUCT_DEFINITION('BR-107','BR-107',#51603,#51593);
#51595=PRODUCT_DEFINITION('Clamp_01','Clamp_01',#51604,#51593);
#51596=PRODUCT_DEFINITION('Screw_01','Screw_01',#51605,#51593);
#51597=PRODUCT_DEFINITION('Nut_02','Nut_02',#51606,#51593);
#51598=PRODUCT_DEFINITION('Spring_part','Spring_part',#51607,#51593);
#51599=PRODUCT_DEFINITION('Nut_01','Nut_01',#51608,#51593);
#51600=PRODUCT_DEFINITION('Screw_02','Screw_02',#51609,#51593);
#51601=PRODUCT_DEFINITION('Clamp_02','Clamp_02',#51610,#51593);
#51602=PRODUCT_DEFINITION('Rod','Rod',#51611,#51593);
#51603=PRODUCT_DEFINITION_FORMATION('',$,#51624);
#51604=PRODUCT_DEFINITION_FORMATION('',$,#51625);
#51605=PRODUCT_DEFINITION_FORMATION('',$,#51626);
#51606=PRODUCT_DEFINITION_FORMATION('',$,#51627);
#51607=PRODUCT_DEFINITION_FORMATION('',$,#51628);
#51608=PRODUCT_DEFINITION_FORMATION('',$,#51629);
#51609=PRODUCT_DEFINITION_FORMATION('',$,#51630);
#51610=PRODUCT_DEFINITION_FORMATION('',$,#51631);
#51611=PRODUCT_DEFINITION_FORMATION('',$,#51632);
#51612=PRODUCT_RELATED_PRODUCT_CATEGORY('BR-107','BR-107',(#51624));
#51613=PRODUCT_RELATED_PRODUCT_CATEGORY('Clamp_01','Clamp_01',(#51625));
#51614=PRODUCT_RELATED_PRODUCT_CATEGORY('Screw_01','Screw_01',(#51626));
#51615=PRODUCT_RELATED_PRODUCT_CATEGORY('Nut_02','Nut_02',(#51627));
#51616=PRODUCT_RELATED_PRODUCT_CATEGORY('Spring_part','Spring_part',(#51628));
#51617=PRODUCT_RELATED_PRODUCT_CATEGORY('Nut_01','Nut_01',(#51629));
#51618=PRODUCT_RELATED_PRODUCT_CATEGORY('Screw_02','Screw_02',(#51630));
#51619=PRODUCT_RELATED_PRODUCT_CATEGORY('Clamp_02','Clamp_02',(#51631));
#51620=PRODUCT_RELATED_PRODUCT_CATEGORY('Rod','Rod',(#51632));
#51621=APPLICATION_PROTOCOL_DEFINITION('international standard',
'automotive_design',2009,#51622);
#51622=APPLICATION_CONTEXT(
'Core Data for Automotive Mechanical Design Process');
#51623=PRODUCT_CONTEXT('part definition',#51622,'mechanical');
#51624=PRODUCT('BR-107','BR-107',$,(#51623));
#51625=PRODUCT('Clamp_01','Clamp_01',$,(#51623));
#51626=PRODUCT('Screw_01','Screw_01',$,(#51623));
#51627=PRODUCT('Nut_02','Nut_02',$,(#51623));
#51628=PRODUCT('Spring_part','Spring_part',$,(#51623));
#51629=PRODUCT('Nut_01','Nut_01',$,(#51623));
#51630=PRODUCT('Screw_02','Screw_02',$,(#51623));
#51631=PRODUCT('Clamp_02','Clamp_02',$,(#51623));
#51632=PRODUCT('Rod','Rod',$,(#51623));
#51633=PRESENTATION_STYLE_ASSIGNMENT((#51636));
#51634=PRESENTATION_STYLE_ASSIGNMENT((#51637));
#51635=PRESENTATION_STYLE_ASSIGNMENT((#51638));
#51636=SURFACE_STYLE_USAGE(.BOTH.,#51639);
#51637=SURFACE_STYLE_USAGE(.BOTH.,#51640);
#51638=SURFACE_STYLE_USAGE(.BOTH.,#51641);
#51639=SURFACE_SIDE_STYLE('',(#51642));
#51640=SURFACE_SIDE_STYLE('',(#51643));
#51641=SURFACE_SIDE_STYLE('',(#51644));
#51642=SURFACE_STYLE_FILL_AREA(#51645);
#51643=SURFACE_STYLE_FILL_AREA(#51646);
#51644=SURFACE_STYLE_FILL_AREA(#51647);
#51645=FILL_AREA_STYLE('Steel - Satin',(#51648));
#51646=FILL_AREA_STYLE('Opaque(203,203,203)',(#51649));
#51647=FILL_AREA_STYLE('Opaque(60,60,60)',(#51650));
#51648=FILL_AREA_STYLE_COLOUR('Steel - Satin',#51651);
#51649=FILL_AREA_STYLE_COLOUR('Opaque(203,203,203)',#51652);
#51650=FILL_AREA_STYLE_COLOUR('Opaque(60,60,60)',#51653);
#51651=COLOUR_RGB('Steel - Satin', 0.09019608, 0.27058824, 0.51372549);
#51652=COLOUR_RGB('Opaque(203,203,203)', 0.09019608, 0.27058824, 0.51372549);
#51653=COLOUR_RGB('Opaque(60,60,60)', 0.40784314, 0.44705882, 0.49803922);
ENDSEC;
END-ISO-10303-21;
